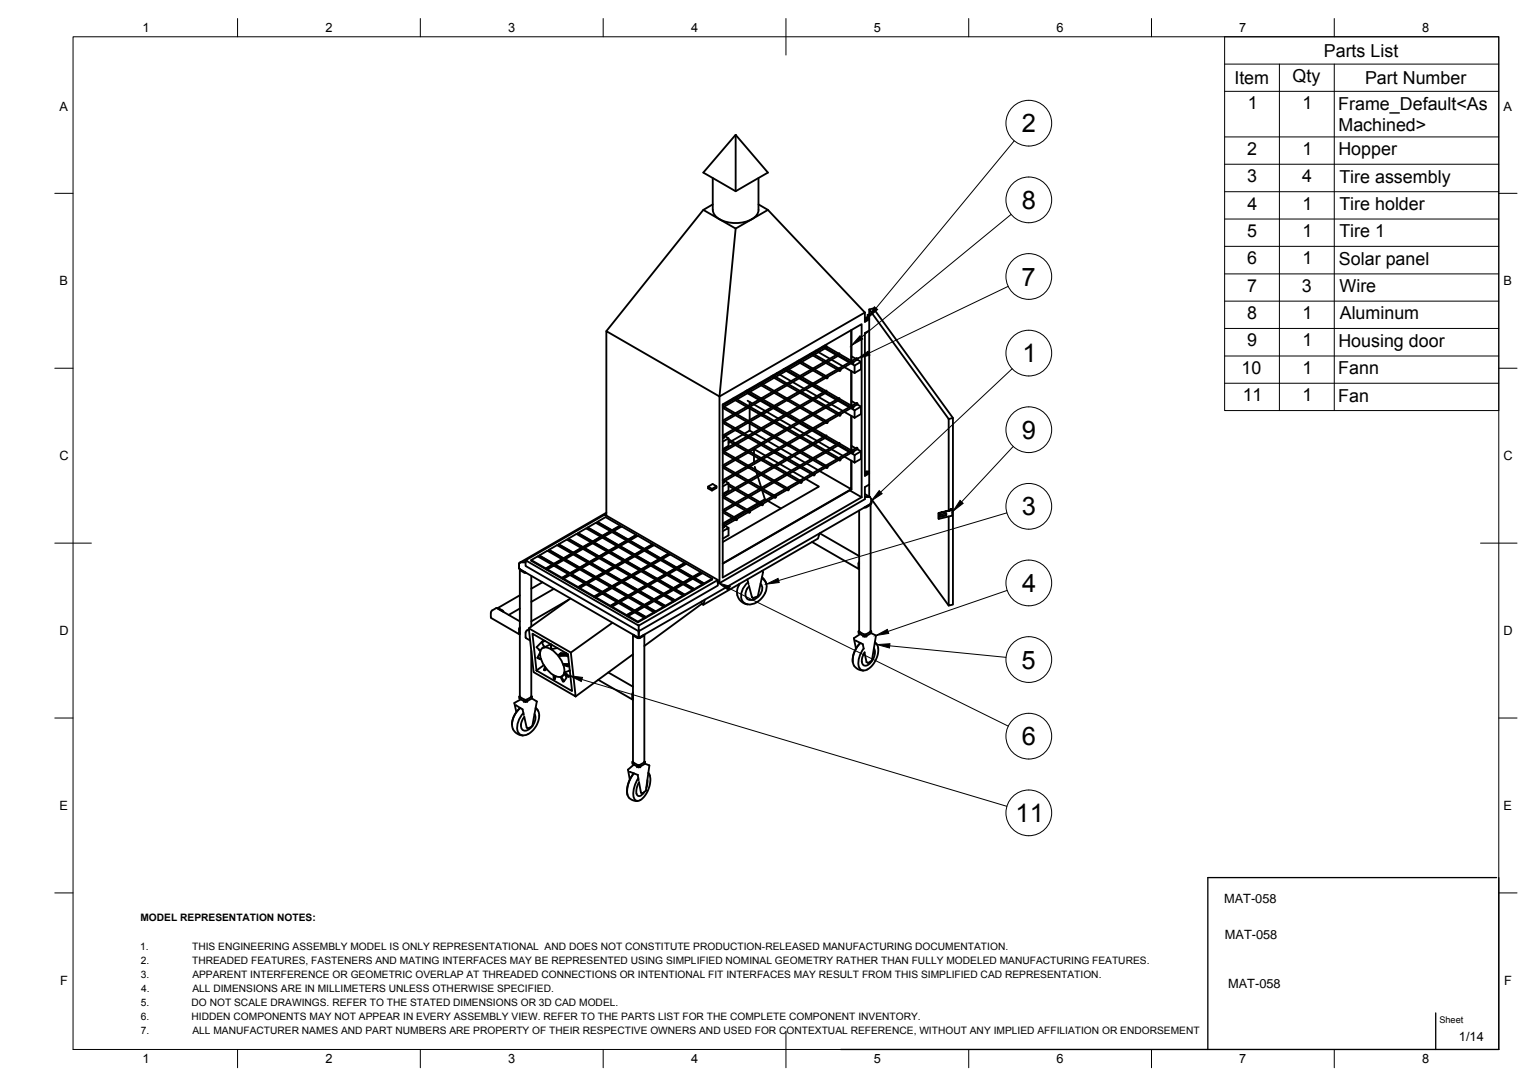
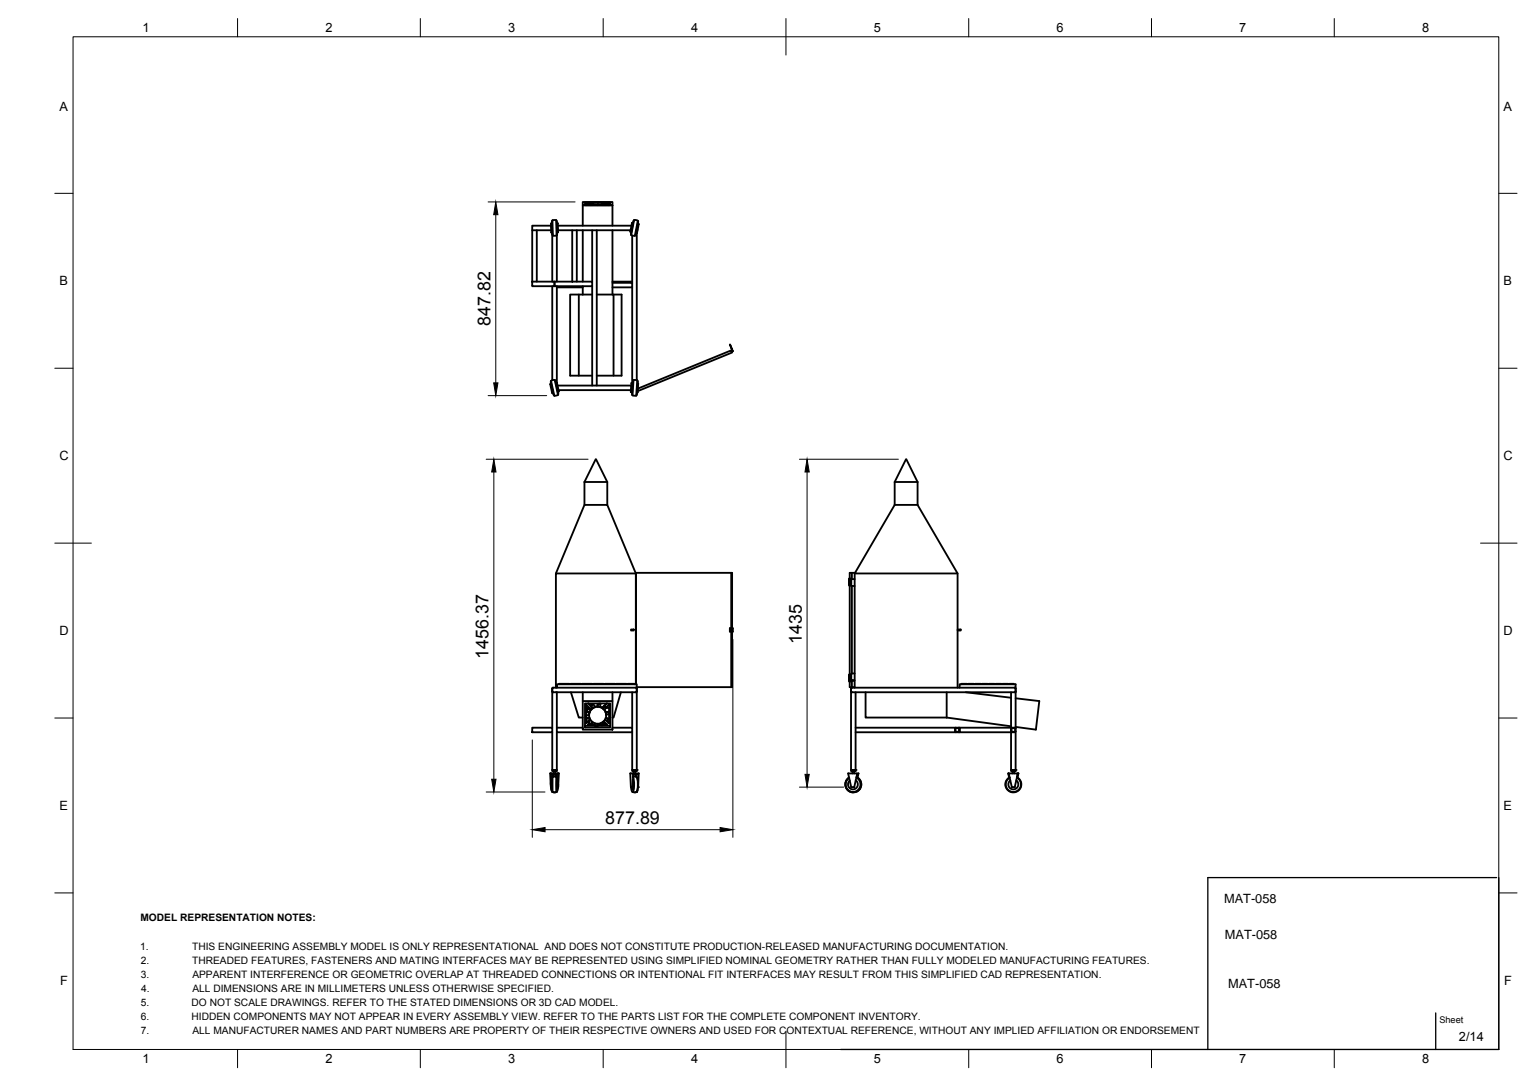
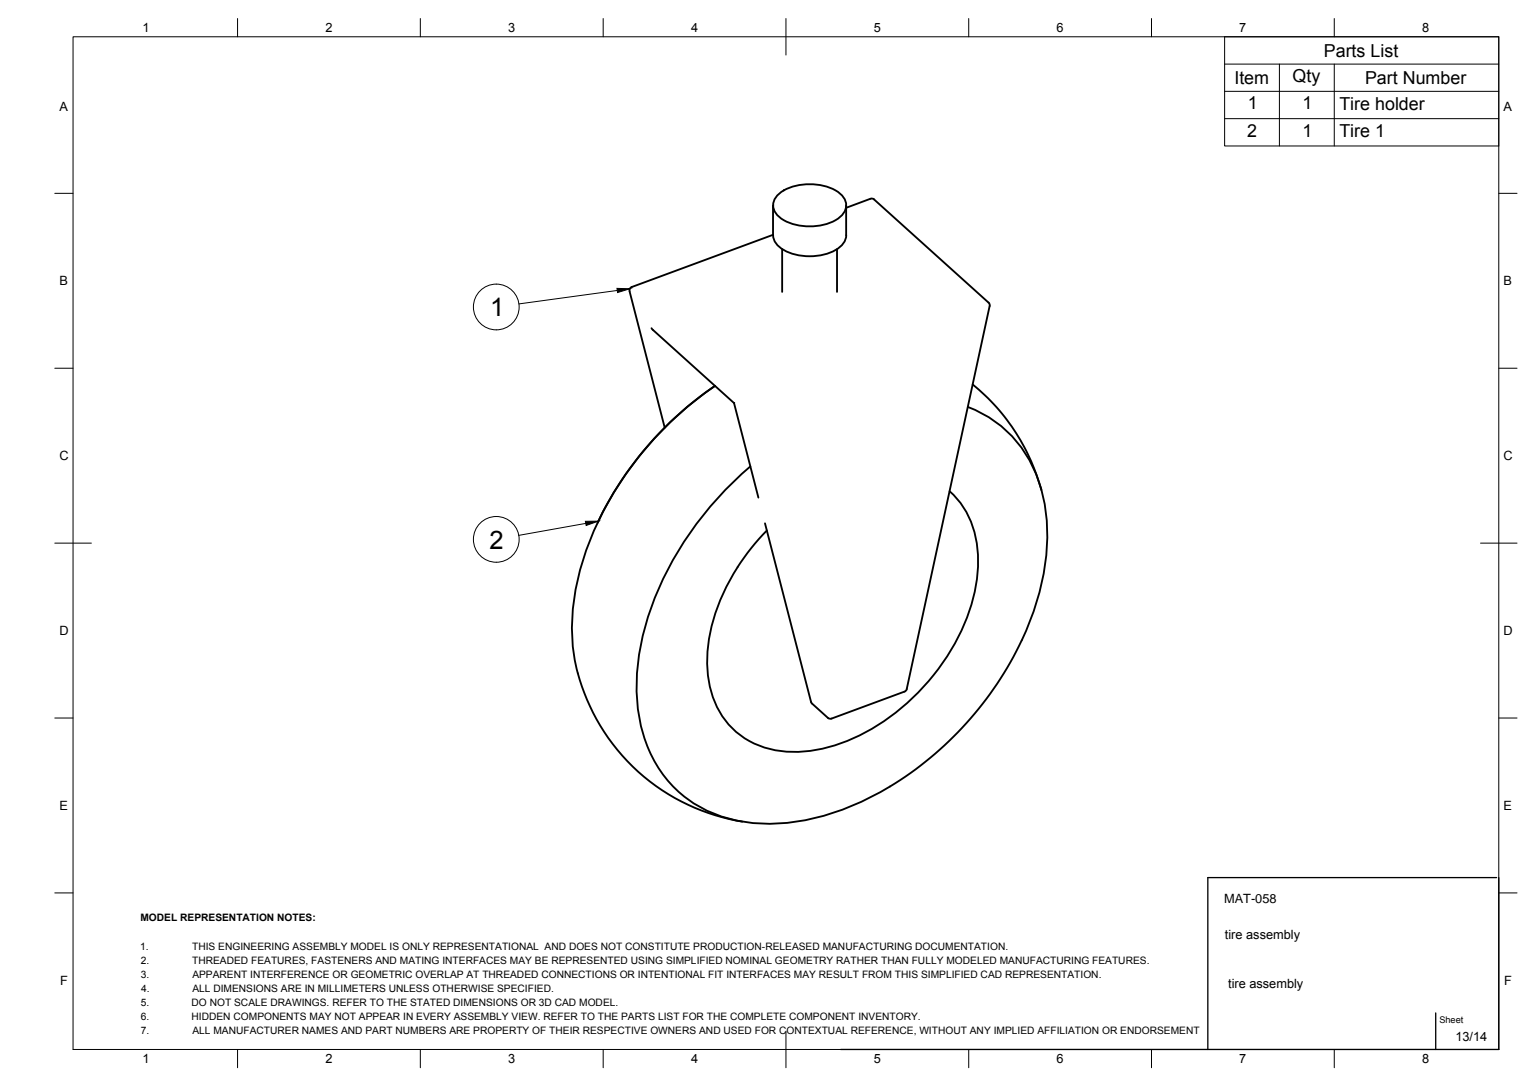
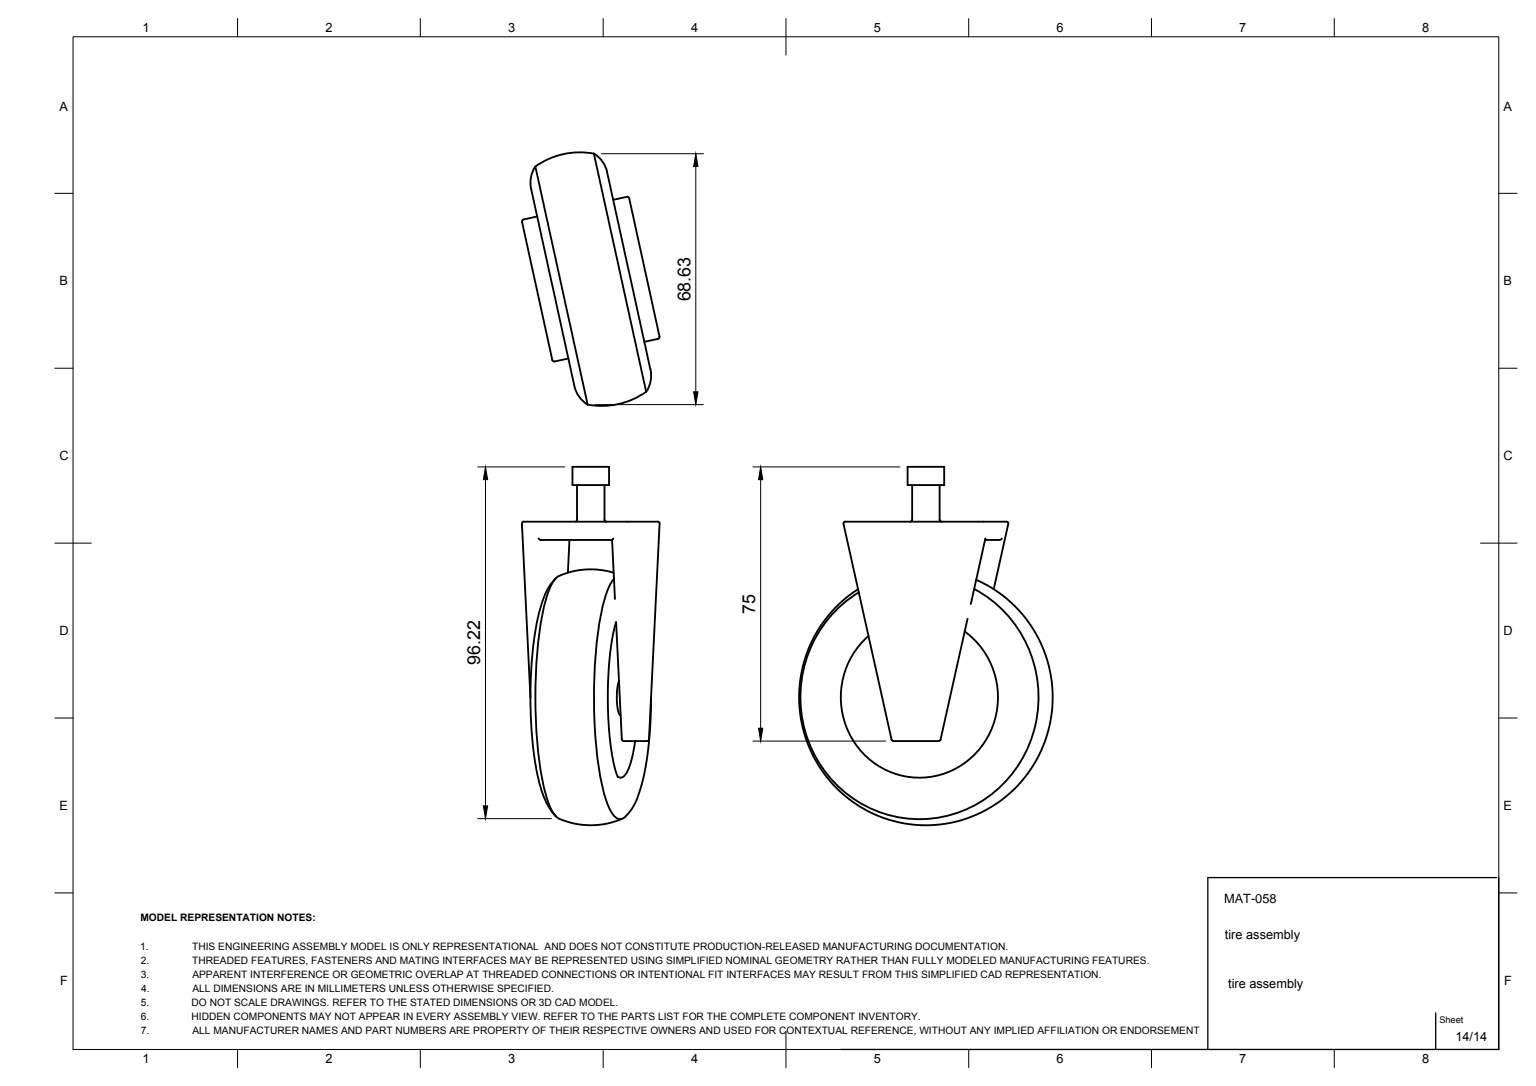
ISO-10303-21;
HEADER;
FILE_DESCRIPTION (('STEP AP214'),
    '1' );
FILE_NAME ('MAT-058',
    '2026-10-21T17:54:40',
    ( '' ),
    ( '' ),
    'SwSTEP 2.0',
    'SolidWorks 2026',
    '' );
FILE_SCHEMA (( 'AUTOMOTIVE_DESIGN' ));
ENDSEC;

DATA;
#1 = CARTESIAN_POINT ( 'NONE',  ( -0.3862712429686977478, 1.188820645368937390, -10.00000000000000000 ) ) ;
#2 = CIRCLE ( 'NONE', #7396, 2.000000000000001776 ) ;
#3 = ORIENTED_EDGE ( 'NONE', *, *, #134, .T. ) ;
#4 = FACE_OUTER_BOUND ( 'NONE', #5138, .T. ) ;
#5 = ORIENTED_EDGE ( 'NONE', *, *, #50322, .T. ) ;
#6 = ADVANCED_FACE ( 'NONE', ( #30321 ), #29814, .T. ) ;
#7 = ORIENTED_EDGE ( 'NONE', *, *, #34701, .F. ) ;
#8 = CARTESIAN_POINT ( 'NONE',  ( 341.9999999999999432, -181.0000000000001421, -349.9999999999998863 ) ) ;
#9 = DIRECTION ( 'NONE',  ( -1.000000000000000000, -0.000000000000000000, -0.000000000000000000 ) ) ;
#10 = ORIENTED_EDGE ( 'NONE', *, *, #50701, .F. ) ;
#11 = ORIENTED_EDGE ( 'NONE', *, *, #36636, .F. ) ;
#12 = EDGE_CURVE ( 'NONE', #49361, #27194, #1364, .T. ) ;
#13 = EDGE_CURVE ( 'NONE', #17667, #14780, #49006, .T. ) ;
#14 = ORIENTED_EDGE ( 'NONE', *, *, #5906, .T. ) ;
#15 = CARTESIAN_POINT ( 'NONE',  ( 71.55402655318505367, 1.025126265847089657, 79.06828755692797017 ) ) ;
#16 = DIRECTION ( 'NONE',  ( -1.000000000000000000, -0.000000000000000000, -0.000000000000000000 ) ) ;
#17 = ORIENTED_EDGE ( 'NONE', *, *, #15192, .T. ) ;
#18 = CARTESIAN_POINT ( 'NONE',  ( -1.011271242968683426, -0.7347315653655928092, 3.333333333333333481 ) ) ;
#19 = CARTESIAN_POINT ( 'NONE',  ( 42.78107912161490844, -16.56908454419397003, -9.367992836599951190 ) ) ;
#20 = EDGE_CURVE ( 'NONE', #23493, #39659, #10554, .T. ) ;
#21 = CARTESIAN_POINT ( 'NONE',  ( 191.5540265531851105, 0.000000000000000000, 162.5682875569279702 ) ) ;
#22 = ORIENTED_EDGE ( 'NONE', *, *, #35505, .T. ) ;
#23 = B_SPLINE_CURVE_WITH_KNOTS ( 'NONE', 3,
 ( #8249, #22875, #15684, #35464 ),
 .UNSPECIFIED., .F., .F.,
 ( 4, 4 ),
 ( 0.9895749839358303213, 1.000000000000000000 ),
 .UNSPECIFIED. ) ;
#24 = AXIS2_PLACEMENT_3D ( 'NONE', #27397, #19697, #35376 ) ;
#25 = FACE_OUTER_BOUND ( 'NONE', #19071, .T. ) ;
#26 = AXIS2_PLACEMENT_3D ( 'NONE', #26313, #42956, #39141 ) ;
#27 = VECTOR ( 'NONE', #2447, 1000.000000000000000 ) ;
#28 = EDGE_LOOP ( 'NONE', ( #27721, #41383, #11208, #21958 ) ) ;
#29 = CARTESIAN_POINT ( 'NONE',  ( 155.0540265531850537, 2.143131898507880377E-16, -37.43171244307205825 ) ) ;
#30 = DIRECTION ( 'NONE',  ( 0.000000000000000000, 0.000000000000000000, 1.000000000000000000 ) ) ;
#31 = ORIENTED_EDGE ( 'NONE', *, *, #39072, .F. ) ;
#32 = CARTESIAN_POINT ( 'NONE',  ( -24.39427009666018265, -44.07992421011638129, 8.807470649214879543 ) ) ;
#33 = VECTOR ( 'NONE', #35078, 1000.000000000000000 ) ;
#34 = AXIS2_PLACEMENT_3D ( 'NONE', #550, #47684, #4384 ) ;
#35 = CARTESIAN_POINT ( 'NONE',  ( 181.0000000000000284, -174.9999999999999716, -111.0000000000001563 ) ) ;
#36 = VERTEX_POINT ( 'NONE', #37038 ) ;
#37 = CARTESIAN_POINT ( 'NONE',  ( 38.06347959788622859, -17.13191708601470964, -8.080361901872240793 ) ) ;
#38 = FACE_OUTER_BOUND ( 'NONE', #34200, .T. ) ;
#39 = CARTESIAN_POINT ( 'NONE',  ( -48.44597344681495343, 0.000000000000000000, 159.0682875569279702 ) ) ;
#40 = VECTOR ( 'NONE', #48975, 1000.000000000000000 ) ;
#41 = DIRECTION ( 'NONE',  ( -1.000000000000000000, -0.000000000000000000, -0.000000000000000000 ) ) ;
#42 = EDGE_LOOP ( 'NONE', ( #31144, #13391, #8793, #47116, #38295 ) ) ;
#43 = FACE_OUTER_BOUND ( 'NONE', #38714, .T. ) ;
#44 = CARTESIAN_POINT ( 'NONE',  ( 45.64490844644691236, 21.32281559348795952, 8.807470649214879543 ) ) ;
#45 = LINE ( 'NONE', #24156, #46879 ) ;
#46 = ORIENTED_EDGE ( 'NONE', *, *, #39361, .F. ) ;
#47 = ADVANCED_FACE ( 'NONE', ( #25459 ), #1863, .T. ) ;
#48 = ORIENTED_EDGE ( 'NONE', *, *, #42434, .T. ) ;
#49 = PRODUCT_CONTEXT ( 'NONE', #18094, 'mechanical' ) ;
#50 = CARTESIAN_POINT ( 'NONE',  ( 112.2789002873379758, -1.749999999999996891, -80.20683870891909351 ) ) ;
#51 = CARTESIAN_POINT ( 'NONE',  ( -114.9999999999984652, 17.00000000000000000, 60.00000000000000000 ) ) ;
#52 =( LENGTH_UNIT ( ) NAMED_UNIT ( * ) SI_UNIT ( .MILLI., .METRE. ) );
#53 = DIRECTION ( 'NONE',  ( -1.000000000000000000, -0.000000000000000000, -0.000000000000000000 ) ) ;
#54 = CARTESIAN_POINT ( 'NONE',  ( -85.67084718096784002, 1.750000000000010214, -118.1565861772249519 ) ) ;
#55 = VERTEX_POINT ( 'NONE', #2115 ) ;
#56 = CARTESIAN_POINT ( 'NONE',  ( 47.23269937569327226, -16.43609759007049931, -2.408242355805840784 ) ) ;
#57 = LINE ( 'NONE', #42375, #32687 ) ;
#58 = CARTESIAN_POINT ( 'NONE',  ( 130.0000000000021032, 17.00000000000000000, 95.00000000000000000 ) ) ;
#59 = CARTESIAN_POINT ( 'NONE',  ( 164.9999999999999716, -174.9999999999999716, -340.0000000000001137 ) ) ;
#60 = AXIS2_PLACEMENT_3D ( 'NONE', #7908, #4040, #30745 ) ;
#61 = EDGE_LOOP ( 'NONE', ( #36555, #35091, #44528, #47513 ) ) ;
#62 = AXIS2_PLACEMENT_3D ( 'NONE', #28771, #36489, #21066 ) ;
#63 = ORIENTED_EDGE ( 'NONE', *, *, #25801, .F. ) ;
#64 = CYLINDRICAL_SURFACE ( 'NONE', #8155, 1.750000000000001554 ) ;
#65 = CARTESIAN_POINT ( 'NONE',  ( -0.3370904143228978245, 0.2449105217885259589, 10.00000000000000000 ) ) ;
#66 = ORIENTED_EDGE ( 'NONE', *, *, #13113, .F. ) ;
#67 = CARTESIAN_POINT ( 'NONE',  ( -12.78770032058971395, -31.68259716188267916, 7.455576670931136185 ) ) ;
#68 = CARTESIAN_POINT ( 'NONE',  ( 183.0000000000000000, 175.0000000000000284, -356.0000000000001705 ) ) ;
#69 = AXIS2_PLACEMENT_3D ( 'NONE', #31209, #39422, #27614 ) ;
#70 = AXIS2_PLACEMENT_3D ( 'NONE', #6927, #30792, #6416 ) ;
#71 = CARTESIAN_POINT ( 'NONE',  ( 10.30302290646030450, 13.08520913973580235, -9.683996418299976483 ) ) ;
#72 = LINE ( 'NONE', #42385, #35392 ) ;
#73 = EDGE_LOOP ( 'NONE', ( #24470, #20215, #48107, #6586 ) ) ;
#74 = CARTESIAN_POINT ( 'NONE',  ( 50.11058929355269953, -7.578863168071589662, 7.455576670931136185 ) ) ;
#75 = DIRECTION ( 'NONE',  ( 0.000000000000000000, 3.469446951953611033E-15, 1.000000000000000000 ) ) ;
#76 = VERTEX_POINT ( 'NONE', #17762 ) ;
#77 = LINE ( 'NONE', #43169, #13986 ) ;
#78 = DIRECTION ( 'NONE',  ( -0.000000000000000000, -0.000000000000000000, -1.000000000000000000 ) ) ;
#79 = DIRECTION ( 'NONE',  ( 0.000000000000000000, -1.000000000000000000, -3.186989995019654210E-49 ) ) ;
#80 = CARTESIAN_POINT ( 'NONE',  ( -10.00000000000000355, -34.54492135858216528, 5.000000000000000000 ) ) ;
#81 = EDGE_CURVE ( 'NONE', #16655, #7516, #13481, .T. ) ;
#82 = ORIENTED_EDGE ( 'NONE', *, *, #7839, .T. ) ;
#83 = ORIENTED_EDGE ( 'NONE', *, *, #42278, .F. ) ;
#84 = CARTESIAN_POINT ( 'NONE',  ( -0.8965959638259611841, -1.582931917743307215, 9.903764339332084887 ) ) ;
#85 = ORIENTED_EDGE ( 'NONE', *, *, #19964, .F. ) ;
#86 = CARTESIAN_POINT ( 'NONE',  ( 71.55402655318505367, 0.000000000000000000, 165.0000000000000000 ) ) ;
#87 = CARTESIAN_POINT ( 'NONE',  ( 355.9999999999999432, -181.0000000000001421, -349.9999999999999432 ) ) ;
#88 = DIRECTION ( 'NONE',  ( 1.121065046350011585E-16, 0.7071067811865475727, 0.7071067811865474617 ) ) ;
#89 = ORIENTED_EDGE ( 'NONE', *, *, #20681, .F. ) ;
#90 = CARTESIAN_POINT ( 'NONE',  ( 193.3040265531851105, 1.750000000000010658, 80.81828755692798438 ) ) ;
#91 = ORIENTED_EDGE ( 'NONE', *, *, #48428, .F. ) ;
#92 = EDGE_CURVE ( 'NONE', #33627, #36736, #41611, .T. ) ;
#93 = CARTESIAN_POINT ( 'NONE',  ( -32.43949840348904701, -7.871562655726274116, -9.367992836599954742 ) ) ;
#94 = EDGE_CURVE ( 'NONE', #19596, #23363, #2597, .T. ) ;
#95 = CARTESIAN_POINT ( 'NONE',  ( 111.5540265531850679, 0.000000000000000000, -77.43171244307204404 ) ) ;
#96 = CIRCLE ( 'NONE', #3362, 4.000000000000003553 ) ;
#97 = LINE ( 'NONE', #40110, #967 ) ;
#98 = AXIS2_PLACEMENT_3D ( 'NONE', #41759, #33325, #22512 ) ;
#99 = ORIENTED_EDGE ( 'NONE', *, *, #35916, .T. ) ;
#100 = EDGE_LOOP ( 'NONE', ( #22322, #8541, #32792, #19627 ) ) ;
#101 = ORIENTED_EDGE ( 'NONE', *, *, #35031, .T. ) ;
#102 = CARTESIAN_POINT ( 'NONE',  ( 1.011271242968688311, -0.7347315653655855927, 10.00000000000000000 ) ) ;
#103 = FACE_OUTER_BOUND ( 'NONE', #47648, .T. ) ;
#104 = CARTESIAN_POINT ( 'NONE',  ( -164.9459734468149463, 1.025126265847089435, -40.93171244307204404 ) ) ;
#105 = ORIENTED_EDGE ( 'NONE', *, *, #23023, .F. ) ;
#106 = CARTESIAN_POINT ( 'NONE',  ( -194.9999999999999432, 173.0000000000000000, 372.0000000000000000 ) ) ;
#107 = VECTOR ( 'NONE', #36359, 1000.000000000000000 ) ;
#108 = ADVANCED_FACE ( 'NONE', ( #42862 ), #18238, .T. ) ;
#109 = B_SPLINE_CURVE_WITH_KNOTS ( 'NONE', 3,
 ( #13337, #1308, #25156, #24903 ),
 .UNSPECIFIED., .F., .F.,
 ( 4, 4 ),
 ( 1.110764993427085326E-17, 0.002466147708923237519 ),
 .UNSPECIFIED. ) ;
#110 = ORIENTED_EDGE ( 'NONE', *, *, #46921, .F. ) ;
#111 = DIRECTION ( 'NONE',  ( 0.000000000000000000, -2.265761274745217480E-16, 1.000000000000000000 ) ) ;
#112 = ORIENTED_EDGE ( 'NONE', *, *, #36233, .F. ) ;
#113 = EDGE_CURVE ( 'NONE', #40036, #44970, #10285, .T. ) ;
#114 = CARTESIAN_POINT ( 'NONE',  ( 0.000000000000000000, 181.0000000000000284, -356.0000000000002274 ) ) ;
#115 = CARTESIAN_POINT ( 'NONE',  ( 24.39427009665985224, 44.07992421011656603, 8.807470649214879543 ) ) ;
#116 = PLANE ( 'NONE',  #46273 ) ;
#117 = CARTESIAN_POINT ( 'NONE',  ( 357.1715728752538439, -167.0000000000001137, 342.0000000000000000 ) ) ;
#118 = LINE ( 'NONE', #878, #10886 ) ;
#119 = ORIENTED_EDGE ( 'NONE', *, *, #13290, .T. ) ;
#120 = EDGE_LOOP ( 'NONE', ( #42684, #24578, #28599, #31905 ) ) ;
#121 = CARTESIAN_POINT ( 'NONE',  ( -114.9999999999978542, 17.00000000000000000, 95.00000000000000000 ) ) ;
#122 =( BOUNDED_CURVE ( )  B_SPLINE_CURVE ( 3, ( #11119, #46228, #4929, #44170 ),
 .UNSPECIFIED., .F., .F. ) 
 B_SPLINE_CURVE_WITH_KNOTS ( ( 4, 4 ),
 ( 0.000000000000000000, 1.570796326794896558 ),
 .UNSPECIFIED. ) 
 CURVE ( )  GEOMETRIC_REPRESENTATION_ITEM ( )  RATIONAL_B_SPLINE_CURVE ( ( 1.000000000000000000, 0.8047378541243649375, 0.8047378541243649375, 1.000000000000000000 ) ) 
 REPRESENTATION_ITEM ( '' )  );
#123 = DIRECTION ( 'NONE',  ( -0.000000000000000000, -1.000000000000000000, -0.000000000000000000 ) ) ;
#124 = DIRECTION ( 'NONE',  ( -0.000000000000000000, -0.000000000000000000, -1.000000000000000000 ) ) ;
#125 = CARTESIAN_POINT ( 'NONE',  ( -115.0000000000000284, 17.00000000000000000, -114.9999999999999858 ) ) ;
#126 = CARTESIAN_POINT ( 'NONE',  ( 168.9999999999999716, -272.4999999999999432, -359.9999999999999432 ) ) ;
#127 = ORIENTED_EDGE ( 'NONE', *, *, #28456, .T. ) ;
#128 = CARTESIAN_POINT ( 'NONE',  ( 355.9999999999999432, 174.9999999999996589, -356.0000000000003411 ) ) ;
#129 = CIRCLE ( 'NONE', #5860, 4.000000000000003553 ) ;
#130 = EDGE_CURVE ( 'NONE', #39856, #25517, #44158, .T. ) ;
#131 = DIRECTION ( 'NONE',  ( -1.000000000000000000, -1.156482317317870492E-16, 0.000000000000000000 ) ) ;
#132 = CIRCLE ( 'NONE', #9133, 37.50000000000000000 ) ;
#133 = ORIENTED_EDGE ( 'NONE', *, *, #48424, .F. ) ;
#134 = EDGE_CURVE ( 'NONE', #24013, #25229, #8136, .T. ) ;
#135 = EDGE_CURVE ( 'NONE', #16306, #8464, #38459, .T. ) ;
#136 = CARTESIAN_POINT ( 'NONE',  ( -127.7210997126620242, -1.749999999999996891, 119.7931612910809065 ) ) ;
#137 = FACE_OUTER_BOUND ( 'NONE', #38012, .T. ) ;
#138 = ADVANCED_FACE ( 'NONE', ( #43 ), #14562, .T. ) ;
#139 = ORIENTED_EDGE ( 'NONE', *, *, #39135, .F. ) ;
#140 = VECTOR ( 'NONE', #20878, 1000.000000000000000 ) ;
#141 = ORIENTED_EDGE ( 'NONE', *, *, #37641, .T. ) ;
#142 = CARTESIAN_POINT ( 'NONE',  ( 1.088201875076330705, 0.7239277119154168272, 9.945465949847356768 ) ) ;
#143 = ADVANCED_FACE ( 'NONE', ( #18750 ), #30578, .T. ) ;
#144 = FACE_OUTER_BOUND ( 'NONE', #19501, .T. ) ;
#145 = ORIENTED_EDGE ( 'NONE', *, *, #17426, .F. ) ;
#146 = ORIENTED_EDGE ( 'NONE', *, *, #12335, .F. ) ;
#147 = CARTESIAN_POINT ( 'NONE',  ( -44.94597344681493922, 2.143131898507880377E-16, -37.43171244307200141 ) ) ;
#148 = CARTESIAN_POINT ( 'NONE',  ( 35.51846793572394034, -35.99772139009119343, 7.906207997025717304 ) ) ;
#149 = CARTESIAN_POINT ( 'NONE',  ( -4.763548243873389154, 16.57409059453848599, 8.727788335465566760 ) ) ;
#150 = CARTESIAN_POINT ( 'NONE',  ( -14.99999999999876366, 17.00000000000000000, 30.00000000000000000 ) ) ;
#151 = ORIENTED_EDGE ( 'NONE', *, *, #46263, .F. ) ;
#152 = ORIENTED_EDGE ( 'NONE', *, *, #12710, .F. ) ;
#153 = ORIENTED_EDGE ( 'NONE', *, *, #11070, .T. ) ;
#154 = CARTESIAN_POINT ( 'NONE',  ( 2.188678504086826848, -0.3267089737525829540, 9.881002359080282460 ) ) ;
#155 = DIRECTION ( 'NONE',  ( 0.000000000000000000, 0.000000000000000000, 1.000000000000000000 ) ) ;
#156 = VERTEX_POINT ( 'NONE', #11065 ) ;
#157 = CARTESIAN_POINT ( 'NONE',  ( 1.249999999999999778, 0.000000000000000000, 3.333333333333333481 ) ) ;
#158 = CARTESIAN_POINT ( 'NONE',  ( 1.228394325311184421, -1.341866297401743235, 9.903764339332088440 ) ) ;
#159 = CARTESIAN_POINT ( 'NONE',  ( 73.30402655318508209, 1.750000000000010658, -119.1817124430720440 ) ) ;
#160 = ORIENTED_EDGE ( 'NONE', *, *, #20171, .T. ) ;
#161 = ORIENTED_EDGE ( 'NONE', *, *, #26521, .T. ) ;
#162 = LINE ( 'NONE', #15801, #49153 ) ;
#163 = CARTESIAN_POINT ( 'NONE',  ( -124.9459734468149463, 2.143131898507847836E-16, -120.9317124430720156 ) ) ;
#164 = AXIS2_PLACEMENT_3D ( 'NONE', #11516, #32040, #11769 ) ;
#165 = LINE ( 'NONE', #47317, #28159 ) ;
#166 = ORIENTED_EDGE ( 'NONE', *, *, #34974, .F. ) ;
#167 = EDGE_CURVE ( 'NONE', #5103, #46968, #26727, .T. ) ;
#168 = ADVANCED_FACE ( 'NONE', ( #34691 ), #50265, .F. ) ;
#169 = VERTEX_POINT ( 'NONE', #24652 ) ;
#170 = CARTESIAN_POINT ( 'NONE',  ( -0.3862712429686977478, 1.188820645368937390, -3.333333333333333481 ) ) ;
#171 = EDGE_LOOP ( 'NONE', ( #28708, #6316, #9774, #15681 ) ) ;
#172 = EDGE_CURVE ( 'NONE', #7661, #23271, #44918, .T. ) ;
#173 = CARTESIAN_POINT ( 'NONE',  ( 113.3040265531850537, 1.749999999999997113, 40.81828755692798438 ) ) ;
#174 = LINE ( 'NONE', #20666, #643 ) ;
#175 = CARTESIAN_POINT ( 'NONE',  ( 30.00000000000062172, 17.00000000000000000, -54.99999999999999289 ) ) ;
#176 = EDGE_CURVE ( 'NONE', #39875, #24207, #43623, .T. ) ;
#177 = VECTOR ( 'NONE', #3121, 1000.000000000000000 ) ;
#178 = CARTESIAN_POINT ( 'NONE',  ( 26.18032376592674737, -21.95228666728361233, 7.455576670931136185 ) ) ;
#179 = ORIENTED_EDGE ( 'NONE', *, *, #14430, .F. ) ;
#180 = ADVANCED_FACE ( 'NONE', ( #12327 ), #40546, .F. ) ;
#181 = CYLINDRICAL_SURFACE ( 'NONE', #33279, 4.000000000000003553 ) ;
#182 = ADVANCED_FACE ( 'NONE', ( #17198 ), #5386, .T. ) ;
#183 = DIRECTION ( 'NONE',  ( -1.000000000000000000, -0.000000000000000000, -0.000000000000000000 ) ) ;
#184 = CARTESIAN_POINT ( 'NONE',  ( 115.0540265531850395, 2.143131898507847836E-16, 42.56828755692795596 ) ) ;
#185 = CARTESIAN_POINT ( 'NONE',  ( 359.9999999999999432, -165.0000000000001137, -106.0000000000001990 ) ) ;
#186 = ORIENTED_EDGE ( 'NONE', *, *, #38813, .T. ) ;
#187 = CARTESIAN_POINT ( 'NONE',  ( 214.9999999999999432, 164.9999999999999716, 132.0000000000000000 ) ) ;
#188 = CARTESIAN_POINT ( 'NONE',  ( -49.46074318306826001, 9.578883844007169301, 8.807470649214879543 ) ) ;
#189 = EDGE_CURVE ( 'NONE', #37243, #19301, #48193, .T. ) ;
#190 = CARTESIAN_POINT ( 'NONE',  ( 151.5540265531850537, 1.025126265847089435, 39.06828755692797728 ) ) ;
#191 = ORIENTED_EDGE ( 'NONE', *, *, #24035, .F. ) ;
#192 = CARTESIAN_POINT ( 'NONE',  ( -88.44597344681497475, 0.000000000000000000, 122.5682875569279986 ) ) ;
#193 = EDGE_CURVE ( 'NONE', #28907, #37670, #20287, .T. ) ;
#194 = ADVANCED_FACE ( 'NONE', ( #21045 ), #12090, .T. ) ;
#195 = FACE_OUTER_BOUND ( 'NONE', #5721, .T. ) ;
#196 = VECTOR ( 'NONE', #29683, 1000.000000000000000 ) ;
#197 = ORIENTED_EDGE ( 'NONE', *, *, #48845, .F. ) ;
#198 = PLANE ( 'NONE',  #9790 ) ;
#199 = CYLINDRICAL_SURFACE ( 'NONE', #44476, 1.750000000000015543 ) ;
#200 = DIRECTION ( 'NONE',  ( -0.000000000000000000, -0.000000000000000000, 1.000000000000000000 ) ) ;
#201 = AXIS2_PLACEMENT_3D ( 'NONE', #39874, #40365, #36024 ) ;
#202 = ORIENTED_EDGE ( 'NONE', *, *, #48337, .T. ) ;
#203 = CARTESIAN_POINT ( 'NONE',  ( 349.9999999999999432, -168.9999999999999432, 339.9999999999997726 ) ) ;
#204 = ORIENTED_EDGE ( 'NONE', *, *, #887, .F. ) ;
#205 = ORIENTED_EDGE ( 'NONE', *, *, #34328, .T. ) ;
#206 = CARTESIAN_POINT ( 'NONE',  ( -46.69597344681494633, -1.750000000000010214, -39.18171244307202983 ) ) ;
#207 = DIRECTION ( 'NONE',  ( -3.469446951953610639E-15, 0.000000000000000000, 1.000000000000000000 ) ) ;
#208 = ORIENTED_EDGE ( 'NONE', *, *, #13614, .F. ) ;
#209 = VECTOR ( 'NONE', #36714, 1000.000000000000000 ) ;
#210 = CARTESIAN_POINT ( 'NONE',  ( 168.9999999999999716, 165.0000000000000000, -360.0000000000002274 ) ) ;
#211 = DIRECTION ( 'NONE',  ( -1.000000000000000000, 0.000000000000000000, 1.860490536778032451E-50 ) ) ;
#212 = ADVANCED_FACE ( 'NONE', ( #47688 ), #43368, .T. ) ;
#213 = CARTESIAN_POINT ( 'NONE',  ( -0.4830800013901715428, -1.200413232422907761, 9.947020512645419643 ) ) ;
#214 = VERTEX_POINT ( 'NONE', #5134 ) ;
#215 = DIRECTION ( 'NONE',  ( 0.000000000000000000, 3.186989995019654210E-49, 1.000000000000000000 ) ) ;
#216 = DIRECTION ( 'NONE',  ( 3.172065784643302499E-16, 1.000000000000000000, 0.000000000000000000 ) ) ;
#217 = DIRECTION ( 'NONE',  ( -1.000000000000000000, -0.000000000000000000, -0.000000000000000000 ) ) ;
#218 = VERTEX_POINT ( 'NONE', #20031 ) ;
#219 = CARTESIAN_POINT ( 'NONE',  ( 1.011271242968677653, 0.7347315653656002477, 10.00000000000000000 ) ) ;
#220 = CARTESIAN_POINT ( 'NONE',  ( 168.9999999999999716, 10.00000000000006395, 339.9999999999998295 ) ) ;
#221 = ORIENTED_EDGE ( 'NONE', *, *, #30959, .F. ) ;
#222 = EDGE_CURVE ( 'NONE', #31646, #38096, #39265, .T. ) ;
#223 = EDGE_LOOP ( 'NONE', ( #625, #40155, #13058, #17108 ) ) ;
#224 = ORIENTED_EDGE ( 'NONE', *, *, #7871, .F. ) ;
#225 = CARTESIAN_POINT ( 'NONE',  ( -1.365263087672800246, 0.5437404457009007430, 9.958264684458713489 ) ) ;
#226 = VECTOR ( 'NONE', #47044, 1000.000000000000000 ) ;
#227 = CARTESIAN_POINT ( 'NONE',  ( -0.9983599181300891745, -1.124146016603549070, 9.953784399990620813 ) ) ;
#228 = ORIENTED_EDGE ( 'NONE', *, *, #24802, .T. ) ;
#229 = CARTESIAN_POINT ( 'NONE',  ( -166.6959734468149463, -1.750000000000010658, -79.18171244307201562 ) ) ;
#230 = PLANE ( 'NONE',  #20488 ) ;
#231 = CARTESIAN_POINT ( 'NONE',  ( -44.99506233596264337, -23.32283626942287214, 7.455576670931136185 ) ) ;
#232 = ADVANCED_FACE ( 'NONE', ( #4388 ), #35956, .T. ) ;
#233 = CARTESIAN_POINT ( 'NONE',  ( 0.4166666666666669072, 0.000000000000000000, 10.00000000000000000 ) ) ;
#234 = DIRECTION ( 'NONE',  ( -0.8962124318248270161, 0.000000000000000000, 0.4436251537532894806 ) ) ;
#235 = ADVANCED_FACE ( 'NONE', ( #32351 ), #40053, .F. ) ;
#236 = DIRECTION ( 'NONE',  ( -0.000000000000000000, -1.000000000000000000, 2.537652627714643577E-15 ) ) ;
#237 = AXIS2_PLACEMENT_3D ( 'NONE', #8518, #24169, #12111 ) ;
#238 = CARTESIAN_POINT ( 'NONE',  ( -1.222012661920452326, 0.2471648704738776681, 9.981352469109934233 ) ) ;
#239 = CARTESIAN_POINT ( 'NONE',  ( -1.249999999999999778, 0.000000000000000000, 9.972675548442463622 ) ) ;
#240 = AXIS2_PLACEMENT_3D ( 'NONE', #22049, #38489, #34625 ) ;
#241 = CARTESIAN_POINT ( 'NONE',  ( -208.1473046169136580, -154.8119894309599260, 472.8425600500171981 ) ) ;
#242 = EDGE_CURVE ( 'NONE', #42713, #16089, #36464, .T. ) ;
#243 = DIRECTION ( 'NONE',  ( 1.000000000000000000, 0.000000000000000000, 0.000000000000000000 ) ) ;
#244 = PLANE ( 'NONE',  #29355 ) ;
#245 = VECTOR ( 'NONE', #20305, 1000.000000000000000 ) ;
#246 = EDGE_CURVE ( 'NONE', #20951, #20388, #31853, .T. ) ;
#247 = EDGE_CURVE ( 'NONE', #43286, #47057, #22018, .T. ) ;
#248 = LINE ( 'NONE', #3822, #36404 ) ;
#249 = CARTESIAN_POINT ( 'NONE',  ( -128.4459734468149179, 0.000000000000000000, -117.4317124430720725 ) ) ;
#250 = AXIS2_PLACEMENT_3D ( 'NONE', #2774, #2274, #17912 ) ;
#251 = DIRECTION ( 'NONE',  ( -1.000000000000000000, -0.000000000000000000, 9.251858538543084240E-16 ) ) ;
#252 = CARTESIAN_POINT ( 'NONE',  ( -86.69597344681494633, -1.750000000000009992, 0.8182875569279768335 ) ) ;
#253 = ORIENTED_EDGE ( 'NONE', *, *, #26936, .F. ) ;
#254 = DIRECTION ( 'NONE',  ( 0.000000000000000000, -1.000000000000000000, 0.000000000000000000 ) ) ;
#255 = EDGE_CURVE ( 'NONE', #50289, #1639, #37383, .T. ) ;
#256 = CARTESIAN_POINT ( 'NONE',  ( -14.52758583651993618, -8.922352469211071835, 8.953103998512858652 ) ) ;
#257 = LINE ( 'NONE', #31044, #20090 ) ;
#258 = CARTESIAN_POINT ( 'NONE',  ( 155.0540265531850537, 2.143131898507880377E-16, 165.0000000000000000 ) ) ;
#259 =( BOUNDED_CURVE ( )  B_SPLINE_CURVE ( 3, ( #2249, #37429, #6606, #3247 ),
 .UNSPECIFIED., .F., .F. ) 
 B_SPLINE_CURVE_WITH_KNOTS ( ( 4, 4 ),
 ( 1.570796326794896558, 3.141592653589793116 ),
 .UNSPECIFIED. ) 
 CURVE ( )  GEOMETRIC_REPRESENTATION_ITEM ( )  RATIONAL_B_SPLINE_CURVE ( ( 1.000000000000000000, 0.8047378541243649375, 0.8047378541243649375, 1.000000000000000000 ) ) 
 REPRESENTATION_ITEM ( '' )  );
#260 = ORIENTED_EDGE ( 'NONE', *, *, #20042, .T. ) ;
#261 = LINE ( 'NONE', #24365, #22339 ) ;
#262 = ORIENTED_EDGE ( 'NONE', *, *, #31509, .T. ) ;
#263 = FACE_OUTER_BOUND ( 'NONE', #4989, .T. ) ;
#264 = EDGE_LOOP ( 'NONE', ( #43850, #6676, #18926, #28305 ) ) ;
#265 = LINE ( 'NONE', #19995, #41034 ) ;
#266 = DIRECTION ( 'NONE',  ( 0.000000000000000000, 0.000000000000000000, 1.000000000000000000 ) ) ;
#267 =( BOUNDED_CURVE ( )  B_SPLINE_CURVE ( 3, ( #50247, #49055, #13937, #13448 ),
 .UNSPECIFIED., .F., .F. ) 
 B_SPLINE_CURVE_WITH_KNOTS ( ( 4, 4 ),
 ( 4.712388980384689674, 6.283185307179586232 ),
 .UNSPECIFIED. ) 
 CURVE ( )  GEOMETRIC_REPRESENTATION_ITEM ( )  RATIONAL_B_SPLINE_CURVE ( ( 1.000000000000000000, 0.8047378541243649375, 0.8047378541243649375, 1.000000000000000000 ) ) 
 REPRESENTATION_ITEM ( '' )  );
#268 = ORIENTED_EDGE ( 'NONE', *, *, #3344, .T. ) ;
#269 = VERTEX_POINT ( 'NONE', #28497 ) ;
#270 = ORIENTED_EDGE ( 'NONE', *, *, #36402, .F. ) ;
#271 = CARTESIAN_POINT ( 'NONE',  ( 71.55402655318506788, 0.000000000000000000, 162.5682875569279702 ) ) ;
#272 = DIRECTION ( 'NONE',  ( 0.000000000000000000, 0.000000000000000000, 1.000000000000000000 ) ) ;
#273 = VECTOR ( 'NONE', #4541, 1000.000000000000000 ) ;
#274 = ORIENTED_EDGE ( 'NONE', *, *, #2719, .F. ) ;
#275 = CARTESIAN_POINT ( 'NONE',  ( -84.94597344681493212, 1.025126265847089879, 122.5682875569280128 ) ) ;
#276 = CARTESIAN_POINT ( 'NONE',  ( 358.0000000000000000, -165.0000000000001137, -94.00000000000019895 ) ) ;
#277 = VECTOR ( 'NONE', #22809, 1000.000000000000000 ) ;
#278 = DIRECTION ( 'NONE',  ( 0.000000000000000000, 5.664403186863042467E-17, 1.000000000000000000 ) ) ;
#279 = ORIENTED_EDGE ( 'NONE', *, *, #33326, .F. ) ;
#280 = DIRECTION ( 'NONE',  ( 3.172065784643304472E-16, 1.000000000000000000, -1.710569414459005214E-49 ) ) ;
#281 = EDGE_CURVE ( 'NONE', #25566, #31089, #9489, .T. ) ;
#282 = DIRECTION ( 'NONE',  ( 0.000000000000000000, -0.000000000000000000, 1.000000000000000000 ) ) ;
#283 = ORIENTED_EDGE ( 'NONE', *, *, #247, .F. ) ;
#284 = AXIS2_PLACEMENT_3D ( 'NONE', #31805, #27184, #19732 ) ;
#285 = CARTESIAN_POINT ( 'NONE',  ( 37.27397286063867199, -4.111076158911552092, 7.697694107796188234 ) ) ;
#286 = EDGE_LOOP ( 'NONE', ( #4759, #15600, #2107, #33444, #6619, #35466, #25872, #11433 ) ) ;
#287 = DIRECTION ( 'NONE',  ( -0.000000000000000000, -1.000000000000000000, -0.000000000000000000 ) ) ;
#288 = CARTESIAN_POINT ( 'NONE',  ( -168.4459734468149463, 0.000000000000000000, 2.568287556927978166 ) ) ;
#289 = B_SPLINE_SURFACE_WITH_KNOTS ( 'NONE', 3, 3, ( 
 ( #36201, #41482, #14018, #25837 ),
 ( #10681, #49135, #24646, #8988 ),
 ( #37654, #47941, #16676, #34051 ),
 ( #45298, #29938, #45553, #6075 ) ),
 .UNSPECIFIED., .F., .F., .F.,
 ( 4, 4 ),
 ( 4, 4 ),
 ( 0.000000000000000000, 1.000000000000000000 ),
 ( 0.000000000000000000, 1.000000000000000000 ),
 .UNSPECIFIED. ) ;
#290 = VERTEX_POINT ( 'NONE', #6397 ) ;
#291 = CARTESIAN_POINT ( 'NONE',  ( 356.0000000000000000, -167.0000000000001137, -349.9999999999999432 ) ) ;
#292 = FACE_OUTER_BOUND ( 'NONE', #17808, .T. ) ;
#293 = LINE ( 'NONE', #43877, #10669 ) ;
#294 = CARTESIAN_POINT ( 'NONE',  ( 74.32915281903215998, -1.750000000000009548, -78.15658617722490931 ) ) ;
#295 = EDGE_CURVE ( 'NONE', #49251, #40145, #37979, .T. ) ;
#296 = EDGE_CURVE ( 'NONE', #47828, #22723, #5634, .T. ) ;
#297 = VERTEX_POINT ( 'NONE', #25154 ) ;
#298 = CARTESIAN_POINT ( 'NONE',  ( 0.3862712429686727678, 1.188820645368945605, -3.333333333333333481 ) ) ;
#299 = CARTESIAN_POINT ( 'NONE',  ( -0.1287570809895658697, 0.3962735484563123523, 10.00000000000000000 ) ) ;
#300 = EDGE_CURVE ( 'NONE', #33060, #42445, #25916, .T. ) ;
#301 = DIRECTION ( 'NONE',  ( 0.000000000000000000, 0.000000000000000000, -1.000000000000000000 ) ) ;
#302 = VERTEX_POINT ( 'NONE', #41553 ) ;
#303 = ORIENTED_EDGE ( 'NONE', *, *, #21142, .F. ) ;
#304 = EDGE_CURVE ( 'NONE', #27971, #25755, #44964, .T. ) ;
#305 = SHAPE_DEFINITION_REPRESENTATION ( #14247, #39915 ) ;
#306 = EDGE_CURVE ( 'NONE', #36749, #10540, #17931, .T. ) ;
#307 = CARTESIAN_POINT ( 'NONE',  ( 113.3040265531850537, -1.749999999999997335, -79.18171244307201562 ) ) ;
#308 = CARTESIAN_POINT ( 'NONE',  ( -3.975459390375366997, -0.2195152216756601216, -2.642742795433417058E-16 ) ) ;
#309 = CARTESIAN_POINT ( 'NONE',  ( 192.2789002873380184, 1.750000000000009548, 39.79316129108089228 ) ) ;
#310 = CIRCLE ( 'NONE', #31701, 4.000000000000003553 ) ;
#311 = VECTOR ( 'NONE', #35432, 1000.000000000000000 ) ;
#312 = CARTESIAN_POINT ( 'NONE',  ( -0.8433491450857070193, 0.9182416014173486740, 9.981352469109932457 ) ) ;
#313 = EDGE_LOOP ( 'NONE', ( #26683, #2356, #8405, #20446 ) ) ;
#314 = EDGE_CURVE ( 'NONE', #4361, #2042, #6678, .T. ) ;
#315 = CARTESIAN_POINT ( 'NONE',  ( 339.9999999999998863, -183.3431457505075741, 358.3431457505074036 ) ) ;
#316 = AXIS2_PLACEMENT_3D ( 'NONE', #35851, #27117, #42740 ) ;
#317 = DIRECTION ( 'NONE',  ( -0.000000000000000000, -0.000000000000000000, -1.000000000000000000 ) ) ;
#318 = PLANE ( 'NONE',  #3677 ) ;
#319 = VECTOR ( 'NONE', #21069, 1000.000000000000000 ) ;
#320 = CYLINDRICAL_SURFACE ( 'NONE', #46063, 1.750000000000015543 ) ;
#321 = ORIENTED_EDGE ( 'NONE', *, *, #26994, .T. ) ;
#322 = CARTESIAN_POINT ( 'NONE',  ( -128.4459734468149179, 0.000000000000000000, 165.0000000000000000 ) ) ;
#323 = VERTEX_POINT ( 'NONE', #49457 ) ;
#324 = CARTESIAN_POINT ( 'NONE',  ( 340.0000000000000000, 181.0000000000000568, 359.9999999999998295 ) ) ;
#325 = VERTEX_POINT ( 'NONE', #9998 ) ;
#326 = FACE_OUTER_BOUND ( 'NONE', #20541, .T. ) ;
#327 = DIRECTION ( 'NONE',  ( 1.000000000000000000, 0.000000000000000000, -0.000000000000000000 ) ) ;
#328 = CARTESIAN_POINT ( 'NONE',  ( 340.0000000000000568, 185.0000000000000284, 355.9999999999997726 ) ) ;
#329 = CARTESIAN_POINT ( 'NONE',  ( 191.5540265531850537, -1.025126265847089435, -157.4317124430720582 ) ) ;
#330 = ORIENTED_EDGE ( 'NONE', *, *, #46512, .T. ) ;
#331 = VECTOR ( 'NONE', #47511, 1000.000000000000000 ) ;
#332 = DIRECTION ( 'NONE',  ( 0.000000000000000000, -1.000000000000000000, 0.000000000000000000 ) ) ;
#333 = CARTESIAN_POINT ( 'NONE',  ( 355.9999999999999432, 185.0000000000002274, -360.0000000000003411 ) ) ;
#334 = ORIENTED_EDGE ( 'NONE', *, *, #5259, .T. ) ;
#335 = CARTESIAN_POINT ( 'NONE',  ( 7.937171537365877327, 0.3824377404836619698, 9.432811472610140413 ) ) ;
#336 = LINE ( 'NONE', #31644, #47492 ) ;
#337 = CARTESIAN_POINT ( 'NONE',  ( 0.000000000000000000, 0.000000000000000000, 910.0000000000000000 ) ) ;
#338 = EDGE_CURVE ( 'NONE', #17026, #45615, #13594, .T. ) ;
#339 = VERTEX_POINT ( 'NONE', #33870 ) ;
#340 = ORIENTED_EDGE ( 'NONE', *, *, #875, .T. ) ;
#341 = PLANE ( 'NONE',  #14465 ) ;
#342 = ADVANCED_FACE ( 'NONE', ( #29249, #10502, #26150 ), #6152, .F. ) ;
#343 = VERTEX_POINT ( 'NONE', #22300 ) ;
#344 = CARTESIAN_POINT ( 'NONE',  ( 36.97942854200454832, -6.226705766838405154, 8.914903342594563185 ) ) ;
#345 = DIRECTION ( 'NONE',  ( -1.000000000000000000, 0.000000000000000000, 0.000000000000000000 ) ) ;
#346 = VECTOR ( 'NONE', #39780, 1000.000000000000000 ) ;
#347 = VECTOR ( 'NONE', #5302, 1000.000000000000000 ) ;
#348 = DIRECTION ( 'NONE',  ( -1.000000000000000000, -0.000000000000000000, -0.000000000000000000 ) ) ;
#349 = EDGE_LOOP ( 'NONE', ( #28250, #8227, #4948, #139, #25034, #3385 ) ) ;
#350 = DIRECTION ( 'NONE',  ( -1.000000000000000000, -0.000000000000000000, -0.000000000000000000 ) ) ;
#351 = AXIS2_PLACEMENT_3D ( 'NONE', #22254, #34073, #6858 ) ;
#352 = ORIENTED_EDGE ( 'NONE', *, *, #46014, .T. ) ;
#353 = DIRECTION ( 'NONE',  ( 0.000000000000000000, 0.000000000000000000, 1.000000000000000000 ) ) ;
#354 = VECTOR ( 'NONE', #29219, 1000.000000000000000 ) ;
#355 = DIRECTION ( 'NONE',  ( 3.172065745548403743E-16, 1.000000000000000000, 0.000000000000000000 ) ) ;
#356 = DIRECTION ( 'NONE',  ( 0.000000000000000000, -1.000000000000000000, 0.000000000000000000 ) ) ;
#357 = VERTEX_POINT ( 'NONE', #3480 ) ;
#358 = ORIENTED_EDGE ( 'NONE', *, *, #25263, .T. ) ;
#359 = EDGE_LOOP ( 'NONE', ( #2759, #29859, #45477, #2453, #26930, #35930, #303, #44900 ) ) ;
#360 = DIRECTION ( 'NONE',  ( 0.000000000000000000, 0.000000000000000000, 1.000000000000000000 ) ) ;
#361 = CARTESIAN_POINT ( 'NONE',  ( -84.94597344681493212, -1.025126265847088991, 159.0682875569279418 ) ) ;
#362 = CARTESIAN_POINT ( 'NONE',  ( -29.18392875402943432, -17.44843138996582965, 7.906207997025717304 ) ) ;
#363 = ORIENTED_EDGE ( 'NONE', *, *, #44882, .T. ) ;
#364 = FACE_OUTER_BOUND ( 'NONE', #38900, .T. ) ;
#365 = ORIENTED_EDGE ( 'NONE', *, *, #8301, .F. ) ;
#366 = DIRECTION ( 'NONE',  ( 1.000000000000000000, 0.000000000000000000, 0.000000000000000000 ) ) ;
#367 = ORIENTED_EDGE ( 'NONE', *, *, #18075, .F. ) ;
#368 = CARTESIAN_POINT ( 'NONE',  ( -126.6959734468149321, -1.749999999999997335, 80.81828755692798438 ) ) ;
#369 = CARTESIAN_POINT ( 'NONE',  ( -225.0000000000000568, -165.6999999999999602, 254.8599999999999852 ) ) ;
#370 = CARTESIAN_POINT ( 'NONE',  ( 356.0000000000000000, 175.0000000000000284, -108.0000000000002132 ) ) ;
#371 = VECTOR ( 'NONE', #12956, 1000.000000000000000 ) ;
#372 = CARTESIAN_POINT ( 'NONE',  ( 185.0000000000000000, -93.49999999999998579, -350.0000000000001705 ) ) ;
#373 = LINE ( 'NONE', #27571, #20702 ) ;
#374 = EDGE_LOOP ( 'NONE', ( #37007, #35684, #23876, #49067, #24411 ) ) ;
#375 = VERTEX_POINT ( 'NONE', #32866 ) ;
#376 = EDGE_CURVE ( 'NONE', #35109, #22226, #31907, .T. ) ;
#377 = DIRECTION ( 'NONE',  ( 0.000000000000000000, -0.000000000000000000, -1.000000000000000000 ) ) ;
#378 = CARTESIAN_POINT ( 'NONE',  ( 0.5000000000000000000, -0.5000000000000000000, 1000.000000000000000 ) ) ;
#379 = FACE_OUTER_BOUND ( 'NONE', #33356, .T. ) ;
#380 = CARTESIAN_POINT ( 'NONE',  ( 0.000000000000000000, -165.1999999999999602, 340.1999999999997044 ) ) ;
#381 = AXIS2_PLACEMENT_3D ( 'NONE', #4181, #15227, #23679 ) ;
#382 = CARTESIAN_POINT ( 'NONE',  ( 195.0540265531851105, 2.143131898507880377E-16, 79.06828755692797017 ) ) ;
#383 = ORIENTED_EDGE ( 'NONE', *, *, #37796, .F. ) ;
#384 = VECTOR ( 'NONE', #28524, 1000.000000000000000 ) ;
#385 = DIRECTION ( 'NONE',  ( 0.000000000000000000, -1.000000000000000000, 0.000000000000000000 ) ) ;
#386 = CARTESIAN_POINT ( 'NONE',  ( 0.000000000000000000, 0.000000000000000000, 910.0000000000000000 ) ) ;
#387 = VERTEX_POINT ( 'NONE', #1801 ) ;
#388 = CARTESIAN_POINT ( 'NONE',  ( 8.277096487746778308, -33.14818118907697198, 7.455576670931136185 ) ) ;
#389 = DIRECTION ( 'NONE',  ( 0.000000000000000000, 0.000000000000000000, 1.000000000000000000 ) ) ;
#390 = DIRECTION ( 'NONE',  ( 0.000000000000000000, -2.265761274745217480E-16, 1.000000000000000000 ) ) ;
#391 = ORIENTED_EDGE ( 'NONE', *, *, #26509, .F. ) ;
#392 = PRODUCT_DEFINITION_SHAPE ( 'NONE', 'NONE',  #50736 ) ;
#393 = ORIENTED_EDGE ( 'NONE', *, *, #8336, .F. ) ;
#394 = CARTESIAN_POINT ( 'NONE',  ( 153.3040265531850537, 1.750000000000010658, 80.81828755692798438 ) ) ;
#395 = CARTESIAN_POINT ( 'NONE',  ( 23.82716369509147825, 44.49195112876006419, 8.356839323120299312 ) ) ;
#396 = AXIS2_PLACEMENT_3D ( 'NONE', #30919, #46501, #11395 ) ;
#397 = EDGE_LOOP ( 'NONE', ( #43742, #46810, #26881 ) ) ;
#398 = ORIENTED_EDGE ( 'NONE', *, *, #44450, .F. ) ;
#399 = CARTESIAN_POINT ( 'NONE',  ( 343.9999999999999432, 174.9999999999996589, -360.0000000000003411 ) ) ;
#400 = CARTESIAN_POINT ( 'NONE',  ( -3.229232847726260403, 16.57333684275945629, 9.178419661560148768 ) ) ;
#401 = CYLINDRICAL_SURFACE ( 'NONE', #39045, 4.000000000000003553 ) ;
#402 = DIRECTION ( 'NONE',  ( 1.000000000000000000, -4.105366553918459587E-48, -1.586032880504786307E-16 ) ) ;
#403 = EDGE_LOOP ( 'NONE', ( #46548, #45741, #3676, #28607 ) ) ;
#404 = AXIS2_PLACEMENT_3D ( 'NONE', #20557, #28515, #1323 ) ;
#405 = VERTEX_POINT ( 'NONE', #29501 ) ;
#406 = ORIENTED_EDGE ( 'NONE', *, *, #20191, .F. ) ;
#407 = DIRECTION ( 'NONE',  ( -0.000000000000000000, -0.000000000000000000, -1.000000000000000000 ) ) ;
#408 = EDGE_LOOP ( 'NONE', ( #49712, #23075, #15648, #3432 ) ) ;
#409 = DIRECTION ( 'NONE',  ( 1.000000000000000000, 0.000000000000000000, 0.000000000000000000 ) ) ;
#410 = PLANE ( 'NONE',  #69 ) ;
#411 = ORIENTED_EDGE ( 'NONE', *, *, #49299, .F. ) ;
#412 = ORIENTED_EDGE ( 'NONE', *, *, #15278, .F. ) ;
#413 = CARTESIAN_POINT ( 'NONE',  ( -126.6959734468149321, -1.749999999999997113, -39.18171244307202983 ) ) ;
#414 = CARTESIAN_POINT ( 'NONE',  ( 6.174150299305392053, -50.00000000000000711, 8.807470649214879543 ) ) ;
#415 =( BOUNDED_CURVE ( )  B_SPLINE_CURVE ( 3, ( #5683, #44416, #25963, #48241 ),
 .UNSPECIFIED., .F., .F. ) 
 B_SPLINE_CURVE_WITH_KNOTS ( ( 4, 4 ),
 ( 4.712388980384689674, 6.283185307179586232 ),
 .UNSPECIFIED. ) 
 CURVE ( )  GEOMETRIC_REPRESENTATION_ITEM ( )  RATIONAL_B_SPLINE_CURVE ( ( 1.000000000000000000, 0.8047378541243649375, 0.8047378541243649375, 1.000000000000000000 ) ) 
 REPRESENTATION_ITEM ( '' )  );
#416 = CARTESIAN_POINT ( 'NONE',  ( 344.0000000000000000, 165.0000000000000000, -90.00000000000018474 ) ) ;
#417 = ORIENTED_EDGE ( 'NONE', *, *, #25940, .F. ) ;
#418 = VERTEX_POINT ( 'NONE', #45117 ) ;
#419 = DIRECTION ( 'NONE',  ( -0.000000000000000000, -0.000000000000000000, -1.000000000000000000 ) ) ;
#420 = SURFACE_SIDE_STYLE ('',( #36087 ) ) ;
#421 = ORIENTED_EDGE ( 'NONE', *, *, #38475, .T. ) ;
#422 = DIRECTION ( 'NONE',  ( 0.000000000000000000, -1.000000000000000000, 1.822804496942679766E-16 ) ) ;
#423 = CARTESIAN_POINT ( 'NONE',  ( -47.72109971266203132, 1.750000000000010436, 119.7931612910808781 ) ) ;
#424 = LINE ( 'NONE', #28123, #46558 ) ;
#425 = CYLINDRICAL_SURFACE ( 'NONE', #22465, 1.750000000000001554 ) ;
#426 = ORIENTED_EDGE ( 'NONE', *, *, #295, .T. ) ;
#427 = EDGE_CURVE ( 'NONE', #32721, #15345, #25659, .T. ) ;
#428 = PLANE ( 'NONE',  #26708 ) ;
#429 = DIRECTION ( 'NONE',  ( -1.000000000000000000, 0.000000000000000000, 0.000000000000000000 ) ) ;
#430 = LINE ( 'NONE', #46568, #36748 ) ;
#431 = EDGE_CURVE ( 'NONE', #16089, #12079, #28992, .T. ) ;
#432 = DIRECTION ( 'NONE',  ( -1.000000000000000000, 1.331116318405244905E-23, 4.755310728521421461E-16 ) ) ;
#433 = ADVANCED_FACE ( 'NONE', ( #33614 ), #49204, .F. ) ;
#434 = VECTOR ( 'NONE', #13236, 1000.000000000000000 ) ;
#435 = APPLICATION_CONTEXT ( 'automotive_design' ) ;
#436 = AXIS2_PLACEMENT_3D ( 'NONE', #25349, #45321, #26098 ) ;
#437 = ADVANCED_FACE ( 'NONE', ( #14088 ), #48694, .T. ) ;
#438 = FACE_OUTER_BOUND ( 'NONE', #43936, .T. ) ;
#439 = DIRECTION ( 'NONE',  ( -1.586032892321652236E-16, -1.000000000000000000, -6.853681917100419162E-49 ) ) ;
#440 = EDGE_CURVE ( 'NONE', #43432, #19548, #26025, .T. ) ;
#441 = ORIENTED_EDGE ( 'NONE', *, *, #33733, .F. ) ;
#442 = LINE ( 'NONE', #685, #41199 ) ;
#443 = VECTOR ( 'NONE', #3485, 1000.000000000000000 ) ;
#444 = FACE_OUTER_BOUND ( 'NONE', #40389, .T. ) ;
#445 = CIRCLE ( 'NONE', #40629, 2.000000000000001776 ) ;
#446 = ORIENTED_EDGE ( 'NONE', *, *, #24923, .F. ) ;
#447 = CARTESIAN_POINT ( 'NONE',  ( 35.05402655318504657, 2.143131898507880377E-16, 42.56828755692798438 ) ) ;
#448 = DIRECTION ( 'NONE',  ( 0.000000000000000000, 0.000000000000000000, 1.000000000000000000 ) ) ;
#449 = VERTEX_POINT ( 'NONE', #669 ) ;
#450 = PRODUCT_DEFINITION_FORMATION_WITH_SPECIFIED_SOURCE ( 'ANY', '', #29832, .NOT_KNOWN. ) ;
#451 = CARTESIAN_POINT ( 'NONE',  ( -5.647304616913629616, 54.43801056904005975, 22.84256005001721945 ) ) ;
#452 = ADVANCED_FACE ( 'NONE', ( #16069 ), #23519, .T. ) ;
#454 = ORIENTED_EDGE ( 'NONE', *, *, #15929, .F. ) ;
#453 = EDGE_CURVE ( 'NONE', #46359, #24983, #8124, .T. ) ;
#455 = EDGE_LOOP ( 'NONE', ( #22398, #42737, #33219, #30241 ) ) ;
#456 = CARTESIAN_POINT ( 'NONE',  ( 33.08717642956892746, 5.870837526465160217, -8.016098858316199838 ) ) ;
#457 = CARTESIAN_POINT ( 'NONE',  ( 153.2026953830863647, 69.44873401059479079, -93.79675437945476801 ) ) ;
#458 = EDGE_CURVE ( 'NONE', #40596, #15960, #31982, .T. ) ;
#459 = EDGE_CURVE ( 'NONE', #16448, #40222, #8626, .T. ) ;
#460 = ORIENTED_EDGE ( 'NONE', *, *, #7056, .F. ) ;
#461 = DIRECTION ( 'NONE',  ( -1.000000000000000000, -0.000000000000000000, -0.000000000000000000 ) ) ;
#462 = LINE ( 'NONE', #35873, #24910 ) ;
#463 = ORIENTED_EDGE ( 'NONE', *, *, #39701, .T. ) ;
#464 = EDGE_CURVE ( 'NONE', #48470, #25557, #25629, .T. ) ;
#465 = ADVANCED_FACE ( 'NONE', ( #19658 ), #39933, .F. ) ;
#466 = DIRECTION ( 'NONE',  ( 0.000000000000000000, 0.000000000000000000, 1.000000000000000000 ) ) ;
#467 = ORIENTED_EDGE ( 'NONE', *, *, #8643, .T. ) ;
#468 = CARTESIAN_POINT ( 'NONE',  ( -9.998889670239194061, -0.1490146381531308739, 9.282506307616474217 ) ) ;
#469 = CARTESIAN_POINT ( 'NONE',  ( 135.0000000000015632, 17.00000000000000000, 35.00000000000000000 ) ) ;
#470 = AXIS2_PLACEMENT_3D ( 'NONE', #3136, #22152, #46465 ) ;
#471 = ORIENTED_EDGE ( 'NONE', *, *, #17428, .F. ) ;
#472 = CYLINDRICAL_SURFACE ( 'NONE', #11197, 1.750000000000008438 ) ;
#473 = CARTESIAN_POINT ( 'NONE',  ( 355.9999999999999432, -185.0000000000001421, 360.0000000000000000 ) ) ;
#474 = ORIENTED_EDGE ( 'NONE', *, *, #34538, .F. ) ;
#475 = AXIS2_PLACEMENT_3D ( 'NONE', #19383, #34284, #35070 ) ;
#476 = ORIENTED_EDGE ( 'NONE', *, *, #29069, .T. ) ;
#477 = ORIENTED_EDGE ( 'NONE', *, *, #9884, .T. ) ;
#478 = CARTESIAN_POINT ( 'NONE',  ( -34.38425513258694366, 36.82177522737846687, 8.807470649214879543 ) ) ;
#479 = AXIS2_PLACEMENT_3D ( 'NONE', #48205, #1053, #44377 ) ;
#480 = PLANE ( 'NONE',  #30774 ) ;
#481 = ORIENTED_EDGE ( 'NONE', *, *, #5333, .T. ) ;
#482 = EDGE_CURVE ( 'NONE', #50669, #27161, #35845, .T. ) ;
#483 = CARTESIAN_POINT ( 'NONE',  ( -26.18032376592659105, 21.95228666728381128, 7.455576670931136185 ) ) ;
#484 = DIRECTION ( 'NONE',  ( 0.1191452206184307472, 0.000000000000000000, -0.9928768384869219865 ) ) ;
#485 = DIRECTION ( 'NONE',  ( -0.000000000000000000, -0.000000000000000000, -1.000000000000000000 ) ) ;
#486 = EDGE_CURVE ( 'NONE', #24711, #40831, #43254, .T. ) ;
#487 = CARTESIAN_POINT ( 'NONE',  ( -6.174150299305392053, 50.00000000000000711, 8.807470649214879543 ) ) ;
#488 = CARTESIAN_POINT ( 'NONE',  ( -87.72109971266203843, -1.750000000000009548, 159.7931612910809065 ) ) ;
#489 = EDGE_CURVE ( 'NONE', #13008, #49667, #30971, .T. ) ;
#490 = CARTESIAN_POINT ( 'NONE',  ( 2.462075149652696027, -16.57295996686994499, 9.403735324607438884 ) ) ;
#491 = AXIS2_PLACEMENT_3D ( 'NONE', #861, #24715, #16507 ) ;
#492 = DIRECTION ( 'NONE',  ( 1.000000000000000000, 0.000000000000000000, 0.000000000000000000 ) ) ;
#493 = PRESENTATION_STYLE_ASSIGNMENT (( #23834 ) ) ;
#494 = CARTESIAN_POINT ( 'NONE',  ( 1.578643388466006714, -1.550786058692517511, 9.881002359080275355 ) ) ;
#495 = DIRECTION ( 'NONE',  ( 0.000000000000000000, 2.537652627714642000E-15, 1.000000000000000000 ) ) ;
#496 = CARTESIAN_POINT ( 'NONE',  ( 0.2773062244624638351, -1.251557370488896481, 9.948547179989619238 ) ) ;
#497 = AXIS2_PLACEMENT_3D ( 'NONE', #34833, #26856, #31230 ) ;
#498 = EDGE_CURVE ( 'NONE', #19922, #10844, #20629, .T. ) ;
#499 = VECTOR ( 'NONE', #28091, 1000.000000000000000 ) ;
#500 = PLANE ( 'NONE',  #17515 ) ;
#501 = CARTESIAN_POINT ( 'NONE',  ( 359.9999999999999432, -181.0000000000001137, -356.0000000000003411 ) ) ;
#502 =( BOUNDED_CURVE ( )  B_SPLINE_CURVE ( 3, ( #2955, #14255, #29915, #26067 ),
 .UNSPECIFIED., .F., .F. ) 
 B_SPLINE_CURVE_WITH_KNOTS ( ( 4, 4 ),
 ( 1.570796326794896558, 3.141592653589793116 ),
 .UNSPECIFIED. ) 
 CURVE ( )  GEOMETRIC_REPRESENTATION_ITEM ( )  RATIONAL_B_SPLINE_CURVE ( ( 1.000000000000000000, 0.8047378541243649375, 0.8047378541243649375, 1.000000000000000000 ) ) 
 REPRESENTATION_ITEM ( '' )  );
#503 = CARTESIAN_POINT ( 'NONE',  ( 35.00000000000186162, 17.00000000000000000, 90.00000000000000000 ) ) ;
#504 = CARTESIAN_POINT ( 'NONE',  ( 343.9999999999999432, 165.0000000000000000, -108.0000000000002132 ) ) ;
#505 = ORIENTED_EDGE ( 'NONE', *, *, #34410, .F. ) ;
#506 = CARTESIAN_POINT ( 'NONE',  ( 193.3040265531851105, 1.750000000000010658, -119.1817124430720440 ) ) ;
#507 = CARTESIAN_POINT ( 'NONE',  ( 113.3040265531850537, -1.749999999999996891, 160.8182875569279702 ) ) ;
#508 = CARTESIAN_POINT ( 'NONE',  ( -49.46074318306826001, 9.578883844007169301, 8.807470649214879543 ) ) ;
#509 = ADVANCED_FACE ( 'NONE', ( #12210 ), #8377, .F. ) ;
#510 = ORIENTED_EDGE ( 'NONE', *, *, #27958, .F. ) ;
#511 = FACE_OUTER_BOUND ( 'NONE', #39266, .T. ) ;
#512 = ORIENTED_EDGE ( 'NONE', *, *, #25092, .T. ) ;
#513 = LINE ( 'NONE', #24116, #49110 ) ;
#514 = EDGE_CURVE ( 'NONE', #45973, #15209, #36212, .T. ) ;
#515 = AXIS2_PLACEMENT_3D ( 'NONE', #26720, #30070, #30315 ) ;
#516 = B_SPLINE_CURVE_WITH_KNOTS ( 'NONE', 3,
 ( #27272, #33769, #31384, #8032 ),
 .UNSPECIFIED., .F., .F.,
 ( 4, 4 ),
 ( 3.824349771687705441E-16, 0.009762429746916051129 ),
 .UNSPECIFIED. ) ;
#517 = ORIENTED_EDGE ( 'NONE', *, *, #29930, .T. ) ;
#518 = CARTESIAN_POINT ( 'NONE',  ( -239.0000000000000853, -165.6999999999999602, 254.8599999999999852 ) ) ;
#519 = CARTESIAN_POINT ( 'NONE',  ( 191.5540265531851105, 0.000000000000000000, -77.43171244307204404 ) ) ;
#520 = CARTESIAN_POINT ( 'NONE',  ( 111.5540265531850537, 1.025126265847081886, -120.9317124430720440 ) ) ;
#521 = ORIENTED_EDGE ( 'NONE', *, *, #27225, .F. ) ;
#522 = LINE ( 'NONE', #27456, #25721 ) ;
#523 = ORIENTED_EDGE ( 'NONE', *, *, #44396, .T. ) ;
#524 = CIRCLE ( 'NONE', #29193, 2.000000000000001776 ) ;
#525 = EDGE_CURVE ( 'NONE', #17682, #46476, #42731, .T. ) ;
#526 = ADVANCED_FACE ( 'NONE', ( #38927 ), #19406, .T. ) ;
#527 = ORIENTED_EDGE ( 'NONE', *, *, #43614, .T. ) ;
#528 = CARTESIAN_POINT ( 'NONE',  ( -194.9999999999999432, 0.000000000000000000, 0.000000000000000000 ) ) ;
#529 = CARTESIAN_POINT ( 'NONE',  ( 130.0000000000008811, 17.00000000000000000, 0.000000000000000000 ) ) ;
#530 = VECTOR ( 'NONE', #42052, 1000.000000000000000 ) ;
#531 = ORIENTED_EDGE ( 'NONE', *, *, #41855, .T. ) ;
#532 = CARTESIAN_POINT ( 'NONE',  ( -126.6959734468149321, 1.749999999999996891, -159.1817124430720298 ) ) ;
#533 = CARTESIAN_POINT ( 'NONE',  ( -1.280882217648866117, 0.5301415400469891015, 9.960033073700733652 ) ) ;
#534 = EDGE_CURVE ( 'NONE', #28470, #12513, #27359, .T. ) ;
#535 = FACE_OUTER_BOUND ( 'NONE', #48692, .T. ) ;
#536 = EDGE_CURVE ( 'NONE', #38434, #12843, #25274, .T. ) ;
#537 = CARTESIAN_POINT ( 'NONE',  ( 168.9999999999999716, 10.00000000000006395, -350.0000000000001705 ) ) ;
#538 = AXIS2_PLACEMENT_3D ( 'NONE', #2831, #26198, #14128 ) ;
#539 = EDGE_CURVE ( 'NONE', #9223, #45368, #5772, .T. ) ;
#540 = CARTESIAN_POINT ( 'NONE',  ( 0.000000000000000000, 17.00000000000000000, 0.000000000000000000 ) ) ;
#541 = VERTEX_POINT ( 'NONE', #28876 ) ;
#542 = CARTESIAN_POINT ( 'NONE',  ( -1.250000000000000222, 0.000000000000000000, -3.333333333333333481 ) ) ;
#543 = CARTESIAN_POINT ( 'NONE',  ( -127.7210997126620242, -1.749999999999996891, -80.20683870891909351 ) ) ;
#544 = EDGE_LOOP ( 'NONE', ( #3336, #43444, #1050, #33795, #29407 ) ) ;
#545 = DIRECTION ( 'NONE',  ( 0.000000000000000000, 0.000000000000000000, -1.000000000000000000 ) ) ;
#546 = FACE_OUTER_BOUND ( 'NONE', #42414, .T. ) ;
#547 = ORIENTED_EDGE ( 'NONE', *, *, #1230, .F. ) ;
#548 = LINE ( 'NONE', #16187, #556 ) ;
#549 = CARTESIAN_POINT ( 'NONE',  ( -16.02661358026017524, -4.530191650547608972, -9.683996418299976483 ) ) ;
#550 = CARTESIAN_POINT ( 'NONE',  ( -14.99999999999906919, 17.00000000000000000, 0.000000000000000000 ) ) ;
#551 = DIRECTION ( 'NONE',  ( 1.000000000000000000, -4.758098676964956461E-16, -8.975803739141899931E-48 ) ) ;
#552 = AXIS2_PLACEMENT_3D ( 'NONE', #49748, #38283, #46673 ) ;
#553 = ADVANCED_FACE ( 'NONE', ( #32726 ), #1435, .F. ) ;
#554 = EDGE_LOOP ( 'NONE', ( #44360, #32925, #21521, #39510 ) ) ;
#555 = CARTESIAN_POINT ( 'NONE',  ( -206.6959734468149463, 0.000000000000000000, 165.0000000000000000 ) ) ;
#556 = VECTOR ( 'NONE', #4868, 1000.000000000000000 ) ;
#557 = CARTESIAN_POINT ( 'NONE',  ( 181.0000000000000000, -182.9999999999999716, -350.0000000000001705 ) ) ;
#558 = PLANE ( 'NONE',  #37929 ) ;
#559 = VERTEX_POINT ( 'NONE', #44993 ) ;
#560 = ORIENTED_EDGE ( 'NONE', *, *, #34963, .T. ) ;
#561 = DIRECTION ( 'NONE',  ( 1.000000000000000000, 0.000000000000000000, 0.000000000000000000 ) ) ;
#562 = FACE_OUTER_BOUND ( 'NONE', #36379, .T. ) ;
#563 =( BOUNDED_CURVE ( )  B_SPLINE_CURVE ( 3, ( #5786, #21426, #38810, #49593 ),
 .UNSPECIFIED., .F., .F. ) 
 B_SPLINE_CURVE_WITH_KNOTS ( ( 4, 4 ),
 ( 1.570796326794896558, 3.141592653589793116 ),
 .UNSPECIFIED. ) 
 CURVE ( )  GEOMETRIC_REPRESENTATION_ITEM ( )  RATIONAL_B_SPLINE_CURVE ( ( 1.000000000000000000, 0.8047378541243649375, 0.8047378541243649375, 1.000000000000000000 ) ) 
 REPRESENTATION_ITEM ( '' )  );
#564 = CARTESIAN_POINT ( 'NONE',  ( 339.9999999999999432, -168.9999999999999432, 343.9999999999998295 ) ) ;
#565 = CARTESIAN_POINT ( 'NONE',  ( -1.011271242968683426, -0.7347315653655928092, 3.333333333333333481 ) ) ;
#566 = VERTEX_POINT ( 'NONE', #21168 ) ;
#567 = DIRECTION ( 'NONE',  ( -1.000000000000000000, -0.000000000000000000, -0.000000000000000000 ) ) ;
#568 =( BOUNDED_CURVE ( )  B_SPLINE_CURVE ( 3, ( #26623, #27136, #28083, #11235 ),
 .UNSPECIFIED., .F., .F. ) 
 B_SPLINE_CURVE_WITH_KNOTS ( ( 4, 4 ),
 ( 1.570796326794896558, 3.141592653589793116 ),
 .UNSPECIFIED. ) 
 CURVE ( )  GEOMETRIC_REPRESENTATION_ITEM ( )  RATIONAL_B_SPLINE_CURVE ( ( 1.000000000000000000, 0.8047378541243649375, 0.8047378541243649375, 1.000000000000000000 ) ) 
 REPRESENTATION_ITEM ( '' )  );
#569 = CARTESIAN_POINT ( 'NONE',  ( -47.72109971266203132, -1.750000000000009548, 41.84341382277508359 ) ) ;
#570 = FACE_OUTER_BOUND ( 'NONE', #16621, .T. ) ;
#571 = DIRECTION ( 'NONE',  ( 0.000000000000000000, 0.000000000000000000, 1.000000000000000000 ) ) ;
#572 = VERTEX_POINT ( 'NONE', #13469 ) ;
#573 = DIRECTION ( 'NONE',  ( -1.000000000000000000, -0.000000000000000000, -0.000000000000000000 ) ) ;
#574 = VERTEX_POINT ( 'NONE', #21414 ) ;
#575 = FACE_OUTER_BOUND ( 'NONE', #37918, .T. ) ;
#576 = VERTEX_POINT ( 'NONE', #29130 ) ;
#577 = CARTESIAN_POINT ( 'NONE',  ( -4.945973446814917018, 1.025126265847097429, 42.56828755692800570 ) ) ;
#578 = CARTESIAN_POINT ( 'NONE',  ( -4.945973446814903696, 2.143131898507912917E-16, 2.568287556928034121 ) ) ;
#579 = DIRECTION ( 'NONE',  ( -1.000000000000000000, 0.000000000000000000, 0.000000000000000000 ) ) ;
#580 = ORIENTED_EDGE ( 'NONE', *, *, #21589, .T. ) ;
#581 = ADVANCED_FACE ( 'NONE', ( #9872 ), #36344, .T. ) ;
#582 = PLANE ( 'NONE',  #3188 ) ;
#583 = EDGE_CURVE ( 'NONE', #42490, #24640, #48326, .T. ) ;
#584 = VECTOR ( 'NONE', #25385, 1000.000000000000000 ) ;
#585 = DIRECTION ( 'NONE',  ( -1.000000000000000000, 0.000000000000000000, 0.000000000000000000 ) ) ;
#586 = VERTEX_POINT ( 'NONE', #1185 ) ;
#587 = CARTESIAN_POINT ( 'NONE',  ( -206.6959734468149463, 1.750000000000010214, -39.18171244307202983 ) ) ;
#588 = CARTESIAN_POINT ( 'NONE',  ( 32.27890028733795447, -1.750000000000009548, 41.84341382277508359 ) ) ;
#589 = CARTESIAN_POINT ( 'NONE',  ( -10.49999999999999467, -46.01315789473684248, -5.916985404131818171 ) ) ;
#590 = DIRECTION ( 'NONE',  ( 0.000000000000000000, 0.000000000000000000, -1.000000000000000000 ) ) ;
#591 = ORIENTED_EDGE ( 'NONE', *, *, #21037, .F. ) ;
#592 = EDGE_CURVE ( 'NONE', #28510, #10704, #32994, .T. ) ;
#593 = VERTEX_POINT ( 'NONE', #47822 ) ;
#594 = DIRECTION ( 'NONE',  ( 0.000000000000000000, 1.000000000000000000, -0.000000000000000000 ) ) ;
#595 = EDGE_CURVE ( 'NONE', #49549, #4874, #20923, .T. ) ;
#596 = EDGE_CURVE ( 'NONE', #45670, #46289, #13721, .T. ) ;
#597 = ORIENTED_EDGE ( 'NONE', *, *, #24654, .T. ) ;
#598 = LINE ( 'NONE', #43663, #20030 ) ;
#599 = DIRECTION ( 'NONE',  ( 0.000000000000000000, 0.2223603367690637489, -0.9749645535258953943 ) ) ;
#600 = FACE_OUTER_BOUND ( 'NONE', #36261, .T. ) ;
#601 = ORIENTED_EDGE ( 'NONE', *, *, #3400, .F. ) ;
#602 = CARTESIAN_POINT ( 'NONE',  ( 195.0540265531851105, 2.143131898507880377E-16, 79.06828755692797017 ) ) ;
#603 = ORIENTED_EDGE ( 'NONE', *, *, #32628, .T. ) ;
#604 = ADVANCED_FACE ( 'NONE', ( #36090 ), #930, .T. ) ;
#605 = FACE_OUTER_BOUND ( 'NONE', #3161, .T. ) ;
#606 = DIRECTION ( 'NONE',  ( 3.172065745548403743E-16, 1.000000000000000000, 0.000000000000000000 ) ) ;
#607 = ORIENTED_EDGE ( 'NONE', *, *, #46352, .F. ) ;
#608 = ORIENTED_EDGE ( 'NONE', *, *, #26583, .T. ) ;
#609 = VERTEX_POINT ( 'NONE', #32230 ) ;
#610 = DIRECTION ( 'NONE',  ( -1.000000000000000000, -0.000000000000000000, -0.000000000000000000 ) ) ;
#611 = CARTESIAN_POINT ( 'NONE',  ( -5.670847180967843570, -1.750000000000023315, 121.8434138227750623 ) ) ;
#612 = DIRECTION ( 'NONE',  ( 0.5038710255240859137, 0.000000000000000000, -0.8637789008984335659 ) ) ;
#613 = PRODUCT_DEFINITION_CONTEXT ( 'detailed design', #38126, 'design' ) ;
#614 = VERTEX_POINT ( 'NONE', #44251 ) ;
#615 = DIRECTION ( 'NONE',  ( -0.000000000000000000, -1.000000000000000000, 0.000000000000000000 ) ) ;
#616 = ORIENTED_EDGE ( 'NONE', *, *, #17986, .F. ) ;
#617 = CARTESIAN_POINT ( 'NONE',  ( 4.353119224256710496, 9.002796955358187247, 0.000000000000000000 ) ) ;
#618 = ORIENTED_EDGE ( 'NONE', *, *, #16431, .T. ) ;
#619 = CARTESIAN_POINT ( 'NONE',  ( 350.0000000000000000, -164.9999999999999432, -344.0000000000001705 ) ) ;
#620 = CARTESIAN_POINT ( 'NONE',  ( 34.32915281903212446, 1.750000000000009326, 161.8434138227750907 ) ) ;
#621 = DIRECTION ( 'NONE',  ( 0.000000000000000000, 0.000000000000000000, -1.000000000000000000 ) ) ;
#622 = DIRECTION ( 'NONE',  ( 0.000000000000000000, -1.000000000000000000, 0.000000000000000000 ) ) ;
#623 = CARTESIAN_POINT ( 'NONE',  ( -19.99999999999971223, 16.00000000000000000, -84.99999999999998579 ) ) ;
#624 = CARTESIAN_POINT ( 'NONE',  ( 432.7825420346616170, 74.83106485270648989, -130.5992382549688955 ) ) ;
#625 = ORIENTED_EDGE ( 'NONE', *, *, #32485, .F. ) ;
#626 = ORIENTED_EDGE ( 'NONE', *, *, #37900, .T. ) ;
#627 = DIRECTION ( 'NONE',  ( -0.000000000000000000, 0.000000000000000000, 1.000000000000000000 ) ) ;
#628 = FACE_OUTER_BOUND ( 'NONE', #50651, .T. ) ;
#629 = ADVANCED_FACE ( 'NONE', ( #5269 ), #9371, .F. ) ;
#630 = FACE_OUTER_BOUND ( 'NONE', #38256, .T. ) ;
#631 = DIRECTION ( 'NONE',  ( 0.000000000000000000, -1.000000000000000000, 5.664403186863042467E-17 ) ) ;
#632 = EDGE_LOOP ( 'NONE', ( #41784, #42230, #9108, #39526 ) ) ;
#633 = FACE_OUTER_BOUND ( 'NONE', #3064, .T. ) ;
#634 = CARTESIAN_POINT ( 'NONE',  ( -7.937171537365877327, -0.3824377404836087346, 9.432811472610140413 ) ) ;
#635 = ORIENTED_EDGE ( 'NONE', *, *, #15818, .F. ) ;
#636 = CARTESIAN_POINT ( 'NONE',  ( -0.6440276692615888310, -16.64212148744554298, -9.683996418299976483 ) ) ;
#637 = DIRECTION ( 'NONE',  ( 0.000000000000000000, 2.537652627714642000E-15, 1.000000000000000000 ) ) ;
#638 = DIRECTION ( 'NONE',  ( 0.000000000000000000, 0.000000000000000000, -1.000000000000000000 ) ) ;
#639 = VERTEX_POINT ( 'NONE', #48070 ) ;
#640 = ORIENTED_EDGE ( 'NONE', *, *, #27418, .F. ) ;
#641 = DIRECTION ( 'NONE',  ( -0.000000000000000000, -0.000000000000000000, -1.000000000000000000 ) ) ;
#642 = FACE_OUTER_BOUND ( 'NONE', #16793, .T. ) ;
#643 = VECTOR ( 'NONE', #47580, 1000.000000000000000 ) ;
#644 = ORIENTED_EDGE ( 'NONE', *, *, #10302, .T. ) ;
#645 = ORIENTED_EDGE ( 'NONE', *, *, #18172, .T. ) ;
#646 = CARTESIAN_POINT ( 'NONE',  ( -124.9459734468149463, 2.143131898507847836E-16, -120.9317124430720156 ) ) ;
#647 = DIRECTION ( 'NONE',  ( 1.000000000000000000, 0.000000000000000000, 0.000000000000000000 ) ) ;
#648 = CARTESIAN_POINT ( 'NONE',  ( 25.04522487443081502, -22.77512090857307925, 8.356839323120299312 ) ) ;
#649 = DIRECTION ( 'NONE',  ( -0.000000000000000000, -0.000000000000000000, -1.000000000000000000 ) ) ;
#650 = DIRECTION ( 'NONE',  ( -1.000000000000000000, 0.000000000000000000, -0.000000000000000000 ) ) ;
#651 = ORIENTED_EDGE ( 'NONE', *, *, #30859, .F. ) ;
#652 = ORIENTED_EDGE ( 'NONE', *, *, #762, .F. ) ;
#653 = ADVANCED_FACE ( 'NONE', ( #40684 ), #36606, .T. ) ;
#654 = ORIENTED_EDGE ( 'NONE', *, *, #31562, .T. ) ;
#655 = CARTESIAN_POINT ( 'NONE',  ( -34.08355720199904226, 2.371364769369340042, 7.455576670931136185 ) ) ;
#656 = ORIENTED_EDGE ( 'NONE', *, *, #48271, .F. ) ;
#657 = CARTESIAN_POINT ( 'NONE',  ( -1.057156451998854996, 0.7920882637787067804, 9.943883492372851407 ) ) ;
#658 = ORIENTED_EDGE ( 'NONE', *, *, #1230, .T. ) ;
#659 = ORIENTED_EDGE ( 'NONE', *, *, #38242, .F. ) ;
#660 = LINE ( 'NONE', #35837, #18061 ) ;
#661 = FACE_OUTER_BOUND ( 'NONE', #3377, .T. ) ;
#662 = CIRCLE ( 'NONE', #47316, 1.750000000000001554 ) ;
#663 = CARTESIAN_POINT ( 'NONE',  ( -204.9459734468149463, 2.143131898507880377E-16, 2.568287556927978166 ) ) ;
#664 = ORIENTED_EDGE ( 'NONE', *, *, #22451, .F. ) ;
#665 = ORIENTED_EDGE ( 'NONE', *, *, #13294, .F. ) ;
#666 = CARTESIAN_POINT ( 'NONE',  ( 34.08355720199905647, -2.371364769369109116, 7.455576670931136185 ) ) ;
#667 = CARTESIAN_POINT ( 'NONE',  ( -126.6959734468149321, 1.749999999999997335, 80.81828755692798438 ) ) ;
#668 = ORIENTED_EDGE ( 'NONE', *, *, #6729, .T. ) ;
#669 = CARTESIAN_POINT ( 'NONE',  ( -20.21530556545279111, 31.58467066308232063, -9.422646554964174470 ) ) ;
#670 = DIRECTION ( 'NONE',  ( -1.000000000000000000, 0.000000000000000000, 0.000000000000000000 ) ) ;
#671 = LINE ( 'NONE', #11708, #25318 ) ;
#672 = CARTESIAN_POINT ( 'NONE',  ( 20.40054609052976531, -26.26366202847973597, -3.760136334089591248 ) ) ;
#673 = EDGE_LOOP ( 'NONE', ( #3363, #25492, #26505, #29647 ) ) ;
#674 = CARTESIAN_POINT ( 'NONE',  ( -119.9999999999994174, 17.00000000000000000, -54.99999999999999289 ) ) ;
#675 = DIRECTION ( 'NONE',  ( 1.000000000000000000, -0.000000000000000000, -0.000000000000000000 ) ) ;
#676 = CARTESIAN_POINT ( 'NONE',  ( 155.0540265531850537, 1.025126265847089879, 122.5682875569280128 ) ) ;
#677 = EDGE_CURVE ( 'NONE', #7451, #29467, #310, .T. ) ;
#678 = CARTESIAN_POINT ( 'NONE',  ( 0.9494396179258391966, -9.954826186926261755, 9.646707543097345905 ) ) ;
#679 = AXIS2_PLACEMENT_3D ( 'NONE', #33054, #24590, #40002 ) ;
#680 = CARTESIAN_POINT ( 'NONE',  ( 80.00000000000153477, 16.00000000000000000, 60.00000000000000000 ) ) ;
#681 = CARTESIAN_POINT ( 'NONE',  ( 164.9999999999999716, 17.00000000000000000, -60.00000000000001421 ) ) ;
#682 = DIRECTION ( 'NONE',  ( 1.000000000000000000, 0.000000000000000000, 0.000000000000000000 ) ) ;
#683 =( BOUNDED_CURVE ( )  B_SPLINE_CURVE ( 3, ( #1713, #9405, #36121, #5040 ),
 .UNSPECIFIED., .F., .F. ) 
 B_SPLINE_CURVE_WITH_KNOTS ( ( 4, 4 ),
 ( 1.570796326794896558, 3.141592653589793116 ),
 .UNSPECIFIED. ) 
 CURVE ( )  GEOMETRIC_REPRESENTATION_ITEM ( )  RATIONAL_B_SPLINE_CURVE ( ( 1.000000000000000000, 0.8047378541243649375, 0.8047378541243649375, 1.000000000000000000 ) ) 
 REPRESENTATION_ITEM ( '' )  );
#684 = ORIENTED_EDGE ( 'NONE', *, *, #22229, .T. ) ;
#685 = CARTESIAN_POINT ( 'NONE',  ( 35.00000000000091660, 17.00000000000000000, -24.99999999999999289 ) ) ;
#686 = CARTESIAN_POINT ( 'NONE',  ( 0.3896797354184660667, -1.262193838292004155, 9.943883492372872723 ) ) ;
#687 = ORIENTED_EDGE ( 'NONE', *, *, #36269, .F. ) ;
#688 = B_SPLINE_CURVE_WITH_KNOTS ( 'NONE', 3,
 ( #8937, #24844, #17140, #45060 ),
 .UNSPECIFIED., .F., .F.,
 ( 4, 4 ),
 ( 0.01010185847678695022, 0.01012833122191988955 ),
 .UNSPECIFIED. ) ;
#689 = CARTESIAN_POINT ( 'NONE',  ( 154.3291528190321458, -1.750000000000009548, -40.20683870891912193 ) ) ;
#690 = LINE ( 'NONE', #30995, #5198 ) ;
#691 = CYLINDRICAL_SURFACE ( 'NONE', #41373, 1.750000000000015543 ) ;
#692 = VERTEX_POINT ( 'NONE', #29376 ) ;
#693 = DIRECTION ( 'NONE',  ( 0.000000000000000000, -0.000000000000000000, 1.000000000000000000 ) ) ;
#694 = B_SPLINE_SURFACE_WITH_KNOTS ( 'NONE', 3, 3, ( 
 ( #30681, #46277, #15527, #50370 ),
 ( #15286, #30946, #46531, #27073 ),
 ( #42705, #38897, #23215, #7579 ),
 ( #3722, #19374, #35056, #28845 ) ),
 .UNSPECIFIED., .F., .F., .F.,
 ( 4, 4 ),
 ( 4, 4 ),
 ( 0.000000000000000000, 1.000000000000000000 ),
 ( 0.000000000000000000, 1.000000000000000000 ),
 .UNSPECIFIED. ) ;
#695 = EDGE_LOOP ( 'NONE', ( #33411, #25754, #20493, #618 ) ) ;
#696 = ORIENTED_EDGE ( 'NONE', *, *, #28856, .F. ) ;
#697 = DIRECTION ( 'NONE',  ( -1.000000000000000000, 0.000000000000000000, 0.000000000000000000 ) ) ;
#698 = CARTESIAN_POINT ( 'NONE',  ( -210.0000000000000568, 0.000000000000000000, -119.1817124430720440 ) ) ;
#699 = ORIENTED_EDGE ( 'NONE', *, *, #40875, .F. ) ;
#700 = DIRECTION ( 'NONE',  ( 1.000000000000000000, 0.000000000000000000, 0.000000000000000000 ) ) ;
#701 = LINE ( 'NONE', #27656, #40511 ) ;
#702 = ORIENTED_EDGE ( 'NONE', *, *, #9302, .T. ) ;
#703 = ADVANCED_FACE ( 'NONE', ( #24523 ), #36856, .T. ) ;
#704 =( BOUNDED_CURVE ( )  B_SPLINE_CURVE ( 3, ( #40799, #48942, #14089, #33120 ),
 .UNSPECIFIED., .F., .F. ) 
 B_SPLINE_CURVE_WITH_KNOTS ( ( 4, 4 ),
 ( 0.000000000000000000, 1.570796326794896558 ),
 .UNSPECIFIED. ) 
 CURVE ( )  GEOMETRIC_REPRESENTATION_ITEM ( )  RATIONAL_B_SPLINE_CURVE ( ( 1.000000000000000000, 0.8047378541243649375, 0.8047378541243649375, 1.000000000000000000 ) ) 
 REPRESENTATION_ITEM ( '' )  );
#705 = CARTESIAN_POINT ( 'NONE',  ( 75.05402655318509630, 1.025126265847089879, 82.56828755692798438 ) ) ;
#706 = ORIENTED_EDGE ( 'NONE', *, *, #193, .T. ) ;
#707 = CARTESIAN_POINT ( 'NONE',  ( 194.9999999999999432, 0.000000000000000000, 0.000000000000000000 ) ) ;
#708 = DIRECTION ( 'NONE',  ( -1.000000000000000000, -0.000000000000000000, -0.000000000000000000 ) ) ;
#709 = CARTESIAN_POINT ( 'NONE',  ( -119.9999999999978400, 17.00000000000000000, 95.00000000000000000 ) ) ;
#710 = ORIENTED_EDGE ( 'NONE', *, *, #4911, .F. ) ;
#711 = AXIS2_PLACEMENT_3D ( 'NONE', #49529, #33197, #17779 ) ;
#712 = CARTESIAN_POINT ( 'NONE',  ( 34.95136153415558056, -36.40974830873469870, 8.356839323120299312 ) ) ;
#713 = CARTESIAN_POINT ( 'NONE',  ( 75.05402655318509630, 1.025126265847089879, 122.5682875569280128 ) ) ;
#714 = ORIENTED_EDGE ( 'NONE', *, *, #39946, .T. ) ;
#715 = VERTEX_POINT ( 'NONE', #28612 ) ;
#716 = ORIENTED_EDGE ( 'NONE', *, *, #36986, .T. ) ;
#717 = FACE_OUTER_BOUND ( 'NONE', #38405, .T. ) ;
#718 = EDGE_CURVE ( 'NONE', #17041, #22983, #49580, .T. ) ;
#719 = EDGE_CURVE ( 'NONE', #32283, #25110, #43691, .T. ) ;
#720 = LINE ( 'NONE', #35138, #11092 ) ;
#721 = ORIENTED_EDGE ( 'NONE', *, *, #6928, .T. ) ;
#722 = CLOSED_SHELL ( 'NONE', ( #33273, #13699, #32863, #47477, #42616, #48990, #26917, #42906, #40350, #7482, #18343, #10767, #37802, #12006, #35923, #10315, #35706, #47951 ) ) ;
#723 = EDGE_CURVE ( 'NONE', #541, #5037, #49825, .T. ) ;
#724 = DIRECTION ( 'NONE',  ( 0.000000000000000000, 1.000000000000000000, 0.000000000000000000 ) ) ;
#725 = CARTESIAN_POINT ( 'NONE',  ( 113.3040265531850537, 0.000000000000000000, 165.0000000000000000 ) ) ;
#726 = EDGE_CURVE ( 'NONE', #3329, #34466, #14990, .T. ) ;
#727 = DIRECTION ( 'NONE',  ( 0.000000000000000000, 0.000000000000000000, 1.000000000000000000 ) ) ;
#728 = PLANE ( 'NONE',  #43991 ) ;
#729 = CYLINDRICAL_SURFACE ( 'NONE', #31264, 1.750000000000015543 ) ;
#730 = CARTESIAN_POINT ( 'NONE',  ( 152.2789002873379900, 1.750000000000009548, 159.7931612910809065 ) ) ;
#731 = CARTESIAN_POINT ( 'NONE',  ( -204.9459734468149463, 2.143131898507880377E-16, -80.93171244307201562 ) ) ;
#732 = CARTESIAN_POINT ( 'NONE',  ( -14.99999999999970868, 17.00000000000000000, -60.00000000000000000 ) ) ;
#733 = CARTESIAN_POINT ( 'NONE',  ( -9.919534718723015843, 1.461167986671116470, 9.524510970296136136 ) ) ;
#734 = PLANE ( 'NONE',  #17438 ) ;
#735 = EDGE_CURVE ( 'NONE', #23031, #24640, #41747, .T. ) ;
#736 = CARTESIAN_POINT ( 'NONE',  ( 30.77287599203632951, 12.70002479445995824, 3.199614146704519602 ) ) ;
#737 = EDGE_CURVE ( 'NONE', #25893, #7888, #18657, .T. ) ;
#738 = DIRECTION ( 'NONE',  ( -1.000000000000000000, -0.000000000000000000, -0.000000000000000000 ) ) ;
#739 = ADVANCED_FACE ( 'NONE', ( #38101 ), #2185, .F. ) ;
#740 = EDGE_CURVE ( 'NONE', #30097, #19392, #10883, .T. ) ;
#741 = CARTESIAN_POINT ( 'NONE',  ( -204.9459734468149463, 2.143131898507880377E-16, 39.06828755692798438 ) ) ;
#742 = DIRECTION ( 'NONE',  ( 1.000000000000000000, 0.000000000000000000, 0.000000000000000000 ) ) ;
#743 = ORIENTED_EDGE ( 'NONE', *, *, #50525, .T. ) ;
#744 = CARTESIAN_POINT ( 'NONE',  ( 2.595273106918288164, 2.906811120256387326, 9.741991644047248045 ) ) ;
#745 = EDGE_CURVE ( 'NONE', #4376, #24866, #38008, .T. ) ;
#746 = DIRECTION ( 'NONE',  ( -0.000000000000000000, -0.000000000000000000, -1.000000000000000000 ) ) ;
#747 = CARTESIAN_POINT ( 'NONE',  ( 5.505322767148756569, -37.09368438467003415, 8.914903342594564961 ) ) ;
#748 = CARTESIAN_POINT ( 'NONE',  ( 153.3040265531850537, -1.750000000000009992, 160.8182875569279702 ) ) ;
#749 = VECTOR ( 'NONE', #19138, 1000.000000000000000 ) ;
#750 = VERTEX_POINT ( 'NONE', #17821 ) ;
#751 = FACE_OUTER_BOUND ( 'NONE', #17565, .T. ) ;
#752 = VECTOR ( 'NONE', #24361, 1000.000000000000000 ) ;
#753 = VECTOR ( 'NONE', #3880, 1000.000000000000000 ) ;
#754 = ORIENTED_EDGE ( 'NONE', *, *, #25734, .F. ) ;
#755 = VECTOR ( 'NONE', #25642, 1000.000000000000000 ) ;
#756 = CARTESIAN_POINT ( 'NONE',  ( -10.30302290646040397, -13.08520913973572597, -9.683996418299976483 ) ) ;
#757 = CARTESIAN_POINT ( 'NONE',  ( -124.9459734468149463, 2.143131898507847836E-16, -77.43171244307204404 ) ) ;
#758 = VECTOR ( 'NONE', #16905, 1000.000000000000000 ) ;
#759 = CARTESIAN_POINT ( 'NONE',  ( 224.9999999999999716, -175.0000000000000000, 32.29650858650035161 ) ) ;
#760 = ORIENTED_EDGE ( 'NONE', *, *, #40276, .T. ) ;
#761 = CARTESIAN_POINT ( 'NONE',  ( 344.0000000000000568, -165.0000000000001137, 340.0000000000000568 ) ) ;
#762 = EDGE_CURVE ( 'NONE', #38466, #44684, #48892, .T. ) ;
#763 = ORIENTED_EDGE ( 'NONE', *, *, #20651, .T. ) ;
#764 = ORIENTED_EDGE ( 'NONE', *, *, #23321, .T. ) ;
#765 = AXIS2_PLACEMENT_3D ( 'NONE', #29029, #12869, #12609 ) ;
#766 = EDGE_CURVE ( 'NONE', #31254, #1663, #37599, .T. ) ;
#767 = EDGE_CURVE ( 'NONE', #14253, #48821, #16231, .T. ) ;
#768 = ORIENTED_EDGE ( 'NONE', *, *, #15009, .T. ) ;
#769 = CARTESIAN_POINT ( 'NONE',  ( -6.000000000000000888, 0.000000000000000000, 15.00000000000000000 ) ) ;
#770 = DIRECTION ( 'NONE',  ( 0.000000000000000000, 0.000000000000000000, -1.000000000000000000 ) ) ;
#771 = ORIENTED_EDGE ( 'NONE', *, *, #33152, .T. ) ;
#772 = DIRECTION ( 'NONE',  ( 0.000000000000000000, 1.000000000000000000, 0.000000000000000000 ) ) ;
#773 = CARTESIAN_POINT ( 'NONE',  ( 350.0000000000000000, -164.9999999999999432, 339.9999999999997726 ) ) ;
#774 = ADVANCED_FACE ( 'NONE', ( #50080 ), #18072, .T. ) ;
#775 = CARTESIAN_POINT ( 'NONE',  ( 181.0000000000000000, -93.49999999999998579, -350.0000000000001705 ) ) ;
#776 = CARTESIAN_POINT ( 'NONE',  ( -16.94310420131188266, 28.83076186680435171, -8.917361510505369182 ) ) ;
#777 = EDGE_LOOP ( 'NONE', ( #3669, #1337, #39144 ) ) ;
#778 = EDGE_CURVE ( 'NONE', #19154, #19994, #662, .T. ) ;
#779 = PLANE ( 'NONE',  #43621 ) ;
#780 = ORIENTED_EDGE ( 'NONE', *, *, #22663, .T. ) ;
#781 = CARTESIAN_POINT ( 'NONE',  ( 135.0000000000021600, 16.00000000000000000, 95.00000000000000000 ) ) ;
#782 = ORIENTED_EDGE ( 'NONE', *, *, #44110, .F. ) ;
#783 = CARTESIAN_POINT ( 'NONE',  ( -1.088201916217454546, -0.7239275277298468092, 9.945465957785078359 ) ) ;
#784 = DIRECTION ( 'NONE',  ( 1.000000000000000000, 0.000000000000000000, 0.000000000000000000 ) ) ;
#785 = ORIENTED_EDGE ( 'NONE', *, *, #12346, .F. ) ;
#786 = DIRECTION ( 'NONE',  ( 4.996003610813203446E-16, 1.000000000000000000, 0.000000000000000000 ) ) ;
#787 = AXIS2_PLACEMENT_3D ( 'NONE', #7371, #10699, #11720 ) ;
#788 = CARTESIAN_POINT ( 'NONE',  ( -34.38425513258695077, 36.82177522737848108, 8.807470649214879543 ) ) ;
#789 = CARTESIAN_POINT ( 'NONE',  ( -19.99999999999940670, 17.00000000000000000, -30.00000000000000000 ) ) ;
#790 = FACE_OUTER_BOUND ( 'NONE', #30397, .T. ) ;
#791 = VECTOR ( 'NONE', #23137, 1000.000000000000000 ) ;
#792 = EDGE_LOOP ( 'NONE', ( #16265, #22967, #43892, #43654, #12939, #41162, #11499, #30707 ) ) ;
#793 =( BOUNDED_CURVE ( )  B_SPLINE_CURVE ( 3, ( #39098, #35003, #3405, #39345 ),
 .UNSPECIFIED., .F., .F. ) 
 B_SPLINE_CURVE_WITH_KNOTS ( ( 4, 4 ),
 ( 0.000000000000000000, 1.570796326794896558 ),
 .UNSPECIFIED. ) 
 CURVE ( )  GEOMETRIC_REPRESENTATION_ITEM ( )  RATIONAL_B_SPLINE_CURVE ( ( 1.000000000000000000, 0.8047378541243649375, 0.8047378541243649375, 1.000000000000000000 ) ) 
 REPRESENTATION_ITEM ( '' )  );
#794 = EDGE_CURVE ( 'NONE', #35777, #38611, #10388, .T. ) ;
#795 = DIRECTION ( 'NONE',  ( -1.586032892321652236E-16, -1.000000000000000000, -6.853681917100419162E-49 ) ) ;
#796 = VECTOR ( 'NONE', #5565, 1000.000000000000000 ) ;
#797 = CARTESIAN_POINT ( 'NONE',  ( 1.040834085586084257E-14, -6.912230148066169200, 5.000000000000000000 ) ) ;
#798 = VECTOR ( 'NONE', #15889, 1000.000000000000000 ) ;
#799 = DIRECTION ( 'NONE',  ( 0.000000000000000000, -1.000000000000000000, 0.000000000000000000 ) ) ;
#800 = ORIENTED_EDGE ( 'NONE', *, *, #21171, .T. ) ;
#801 = ADVANCED_FACE ( 'NONE', ( #14216 ), #41679, .T. ) ;
#802 = EDGE_LOOP ( 'NONE', ( #19892, #43000, #16154, #21779 ) ) ;
#803 = APPLICATION_PROTOCOL_DEFINITION ( 'draft international standard', 'automotive_design', 1998, #40744 ) ;
#805 = FACE_OUTER_BOUND ( 'NONE', #27242, .T. ) ;
#804 = VECTOR ( 'NONE', #10594, 1000.000000000000000 ) ;
#806 = CARTESIAN_POINT ( 'NONE',  ( 0.1265591857323814795, 1.213367045380162823, 9.963925895596176474 ) ) ;
#807 = EDGE_CURVE ( 'NONE', #14566, #8176, #18570, .T. ) ;
#808 = EDGE_CURVE ( 'NONE', #7132, #20673, #30143, .T. ) ;
#809 = DIRECTION ( 'NONE',  ( -1.000000000000000000, 0.000000000000000000, 0.000000000000000000 ) ) ;
#810 = CARTESIAN_POINT ( 'NONE',  ( -85.67084718096784002, -1.750000000000010436, -80.20683870891910772 ) ) ;
#811 = CARTESIAN_POINT ( 'NONE',  ( 35.00000000000186162, 16.00000000000000000, 65.00000000000000000 ) ) ;
#812 = ORIENTED_EDGE ( 'NONE', *, *, #6128, .T. ) ;
#813 = EDGE_CURVE ( 'NONE', #46472, #47613, #15528, .T. ) ;
#814 = CARTESIAN_POINT ( 'NONE',  ( -208.1473046169136580, -154.8119894309599260, 472.8425600500171981 ) ) ;
#815 = ADVANCED_FACE ( 'NONE', ( #7814 ), #26795, .T. ) ;
#816 = CARTESIAN_POINT ( 'NONE',  ( 340.0000000000000000, 165.0000000000000000, -94.00000000000019895 ) ) ;
#817 = LINE ( 'NONE', #58, #1250 ) ;
#818 = CARTESIAN_POINT ( 'NONE',  ( 0.5107275442771160856, 1.175643901748075537, 9.976582533991678048 ) ) ;
#819 = EDGE_LOOP ( 'NONE', ( #45356, #48998, #15248, #7254 ) ) ;
#820 = FACE_BOUND ( 'NONE', #42955, .T. ) ;
#821 = ORIENTED_EDGE ( 'NONE', *, *, #15184, .F. ) ;
#822 = DIRECTION ( 'NONE',  ( -1.000000000000000000, -0.000000000000000000, -0.000000000000000000 ) ) ;
#823 = ORIENTED_EDGE ( 'NONE', *, *, #37911, .F. ) ;
#824 = CARTESIAN_POINT ( 'NONE',  ( 195.0540265531851105, 2.143131898507880377E-16, -80.93171244307201562 ) ) ;
#825 = DIRECTION ( 'NONE',  ( 0.000000000000000000, 3.186989995019654210E-49, 1.000000000000000000 ) ) ;
#826 = LINE ( 'NONE', #16475, #23214 ) ;
#827 = DIRECTION ( 'NONE',  ( 1.000000000000000000, -4.996003610813203446E-16, 1.033975765691284410E-24 ) ) ;
#828 = AXIS2_PLACEMENT_3D ( 'NONE', #16656, #16407, #1278 ) ;
#829 = VERTEX_POINT ( 'NONE', #368 ) ;
#830 = AXIS2_PLACEMENT_3D ( 'NONE', #22262, #22003, #42013 ) ;
#831 = VECTOR ( 'NONE', #20626, 1000.000000000000000 ) ;
#832 = DIRECTION ( 'NONE',  ( -1.000000000000000000, 0.000000000000000000, -0.000000000000000000 ) ) ;
#833 = EDGE_CURVE ( 'NONE', #38070, #15143, #32836, .T. ) ;
#834 = LINE ( 'NONE', #43911, #33679 ) ;
#835 = VERTEX_POINT ( 'NONE', #19344 ) ;
#836 = CARTESIAN_POINT ( 'NONE',  ( -208.4459734468148611, 1.025126265847089213, -37.43171244307202272 ) ) ;
#837 = CARTESIAN_POINT ( 'NONE',  ( -44.94597344681493922, 2.143131898507880377E-16, 165.0000000000000000 ) ) ;
#838 = DIRECTION ( 'NONE',  ( -1.156482317317870492E-16, 1.000000000000000000, 0.000000000000000000 ) ) ;
#839 = CARTESIAN_POINT ( 'NONE',  ( 35.00000000000152767, 16.00000000000000000, 35.00000000000000000 ) ) ;
#840 = AXIS2_PLACEMENT_3D ( 'NONE', #7728, #46676, #34680 ) ;
#841 = ORIENTED_EDGE ( 'NONE', *, *, #33518, .T. ) ;
#842 = PRODUCT_DEFINITION ( 'UNKNOWN', '', #50382, #12393 ) ;
#843 = ORIENTED_EDGE ( 'NONE', *, *, #48550, .T. ) ;
#844 = CARTESIAN_POINT ( 'NONE',  ( -14.99999999999970868, 16.00000000000000000, -84.99999999999998579 ) ) ;
#845 = VECTOR ( 'NONE', #3851, 1000.000000000000000 ) ;
#846 = ORIENTED_EDGE ( 'NONE', *, *, #17978, .T. ) ;
#847 = DIRECTION ( 'NONE',  ( 0.000000000000000000, 0.000000000000000000, -1.000000000000000000 ) ) ;
#848 = CARTESIAN_POINT ( 'NONE',  ( -164.9999999999990905, 17.00000000000000000, -24.99999999999999289 ) ) ;
#849 = CARTESIAN_POINT ( 'NONE',  ( 181.0000000000000000, 165.0000000000000000, -356.0000000000001705 ) ) ;
#850 = ORIENTED_EDGE ( 'NONE', *, *, #26302, .T. ) ;
#851 = LINE ( 'NONE', #19823, #3024 ) ;
#852 = EDGE_CURVE ( 'NONE', #6557, #6202, #30915, .T. ) ;
#853 = CARTESIAN_POINT ( 'NONE',  ( 341.9999999999999432, -174.9999999999999432, 343.9999999999998295 ) ) ;
#854 =( BOUNDED_CURVE ( )  B_SPLINE_CURVE ( 3, ( #12564, #12315, #543, #19499 ),
 .UNSPECIFIED., .F., .F. ) 
 B_SPLINE_CURVE_WITH_KNOTS ( ( 4, 4 ),
 ( 0.000000000000000000, 1.570796326794896558 ),
 .UNSPECIFIED. ) 
 CURVE ( )  GEOMETRIC_REPRESENTATION_ITEM ( )  RATIONAL_B_SPLINE_CURVE ( ( 1.000000000000000000, 0.8047378541243649375, 0.8047378541243649375, 1.000000000000000000 ) ) 
 REPRESENTATION_ITEM ( '' )  );
#855 = CARTESIAN_POINT ( 'NONE',  ( -204.9459734468148895, -1.025126265847089657, 119.0682875569279560 ) ) ;
#856 = ORIENTED_EDGE ( 'NONE', *, *, #7061, .T. ) ;
#857 = ORIENTED_EDGE ( 'NONE', *, *, #37508, .F. ) ;
#858 = EDGE_CURVE ( 'NONE', #47433, #8314, #11391, .T. ) ;
#859 = ORIENTED_EDGE ( 'NONE', *, *, #37775, .T. ) ;
#860 = FACE_OUTER_BOUND ( 'NONE', #47872, .T. ) ;
#861 = CARTESIAN_POINT ( 'NONE',  ( 153.3040265531850537, 0.000000000000000000, 165.0000000000000000 ) ) ;
#862 =( BOUNDED_CURVE ( )  B_SPLINE_CURVE ( 3, ( #46764, #38884, #31695, #35808 ),
 .UNSPECIFIED., .F., .F. ) 
 B_SPLINE_CURVE_WITH_KNOTS ( ( 4, 4 ),
 ( 0.000000000000000000, 1.570796326794896780 ),
 .UNSPECIFIED. ) 
 CURVE ( )  GEOMETRIC_REPRESENTATION_ITEM ( )  RATIONAL_B_SPLINE_CURVE ( ( 1.000000000000000000, 0.8047378541243649375, 0.8047378541243649375, 1.000000000000000000 ) ) 
 REPRESENTATION_ITEM ( '' )  );
#863 = CARTESIAN_POINT ( 'NONE',  ( -582.5000000000000000, -62.49999999999998579, -58.60000000000003695 ) ) ;
#864 = ORIENTED_EDGE ( 'NONE', *, *, #18638, .T. ) ;
#865 = VERTEX_POINT ( 'NONE', #23456 ) ;
#866 = CARTESIAN_POINT ( 'NONE',  ( -46.10908423965022251, -19.89422939639105437, 1.847720168420772691 ) ) ;
#868 = ORIENTED_EDGE ( 'NONE', *, *, #35811, .F. ) ;
#867 = AXIS2_PLACEMENT_3D ( 'NONE', #20688, #16848, #48346 ) ;
#869 = DIRECTION ( 'NONE',  ( 0.000000000000000000, 0.000000000000000000, 1.000000000000000000 ) ) ;
#870 = CARTESIAN_POINT ( 'NONE',  ( 360.0000000000000000, 169.0000000000000000, -344.0000000000001705 ) ) ;
#871 = LINE ( 'NONE', #16519, #9645 ) ;
#872 = CARTESIAN_POINT ( 'NONE',  ( 155.0540265531850537, -1.025126265847088991, -157.4317124430720582 ) ) ;
#873 = EDGE_CURVE ( 'NONE', #23733, #17617, #46498, .T. ) ;
#874 = AXIS2_PLACEMENT_3D ( 'NONE', #50548, #11862, #46963 ) ;
#875 = EDGE_CURVE ( 'NONE', #3991, #24185, #15745, .T. ) ;
#876 = SURFACE_STYLE_FILL_AREA ( #36031 ) ;
#877 = CARTESIAN_POINT ( 'NONE',  ( 9.999999999999998224, -41.51315789473684248, -25.00000000000000000 ) ) ;
#878 = CARTESIAN_POINT ( 'NONE',  ( 350.0000000000001137, 165.0000000000000000, 339.9999999999997726 ) ) ;
#879 = ORIENTED_EDGE ( 'NONE', *, *, #10874, .F. ) ;
#881 = VECTOR ( 'NONE', #25390, 1000.000000000000000 ) ;
#880 = CARTESIAN_POINT ( 'NONE',  ( -19.99999999999815969, 16.00000000000000000, 65.00000000000000000 ) ) ;
#882 = COLOUR_RGB ( '',0.7921568627450980005, 0.8196078431372548767, 0.9333333333333333481 ) ;
#883 = ADVANCED_FACE ( 'NONE', ( #35791 ), #3095, .T. ) ;
#885 = AXIS2_PLACEMENT_3D ( 'NONE', #24920, #14879, #22568 ) ;
#884 = CARTESIAN_POINT ( 'NONE',  ( -9.645054515263723260, 2.693981805359463078, 6.429802539306485265 ) ) ;
#886 = DIRECTION ( 'NONE',  ( 1.000000000000000000, 0.000000000000000000, -0.000000000000000000 ) ) ;
#887 = EDGE_CURVE ( 'NONE', #25778, #16503, #8068, .T. ) ;
#888 = ADVANCED_FACE ( 'NONE', ( #35027, #43446 ), #35271, .F. ) ;
#889 = CARTESIAN_POINT ( 'NONE',  ( -64.99999999999940314, 17.00000000000000000, -54.99999999999999289 ) ) ;
#890 = CARTESIAN_POINT ( 'NONE',  ( 356.0000000000000000, 175.0000000000000284, -106.0000000000001990 ) ) ;
#891 = VERTEX_POINT ( 'NONE', #8318 ) ;
#892 = CARTESIAN_POINT ( 'NONE',  ( 85.00000000000184741, 17.00000000000000000, 65.00000000000000000 ) ) ;
#893 = ADVANCED_FACE ( 'NONE', ( #43200 ), #31679, .T. ) ;
#894 = LINE ( 'NONE', #40643, #19792 ) ;
#895 = ORIENTED_EDGE ( 'NONE', *, *, #4687, .F. ) ;
#896 = CARTESIAN_POINT ( 'NONE',  ( 4.672045878990125800, -50.00000000000000711, 1.847720168420772691 ) ) ;
#897 = CARTESIAN_POINT ( 'NONE',  ( 3.239037401336969602, 33.28348308860766025, -8.917361510505369182 ) ) ;
#898 = FACE_OUTER_BOUND ( 'NONE', #9786, .T. ) ;
#899 = DIRECTION ( 'NONE',  ( -1.000000000000000000, 0.000000000000000000, -2.958228394578794270E-31 ) ) ;
#900 = B_SPLINE_CURVE_WITH_KNOTS ( 'NONE', 3,
 ( #9085, #634, #24744, #13179 ),
 .UNSPECIFIED., .F., .F.,
 ( 4, 4 ),
 ( 0.8097120833243681703, 0.9322955464062560038 ),
 .UNSPECIFIED. ) ;
#901 = EDGE_LOOP ( 'NONE', ( #812, #8607, #36597, #25658, #49808, #20531, #25126, #10877 ) ) ;
#902 = ORIENTED_EDGE ( 'NONE', *, *, #48896, .F. ) ;
#903 = CARTESIAN_POINT ( 'NONE',  ( 153.3040265531850537, -1.750000000000010658, -119.1817124430720440 ) ) ;
#904 = CARTESIAN_POINT ( 'NONE',  ( 14.91630425054810161, -7.943683830272122215, -9.008049429158100807 ) ) ;
#905 = AXIS2_PLACEMENT_3D ( 'NONE', #21960, #14251, #29911 ) ;
#906 = AXIS2_PLACEMENT_3D ( 'NONE', #14046, #29713, #45328 ) ;
#907 = VERTEX_POINT ( 'NONE', #23706 ) ;
#908 = ORIENTED_EDGE ( 'NONE', *, *, #17972, .T. ) ;
#909 = CARTESIAN_POINT ( 'NONE',  ( -44.94597344681493922, 2.143131898507880377E-16, 159.0682875569279702 ) ) ;
#910 = CARTESIAN_POINT ( 'NONE',  ( 35.05402655318504657, 2.143131898507880377E-16, 42.56828755692798438 ) ) ;
#911 = CARTESIAN_POINT ( 'NONE',  ( -204.9459734468148895, 1.025126265847089213, -0.9317124430720324924 ) ) ;
#912 = CARTESIAN_POINT ( 'NONE',  ( 358.0000000000000000, 181.0000000000000284, -356.0000000000001705 ) ) ;
#913 = VERTEX_POINT ( 'NONE', #3428 ) ;
#914 = ORIENTED_EDGE ( 'NONE', *, *, #10312, .F. ) ;
#915 = ORIENTED_EDGE ( 'NONE', *, *, #35068, .T. ) ;
#916 = VECTOR ( 'NONE', #24302, 1000.000000000000000 ) ;
#917 = ADVANCED_FACE ( 'NONE', ( #47265 ), #4455, .F. ) ;
#918 = CARTESIAN_POINT ( 'NONE',  ( -84.94597344681494633, 2.143131898507880377E-16, -77.43171244307204404 ) ) ;
#919 = LINE ( 'NONE', #40420, #42638 ) ;
#920 = VERTEX_POINT ( 'NONE', #34765 ) ;
#921 = VERTEX_POINT ( 'NONE', #15493 ) ;
#922 = CARTESIAN_POINT ( 'NONE',  ( 166.9999999999999716, -81.49999999999997158, -350.0000000000001705 ) ) ;
#923 = FACE_OUTER_BOUND ( 'NONE', #18696, .T. ) ;
#924 = CARTESIAN_POINT ( 'NONE',  ( -204.9459734468149463, 2.143131898507880377E-16, -117.4317124430720725 ) ) ;
#925 = ORIENTED_EDGE ( 'NONE', *, *, #735, .T. ) ;
#926 = ORIENTED_EDGE ( 'NONE', *, *, #50038, .F. ) ;
#927 = CARTESIAN_POINT ( 'NONE',  ( 1.437255894074055185, -3.713052624461447682, -1.301042606982605321E-15 ) ) ;
#928 = CARTESIAN_POINT ( 'NONE',  ( -164.9459734468149463, 1.025126265847089657, -80.93171244307201562 ) ) ;
#929 = ORIENTED_EDGE ( 'NONE', *, *, #34476, .T. ) ;
#930 = CYLINDRICAL_SURFACE ( 'NONE', #24074, 1.750000000000015543 ) ;
#931 = CARTESIAN_POINT ( 'NONE',  ( -207.7210997126620384, 1.750000000000009548, 121.8434138227750623 ) ) ;
#932 = CARTESIAN_POINT ( 'NONE',  ( -1.862232582514199875, -0.9302239440314029606, 9.888808121373916293 ) ) ;
#933 = EDGE_CURVE ( 'NONE', #12765, #28712, #42680, .T. ) ;
#934 = EDGE_CURVE ( 'NONE', #2472, #2811, #29066, .T. ) ;
#935 = CARTESIAN_POINT ( 'NONE',  ( -84.94597344681494633, 2.143131898507873721E-16, 165.0000000000000000 ) ) ;
#936 = VERTEX_POINT ( 'NONE', #12401 ) ;
#937 = LINE ( 'NONE', #39687, #19297 ) ;
#938 = CARTESIAN_POINT ( 'NONE',  ( 17.23491422248386584, -0.5912720620000816441, 8.727788335465566760 ) ) ;
#939 = CARTESIAN_POINT ( 'NONE',  ( 210.0000000000000568, 0.000000000000000000, -79.18171244307201562 ) ) ;
#940 = VECTOR ( 'NONE', #40898, 1000.000000000000000 ) ;
#941 = ADVANCED_FACE ( 'NONE', ( #36028 ), #13159, .F. ) ;
#942 = DIRECTION ( 'NONE',  ( -0.000000000000000000, -0.000000000000000000, -1.000000000000000000 ) ) ;
#943 = EDGE_CURVE ( 'NONE', #29362, #4473, #21108, .T. ) ;
#944 = ADVANCED_FACE ( 'NONE', ( #47762 ), #9567, .T. ) ;
#945 = LINE ( 'NONE', #44015, #12242 ) ;
#946 = VECTOR ( 'NONE', #12223, 1000.000000000000000 ) ;
#947 = LINE ( 'NONE', #16587, #9432 ) ;
#948 = CIRCLE ( 'NONE', #42702, 4.000000000000003553 ) ;
#949 = CARTESIAN_POINT ( 'NONE',  ( 20.08067494016817633, 41.72051557472632055, 7.455576670931136185 ) ) ;
#950 = VERTEX_POINT ( 'NONE', #33187 ) ;
#951 =( LENGTH_UNIT ( ) NAMED_UNIT ( * ) SI_UNIT ( .MILLI., .METRE. ) );
#952 = CARTESIAN_POINT ( 'NONE',  ( -35.87018513526855656, -11.05844981164215746, -6.568693074176323421 ) ) ;
#953 = VERTEX_POINT ( 'NONE', #13403 ) ;
#954 = CARTESIAN_POINT ( 'NONE',  ( 10.00419011302946259, 8.486842105263161073, 18.42339408367722697 ) ) ;
#955 = DIRECTION ( 'NONE',  ( -0.2599384441937725998, 0.8000082703740912793, -0.5407575913134976542 ) ) ;
#956 = CARTESIAN_POINT ( 'NONE',  ( -204.9459734468149463, 2.143131898507880377E-16, -77.43171244307204404 ) ) ;
#957 = ORIENTED_EDGE ( 'NONE', *, *, #47722, .F. ) ;
#958 = FACE_OUTER_BOUND ( 'NONE', #48495, .T. ) ;
#959 = ORIENTED_EDGE ( 'NONE', *, *, #6440, .T. ) ;
#960 = VERTEX_POINT ( 'NONE', #8817 ) ;
#961 = CARTESIAN_POINT ( 'NONE',  ( -3.345242017215803276, 2.159124855890678596, -2.642742795433417058E-16 ) ) ;
#962 = CYLINDRICAL_SURFACE ( 'NONE', #6597, 1.750000000000008438 ) ;
#963 = ORIENTED_EDGE ( 'NONE', *, *, #1726, .F. ) ;
#964 = DIRECTION ( 'NONE',  ( -1.586032880504786307E-16, 1.654361225106055350E-24, -1.000000000000000000 ) ) ;
#965 = CYLINDRICAL_SURFACE ( 'NONE', #36426, 1.750000000000001554 ) ;
#966 = ORIENTED_EDGE ( 'NONE', *, *, #43724, .T. ) ;
#967 = VECTOR ( 'NONE', #8554, 1000.000000000000000 ) ;
#968 = AXIS2_PLACEMENT_3D ( 'NONE', #46813, #24023, #39678 ) ;
#969 = CARTESIAN_POINT ( 'NONE',  ( 210.0000000000000568, 2.143131898507881856E-16, 119.0682875569279560 ) ) ;
#970 = VERTEX_POINT ( 'NONE', #24218 ) ;
#971 = EDGE_CURVE ( 'NONE', #865, #3838, #17011, .T. ) ;
#972 = CARTESIAN_POINT ( 'NONE',  ( -8.445973446814962315, -1.025126265847097207, -157.4317124430720014 ) ) ;
#973 = CARTESIAN_POINT ( 'NONE',  ( -10.01251772323708522, 8.486842105263161073, -18.46084505325461578 ) ) ;
#974 = ORIENTED_EDGE ( 'NONE', *, *, #47561, .T. ) ;
#975 = CARTESIAN_POINT ( 'NONE',  ( 370.7621192902014968, 70.03596893647589638, -94.69675437945477370 ) ) ;
#976 = VECTOR ( 'NONE', #24664, 1000.000000000000000 ) ;
#977 = CARTESIAN_POINT ( 'NONE',  ( 4.030068433199813782, -6.879221474127158231, -6.505213034913026604E-16 ) ) ;
#978 = ORIENTED_EDGE ( 'NONE', *, *, #12489, .T. ) ;
#979 = ORIENTED_EDGE ( 'NONE', *, *, #1420, .T. ) ;
#980 = VERTEX_POINT ( 'NONE', #870 ) ;
#981 = LINE ( 'NONE', #28431, #46677 ) ;
#982 = CARTESIAN_POINT ( 'NONE',  ( 191.5540265531850537, 1.025126265847089657, -80.93171244307201562 ) ) ;
#983 = VECTOR ( 'NONE', #33572, 1000.000000000000000 ) ;
#984 = ORIENTED_EDGE ( 'NONE', *, *, #12101, .F. ) ;
#985 = LINE ( 'NONE', #10188, #43833 ) ;
#986 = CYLINDRICAL_SURFACE ( 'NONE', #23136, 1.750000000000008438 ) ;
#987 = DIRECTION ( 'NONE',  ( 1.000000000000000000, 0.000000000000000000, 0.000000000000000000 ) ) ;
#988 = DIRECTION ( 'NONE',  ( 0.000000000000000000, 0.000000000000000000, -1.000000000000000000 ) ) ;
#989 = CARTESIAN_POINT ( 'NONE',  ( 0.000000000000000000, 0.000000000000000000, 10.00000000000000000 ) ) ;
#990 = CARTESIAN_POINT ( 'NONE',  ( 15.00000000000000000, 8.986842105263161073, 18.46084505325461578 ) ) ;
#991 = PLANE ( 'NONE',  #47135 ) ;
#992 = FACE_OUTER_BOUND ( 'NONE', #20572, .T. ) ;
#993 = CARTESIAN_POINT ( 'NONE',  ( 31.93002621080262671, 9.285431160462559674, -2.408242355805840784 ) ) ;
#994 = FACE_BOUND ( 'NONE', #1999, .T. ) ;
#995 =( BOUNDED_CURVE ( )  B_SPLINE_CURVE ( 3, ( #20608, #1379, #32169, #1875 ),
 .UNSPECIFIED., .F., .F. ) 
 B_SPLINE_CURVE_WITH_KNOTS ( ( 4, 4 ),
 ( 0.000000000000000000, 1.570796326794896558 ),
 .UNSPECIFIED. ) 
 CURVE ( )  GEOMETRIC_REPRESENTATION_ITEM ( )  RATIONAL_B_SPLINE_CURVE ( ( 1.000000000000000000, 0.8047378541243649375, 0.8047378541243649375, 1.000000000000000000 ) ) 
 REPRESENTATION_ITEM ( '' )  );
#996 = UNCERTAINTY_MEASURE_WITH_UNIT (LENGTH_MEASURE( 1.000000000000000082E-05 ), #25917, 'distance_accuracy_value', 'NONE');
#997 = CARTESIAN_POINT ( 'NONE',  ( -64.99999999999815259, 17.00000000000000000, 90.00000000000000000 ) ) ;
#998 = ORIENTED_EDGE ( 'NONE', *, *, #4229, .F. ) ;
#999 = EDGE_CURVE ( 'NONE', #12768, #45415, #1198, .T. ) ;
#1000 = FACE_OUTER_BOUND ( 'NONE', #32780, .T. ) ;
#1001 =( BOUNDED_CURVE ( )  B_SPLINE_CURVE ( 3, ( #47575, #25032, #24518, #44247 ),
 .UNSPECIFIED., .F., .F. ) 
 B_SPLINE_CURVE_WITH_KNOTS ( ( 4, 4 ),
 ( 4.712388980384689674, 6.283185307179586232 ),
 .UNSPECIFIED. ) 
 CURVE ( )  GEOMETRIC_REPRESENTATION_ITEM ( )  RATIONAL_B_SPLINE_CURVE ( ( 1.000000000000000000, 0.8047378541243649375, 0.8047378541243649375, 1.000000000000000000 ) ) 
 REPRESENTATION_ITEM ( '' )  );
#1002 = AXIS2_PLACEMENT_3D ( 'NONE', #43365, #551, #47189 ) ;
#1003 = DIRECTION ( 'NONE',  ( -0.000000000000000000, -1.000000000000000000, -0.000000000000000000 ) ) ;
#1004 = CARTESIAN_POINT ( 'NONE',  ( 210.0000000000000568, 0.000000000000000000, 0.8182875569279768335 ) ) ;
#1005 = DIRECTION ( 'NONE',  ( -0.000000000000000000, -0.000000000000000000, -1.000000000000000000 ) ) ;
#1006 = AXIS2_PLACEMENT_3D ( 'NONE', #10575, #7241, #26244 ) ;
#1007 = ORIENTED_EDGE ( 'NONE', *, *, #6239, .F. ) ;
#1008 = SURFACE_STYLE_USAGE ( .BOTH. , #15639 ) ;
#1009 = AXIS2_PLACEMENT_3D ( 'NONE', #24502, #44226, #9104 ) ;
#1010 = CARTESIAN_POINT ( 'NONE',  ( -210.0000000000000568, 0.000000000000000000, 80.81828755692798438 ) ) ;
#1011 = ORIENTED_EDGE ( 'NONE', *, *, #33096, .F. ) ;
#1012 = CARTESIAN_POINT ( 'NONE',  ( -0.9983599181300891745, -1.124146016603549070, 9.953784399990620813 ) ) ;
#1013 = CARTESIAN_POINT ( 'NONE',  ( 169.0000000000000000, -174.9999999999999716, -111.0000000000001563 ) ) ;
#1014 = DIRECTION ( 'NONE',  ( 0.000000000000000000, 0.000000000000000000, -1.000000000000000000 ) ) ;
#1015 =( BOUNDED_CURVE ( )  B_SPLINE_CURVE ( 3, ( #7919, #15095, #7653, #30753 ),
 .UNSPECIFIED., .F., .F. ) 
 B_SPLINE_CURVE_WITH_KNOTS ( ( 4, 4 ),
 ( 4.712388980384689674, 6.283185307179586232 ),
 .UNSPECIFIED. ) 
 CURVE ( )  GEOMETRIC_REPRESENTATION_ITEM ( )  RATIONAL_B_SPLINE_CURVE ( ( 1.000000000000000000, 0.8047378541243649375, 0.8047378541243649375, 1.000000000000000000 ) ) 
 REPRESENTATION_ITEM ( '' )  );
#1016 = VERTEX_POINT ( 'NONE', #25216 ) ;
#1017 = ORIENTED_EDGE ( 'NONE', *, *, #10506, .T. ) ;
#1018 = ORIENTED_EDGE ( 'NONE', *, *, #28826, .T. ) ;
#1019 = ORIENTED_EDGE ( 'NONE', *, *, #24264, .T. ) ;
#1020 = DIRECTION ( 'NONE',  ( -1.000000000000000000, -0.000000000000000000, -0.000000000000000000 ) ) ;
#1021 = CARTESIAN_POINT ( 'NONE',  ( 210.0000000000000568, 0.000000000000000000, -79.18171244307201562 ) ) ;
#1022 = VERTEX_POINT ( 'NONE', #16761 ) ;
#1023 = FACE_OUTER_BOUND ( 'NONE', #10966, .T. ) ;
#1024 = DIRECTION ( 'NONE',  ( 0.000000000000000000, 0.000000000000000000, -1.000000000000000000 ) ) ;
#1025 = DIRECTION ( 'NONE',  ( 2.874857526315640942E-31, -1.000000000000000000, 2.537652627714643577E-15 ) ) ;
#1026 = AXIS2_PLACEMENT_3D ( 'NONE', #8099, #23744, #11682 ) ;
#1027 = CARTESIAN_POINT ( 'NONE',  ( 85.00000000000056843, 17.00000000000000000, -30.00000000000000000 ) ) ;
#1028 = ORIENTED_EDGE ( 'NONE', *, *, #35334, .F. ) ;
#1029 = CARTESIAN_POINT ( 'NONE',  ( -177.4999999999999716, -112.5000000000000000, 0.000000000000000000 ) ) ;
#1030 = ORIENTED_EDGE ( 'NONE', *, *, #46824, .F. ) ;
#1031 = LINE ( 'NONE', #47673, #2150 ) ;
#1032 = CARTESIAN_POINT ( 'NONE',  ( -86.69597344681496054, 0.000000000000000000, 165.0000000000000000 ) ) ;
#1033 = VECTOR ( 'NONE', #47820, 1000.000000000000000 ) ;
#1034 = EDGE_LOOP ( 'NONE', ( #26621, #37966, #49162, #17827 ) ) ;
#1035 = CARTESIAN_POINT ( 'NONE',  ( -14.99999999999876366, 17.00000000000000000, 5.000000000000004441 ) ) ;
#1036 = CIRCLE ( 'NONE', #44408, 37.50000000000000000 ) ;
#1037 = CARTESIAN_POINT ( 'NONE',  ( -34.91952936320829792, 13.67027684621028349, -9.422646554964178023 ) ) ;
#1038 = ORIENTED_EDGE ( 'NONE', *, *, #33245, .F. ) ;
#1039 = VECTOR ( 'NONE', #9761, 1000.000000000000114 ) ;
#1040 = CARTESIAN_POINT ( 'NONE',  ( -44.94597344681493922, 1.025126265847089657, 79.06828755692797017 ) ) ;
#1041 = CARTESIAN_POINT ( 'NONE',  ( -1.011271242968683426, -0.7347315653655928092, 10.00000000000000000 ) ) ;
#1042 = LINE ( 'NONE', #5128, #26252 ) ;
#1043 = DIRECTION ( 'NONE',  ( -1.000000000000000000, 1.331116318405244905E-23, 4.759647537211363479E-16 ) ) ;
#1044 = AXIS2_PLACEMENT_3D ( 'NONE', #45099, #28976, #17429 ) ;
#1045 = VERTEX_POINT ( 'NONE', #32667 ) ;
#1046 = DIRECTION ( 'NONE',  ( 0.000000000000000000, 0.000000000000000000, 1.000000000000000000 ) ) ;
#1047 = PLANE ( 'NONE',  #45564 ) ;
#1048 = CARTESIAN_POINT ( 'NONE',  ( -35.51846793572368455, 35.99772139009146343, 7.906207997025717304 ) ) ;
#1049 = VERTEX_POINT ( 'NONE', #48515 ) ;
#1050 = ORIENTED_EDGE ( 'NONE', *, *, #34971, .T. ) ;
#1051 = ITEM_DEFINED_TRANSFORMATION ( 'NONE', 'NONE', #27478,  #30773 ) ;
#1052 = CARTESIAN_POINT ( 'NONE',  ( -168.4459734468149747, 0.000000000000000000, 162.5682875569279702 ) ) ;
#1053 = DIRECTION ( 'NONE',  ( 0.000000000000000000, -2.537652627714643577E-15, -1.000000000000000000 ) ) ;
#1054 = EDGE_CURVE ( 'NONE', #43553, #14725, #7925, .T. ) ;
#1055 = CARTESIAN_POINT ( 'NONE',  ( 191.5540265531850537, 1.025126265847089435, 39.06828755692797728 ) ) ;
#1056 = CARTESIAN_POINT ( 'NONE',  ( 183.0000000000000000, -164.9999999999999432, -344.0000000000001137 ) ) ;
#1057 = DIRECTION ( 'NONE',  ( 0.000000000000000000, -0.000000000000000000, -1.000000000000000000 ) ) ;
#1058 = VERTEX_POINT ( 'NONE', #40863 ) ;
#1059 = CARTESIAN_POINT ( 'NONE',  ( 210.0000000000000568, 2.143131898507881856E-16, 119.0682875569279560 ) ) ;
#1060 = EDGE_CURVE ( 'NONE', #41472, #40281, #17516, .T. ) ;
#1061 = VECTOR ( 'NONE', #15986, 1000.000000000000000 ) ;
#1062 = CARTESIAN_POINT ( 'NONE',  ( -206.6959734468149463, -1.750000000000009992, 160.8182875569279702 ) ) ;
#1063 = PLANE ( 'NONE',  #31580 ) ;
#1064 = EDGE_CURVE ( 'NONE', #18038, #23733, #24471, .T. ) ;
#1065 = CARTESIAN_POINT ( 'NONE',  ( 0.000000000000000000, -184.9999999999999716, -344.0000000000001705 ) ) ;
#1066 = EDGE_CURVE ( 'NONE', #38528, #20059, #40122, .T. ) ;
#1067 = ORIENTED_EDGE ( 'NONE', *, *, #11385, .F. ) ;
#1068 = CARTESIAN_POINT ( 'NONE',  ( 193.3040265531851105, -1.750000000000010658, 120.8182875569279702 ) ) ;
#1069 = VERTEX_POINT ( 'NONE', #12649 ) ;
#1070 = CARTESIAN_POINT ( 'NONE',  ( 0.3370904143228924954, 0.2449105217885333141, 10.00000000000000000 ) ) ;
#1071 = ORIENTED_EDGE ( 'NONE', *, *, #6720, .F. ) ;
#1072 = DIRECTION ( 'NONE',  ( -0.000000000000000000, -0.000000000000000000, -1.000000000000000000 ) ) ;
#1073 = VECTOR ( 'NONE', #36151, 1000.000000000000114 ) ;
#1074 = CARTESIAN_POINT ( 'NONE',  ( 18.67411147745603373, 27.51799019669827473, -3.760136334089591248 ) ) ;
#1075 = CARTESIAN_POINT ( 'NONE',  ( -205.6708471809678827, 1.750000000000009548, -158.1565861772249377 ) ) ;
#1076 = DIRECTION ( 'NONE',  ( -4.996003610813203446E-16, -1.000000000000000000, 0.000000000000000000 ) ) ;
#1077 = ORIENTED_EDGE ( 'NONE', *, *, #44672, .T. ) ;
#1078 =( GEOMETRIC_REPRESENTATION_CONTEXT ( 3 ) GLOBAL_UNCERTAINTY_ASSIGNED_CONTEXT ( ( #42989 ) ) GLOBAL_UNIT_ASSIGNED_CONTEXT ( ( #15335, #42505, #10210 ) ) REPRESENTATION_CONTEXT ( 'NONE', 'WORKASPACE' ) );
#1079 = DIRECTION ( 'NONE',  ( -1.000000000000000000, 0.000000000000000000, -2.958228394578794270E-31 ) ) ;
#1080 = VECTOR ( 'NONE', #22199, 1000.000000000000000 ) ;
#1081 = ORIENTED_EDGE ( 'NONE', *, *, #27876, .T. ) ;
#1082 = FACE_OUTER_BOUND ( 'NONE', #44486, .T. ) ;
#1083 = CARTESIAN_POINT ( 'NONE',  ( -5.670847180967843570, 1.750000000000022871, -160.2068387089191219 ) ) ;
#1084 = LINE ( 'NONE', #28024, #34432 ) ;
#1085 = DIRECTION ( 'NONE',  ( -0.000000000000000000, -0.000000000000000000, -1.000000000000000000 ) ) ;
#1086 = ORIENTED_EDGE ( 'NONE', *, *, #37198, .T. ) ;
#1088 = ORIENTED_EDGE ( 'NONE', *, *, #677, .F. ) ;
#1087 = ADVANCED_FACE ( 'NONE', ( #36286 ), #10893, .T. ) ;
#1089 = CARTESIAN_POINT ( 'NONE',  ( 8.176860274785711979, -5.756644512789521606, 9.282506307616484875 ) ) ;
#1090 = EDGE_CURVE ( 'NONE', #32291, #24319, #41871, .T. ) ;
#1091 = B_SPLINE_CURVE_WITH_KNOTS ( 'NONE', 3,
 ( #48534, #44212, #9084, #24739 ),
 .UNSPECIFIED., .F., .F.,
 ( 4, 4 ),
 ( 0.9688112071879400045, 0.9724175925769219520 ),
 .UNSPECIFIED. ) ;
#1092 = EDGE_CURVE ( 'NONE', #21408, #45663, #19109, .T. ) ;
#1093 = EDGE_CURVE ( 'NONE', #47298, #26902, #31284, .T. ) ;
#1094 = EDGE_LOOP ( 'NONE', ( #46101, #20220, #8122, #7542, #28111, #7098 ) ) ;
#1095 = CARTESIAN_POINT ( 'NONE',  ( 33.30402655318503946, 0.000000000000000000, 165.0000000000000000 ) ) ;
#1096 = DIRECTION ( 'NONE',  ( 1.000000000000000000, -0.000000000000000000, -0.000000000000000000 ) ) ;
#1097 = DIRECTION ( 'NONE',  ( 0.000000000000000000, 0.000000000000000000, -1.000000000000000000 ) ) ;
#1098 =( BOUNDED_CURVE ( )  B_SPLINE_CURVE ( 3, ( #43625, #11841, #40298, #12329 ),
 .UNSPECIFIED., .F., .F. ) 
 B_SPLINE_CURVE_WITH_KNOTS ( ( 4, 4 ),
 ( 0.000000000000000000, 1.570796326794896558 ),
 .UNSPECIFIED. ) 
 CURVE ( )  GEOMETRIC_REPRESENTATION_ITEM ( )  RATIONAL_B_SPLINE_CURVE ( ( 1.000000000000000000, 0.8047378541243649375, 0.8047378541243649375, 1.000000000000000000 ) ) 
 REPRESENTATION_ITEM ( '' )  );
#1099 = ORIENTED_EDGE ( 'NONE', *, *, #42448, .F. ) ;
#1100 = CARTESIAN_POINT ( 'NONE',  ( -0.02998614097933045841, -1.600097392939481056, 9.919954280166498606 ) ) ;
#1101 = EDGE_CURVE ( 'NONE', #1605, #16604, #6463, .T. ) ;
#1102 = EDGE_CURVE ( 'NONE', #9708, #15072, #33683, .T. ) ;
#1103 = CARTESIAN_POINT ( 'NONE',  ( 111.5540265531850679, 0.000000000000000000, 79.06828755692798438 ) ) ;
#1104 = CARTESIAN_POINT ( 'NONE',  ( -7.203307948779601233, 6.979912421814565171, 9.516222621873129839 ) ) ;
#1105 = LINE ( 'NONE', #32921, #6079 ) ;
#1106 = FACE_OUTER_BOUND ( 'NONE', #15806, .T. ) ;
#1107 = VERTEX_POINT ( 'NONE', #14152 ) ;
#1108 = VERTEX_POINT ( 'NONE', #30327 ) ;
#1109 = CIRCLE ( 'NONE', #39605, 4.000000000000003553 ) ;
#1110 = EDGE_LOOP ( 'NONE', ( #43754, #46043, #30091, #454, #22015, #22407 ) ) ;
#1111 = LINE ( 'NONE', #9059, #11588 ) ;
#1112 = CIRCLE ( 'NONE', #1913, 1.749999999999987566 ) ;
#1113 = CARTESIAN_POINT ( 'NONE',  ( -6.695973446814940111, -1.750000000000024203, 80.81828755692798438 ) ) ;
#1114 = CARTESIAN_POINT ( 'NONE',  ( -6.695973446814940111, -1.750000000000023315, 0.8182875569279768335 ) ) ;
#1115 = VERTEX_POINT ( 'NONE', #45936 ) ;
#1116 = EDGE_CURVE ( 'NONE', #10525, #16010, #26971, .T. ) ;
#1117 = EDGE_CURVE ( 'NONE', #323, #20716, #47031, .T. ) ;
#1118 = MECHANICAL_DESIGN_GEOMETRIC_PRESENTATION_REPRESENTATION (  '', ( #6856 ), #35553 ) ;
#1119 = CARTESIAN_POINT ( 'NONE',  ( 0.3862712429686894766, -1.188820645368940276, -10.00000000000000000 ) ) ;
#1120 = EDGE_LOOP ( 'NONE', ( #7077, #35444, #31188, #7911, #45465, #8066 ) ) ;
#1121 = DIRECTION ( 'NONE',  ( 0.9999999999999998890, 0.000000000000000000, 0.000000000000000000 ) ) ;
#1122 = CARTESIAN_POINT ( 'NONE',  ( 350.0000000000000000, -166.9999999999999432, -356.0000000000002274 ) ) ;
#1123 = DIRECTION ( 'NONE',  ( -1.000000000000000000, 0.000000000000000000, 1.860490536778032451E-50 ) ) ;
#1124 = DIRECTION ( 'NONE',  ( -1.860490536778032451E-50, 0.000000000000000000, 1.000000000000000000 ) ) ;
#1125 = ADVANCED_FACE ( 'NONE', ( #2606 ), #42111, .T. ) ;
#1126 = EDGE_CURVE ( 'NONE', #11740, #19783, #18760, .T. ) ;
#1127 = AXIS2_PLACEMENT_3D ( 'NONE', #37314, #21123, #10080 ) ;
#1128 = FACE_OUTER_BOUND ( 'NONE', #22979, .T. ) ;
#1129 = CARTESIAN_POINT ( 'NONE',  ( -168.4459734468149747, 2.143131898507880377E-16, -160.9317124430720298 ) ) ;
#1130 = CARTESIAN_POINT ( 'NONE',  ( -27.73884755486766096, 25.23502201956265978, 7.697694107796191787 ) ) ;
#1131 = ORIENTED_EDGE ( 'NONE', *, *, #31229, .T. ) ;
#1132 = CARTESIAN_POINT ( 'NONE',  ( 183.0000000000000000, -5.999999999999950262, -350.0000000000001705 ) ) ;
#1133 = B_SPLINE_SURFACE_WITH_KNOTS ( 'NONE', 3, 3, ( 
 ( #2109, #17756, #29306, #17252 ),
 ( #33174, #21344, #17500, #24707 ),
 ( #40843, #16997, #1357, #9550 ),
 ( #40354, #36519, #21865, #49253 ) ),
 .UNSPECIFIED., .F., .F., .F.,
 ( 4, 4 ),
 ( 4, 4 ),
 ( 0.000000000000000000, 1.000000000000000000 ),
 ( 0.000000000000000000, 1.000000000000000000 ),
 .UNSPECIFIED. ) ;
#1134 = CARTESIAN_POINT ( 'NONE',  ( -48.33712804702535237, -13.03701565032741705, -9.367992836599951190 ) ) ;
#1135 = DIRECTION ( 'NONE',  ( -1.000000000000000000, 0.000000000000000000, 0.000000000000000000 ) ) ;
#1136 = VECTOR ( 'NONE', #49570, 1000.000000000000000 ) ;
#1137 = CARTESIAN_POINT ( 'NONE',  ( 49.46074318306830975, -9.578883844006833570, 8.807470649214879543 ) ) ;
#1138 = EDGE_LOOP ( 'NONE', ( #3171, #13323, #12762, #33669 ) ) ;
#1139 = CARTESIAN_POINT ( 'NONE',  ( 195.0540265531851105, 2.143131898507880377E-16, -40.93171244307202983 ) ) ;
#1140 = ORIENTED_EDGE ( 'NONE', *, *, #36191, .F. ) ;
#1141 = EDGE_CURVE ( 'NONE', #23855, #44104, #48772, .T. ) ;
#1142 = CARTESIAN_POINT ( 'NONE',  ( 210.0000000000000568, 2.143131898507881856E-16, 79.06828755692797017 ) ) ;
#1143 = CARTESIAN_POINT ( 'NONE',  ( 10.00000000000000000, -250.0000000000000000, 225.0000000000000000 ) ) ;
#1144 = ORIENTED_EDGE ( 'NONE', *, *, #37806, .T. ) ;
#1145 = CARTESIAN_POINT ( 'NONE',  ( 111.5540265531850537, -1.025126265847082108, 82.56828755692798438 ) ) ;
#1146 = CARTESIAN_POINT ( 'NONE',  ( 344.0000000000000000, 165.0000000000000000, -340.0000000000001137 ) ) ;
#1147 = VECTOR ( 'NONE', #17968, 1000.000000000000000 ) ;
#1148 = EDGE_CURVE ( 'NONE', #30975, #45021, #10068, .T. ) ;
#1149 = CARTESIAN_POINT ( 'NONE',  ( -88.44597344681497475, 0.000000000000000000, -37.43171244307200141 ) ) ;
#1150 = DIRECTION ( 'NONE',  ( 0.000000000000000000, 0.000000000000000000, 1.000000000000000000 ) ) ;
#1151 = ORIENTED_EDGE ( 'NONE', *, *, #23396, .F. ) ;
#1152 = ORIENTED_EDGE ( 'NONE', *, *, #2044, .F. ) ;
#1153 = LINE ( 'NONE', #40404, #2135 ) ;
#1154 = VECTOR ( 'NONE', #48411, 1000.000000000000000 ) ;
#1155 = CARTESIAN_POINT ( 'NONE',  ( 2.499999999999956035, -194.9999999999999716, -224.9999999999999716 ) ) ;
#1156 = VECTOR ( 'NONE', #18949, 1000.000000000000000 ) ;
#1157 =( BOUNDED_CURVE ( )  B_SPLINE_CURVE ( 3, ( #28676, #45302, #25091, #40741 ),
 .UNSPECIFIED., .F., .F. ) 
 B_SPLINE_CURVE_WITH_KNOTS ( ( 4, 4 ),
 ( 3.141592653589793116, 4.712388980384689674 ),
 .UNSPECIFIED. ) 
 CURVE ( )  GEOMETRIC_REPRESENTATION_ITEM ( )  RATIONAL_B_SPLINE_CURVE ( ( 1.000000000000000000, 0.8047378541243649375, 0.8047378541243649375, 1.000000000000000000 ) ) 
 REPRESENTATION_ITEM ( '' )  );
#1158 = ADVANCED_FACE ( 'NONE', ( #25983 ), #18252, .T. ) ;
#1159 = EDGE_CURVE ( 'NONE', #9081, #16392, #13856, .T. ) ;
#1160 = ORIENTED_EDGE ( 'NONE', *, *, #3882, .F. ) ;
#1161 = VERTEX_POINT ( 'NONE', #21613 ) ;
#1162 = PLANE ( 'NONE',  #7566 ) ;
#1163 = LINE ( 'NONE', #28851, #47055 ) ;
#1164 = CARTESIAN_POINT ( 'NONE',  ( 44.99506233596247995, 23.32283626942318833, 7.455576670931136185 ) ) ;
#1165 = CARTESIAN_POINT ( 'NONE',  ( -124.9459734468149321, 1.025126265847081442, -160.9317124430720014 ) ) ;
#1166 = ORIENTED_EDGE ( 'NONE', *, *, #19540, .F. ) ;
#1167 = ORIENTED_EDGE ( 'NONE', *, *, #38891, .F. ) ;
#1168 = EDGE_LOOP ( 'NONE', ( #24157, #47816, #45794, #1614, #31460, #48514 ) ) ;
#1169 =( BOUNDED_CURVE ( )  B_SPLINE_CURVE ( 3, ( #25913, #29750, #33611, #45623 ),
 .UNSPECIFIED., .F., .F. ) 
 B_SPLINE_CURVE_WITH_KNOTS ( ( 4, 4 ),
 ( 3.141592653589793116, 4.712388980384689674 ),
 .UNSPECIFIED. ) 
 CURVE ( )  GEOMETRIC_REPRESENTATION_ITEM ( )  RATIONAL_B_SPLINE_CURVE ( ( 1.000000000000000000, 0.8047378541243649375, 0.8047378541243649375, 1.000000000000000000 ) ) 
 REPRESENTATION_ITEM ( '' )  );
#1170 = EDGE_CURVE ( 'NONE', #15638, #28163, #46956, .T. ) ;
#1171 = EDGE_CURVE ( 'NONE', #24437, #48718, #17769, .T. ) ;
#1172 = CARTESIAN_POINT ( 'NONE',  ( -0.1287570809895602630, -0.3962735484563142396, 10.00000000000000000 ) ) ;
#1173 = EDGE_CURVE ( 'NONE', #7223, #5437, #15181, .T. ) ;
#1174 = VECTOR ( 'NONE', #42245, 1000.000000000000000 ) ;
#1175 = FACE_OUTER_BOUND ( 'NONE', #4354, .T. ) ;
#1176 = ORIENTED_EDGE ( 'NONE', *, *, #32433, .T. ) ;
#1177 = VERTEX_POINT ( 'NONE', #50018 ) ;
#1178 = EDGE_CURVE ( 'NONE', #36229, #829, #36440, .T. ) ;
#1179 = CARTESIAN_POINT ( 'NONE',  ( 210.0000000000000568, 0.000000000000000000, -39.18171244307202983 ) ) ;
#1180 = VERTEX_POINT ( 'NONE', #43137 ) ;
#1181 = ORIENTED_EDGE ( 'NONE', *, *, #33713, .F. ) ;
#1182 = SPHERICAL_SURFACE ( 'NONE', #12671, 0.5000000000000000000 ) ;
#1183 = FILL_AREA_STYLE ('',( #36341 ) ) ;
#1184 = EDGE_LOOP ( 'NONE', ( #33562, #16368, #48239, #12425, #6053, #20848 ) ) ;
#1185 = CARTESIAN_POINT ( 'NONE',  ( 168.9999999999999716, 165.0000000000000000, -342.0000000000001137 ) ) ;
#1186 = FACE_BOUND ( 'NONE', #10121, .T. ) ;
#1187 = DIRECTION ( 'NONE',  ( 0.000000000000000000, -1.000000000000000000, 3.186989995019654210E-49 ) ) ;
#1188 = EDGE_CURVE ( 'NONE', #25957, #49918, #41661, .T. ) ;
#1189 = VECTOR ( 'NONE', #4370, 1000.000000000000000 ) ;
#1190 = DIRECTION ( 'NONE',  ( 0.000000000000000000, -1.000000000000000000, 2.537652627714643577E-15 ) ) ;
#1191 = ORIENTED_EDGE ( 'NONE', *, *, #21634, .T. ) ;
#1192 = AXIS2_PLACEMENT_3D ( 'NONE', #40576, #16973, #37010 ) ;
#1193 = CARTESIAN_POINT ( 'NONE',  ( -0.3862712429686809279, -1.188820645368943163, 3.333333333333333481 ) ) ;
#1194 = DIRECTION ( 'NONE',  ( 0.000000000000000000, 0.000000000000000000, 1.000000000000000000 ) ) ;
#1195 = CARTESIAN_POINT ( 'NONE',  ( 35.00000000000122213, 17.00000000000000000, 5.000000000000004441 ) ) ;
#1196 = AXIS2_PLACEMENT_3D ( 'NONE', #1796, #2048, #11002 ) ;
#1197 = DIRECTION ( 'NONE',  ( 0.000000000000000000, -0.000000000000000000, 1.000000000000000000 ) ) ;
#1198 = B_SPLINE_CURVE_WITH_KNOTS ( 'NONE', 3,
 ( #4713, #28057, #44689, #20352 ),
 .UNSPECIFIED., .F., .F.,
 ( 4, 4 ),
 ( 0.000000000000000000, 0.002368422649471283413 ),
 .UNSPECIFIED. ) ;
#1199 = CARTESIAN_POINT ( 'NONE',  ( 193.3040265531851105, -1.750000000000009992, 0.8182875569279768335 ) ) ;
#1200 = CARTESIAN_POINT ( 'NONE',  ( -0.8155877869437639927, -0.9072449372115535260, 9.963925895596188909 ) ) ;
#1201 = CARTESIAN_POINT ( 'NONE',  ( -2.052549611693787135, 0.2039603569406744088, 9.894754715216729224 ) ) ;
#1202 = DIRECTION ( 'NONE',  ( 0.000000000000000000, 0.000000000000000000, -1.000000000000000000 ) ) ;
#1203 = ORIENTED_EDGE ( 'NONE', *, *, #7025, .F. ) ;
#1204 = AXIS2_PLACEMENT_3D ( 'NONE', #26739, #7748, #19015 ) ;
#1205 = PLANE ( 'NONE',  #27858 ) ;
#1206 = AXIS2_PLACEMENT_3D ( 'NONE', #1940, #6300, #16138 ) ;
#1207 = VERTEX_POINT ( 'NONE', #42867 ) ;
#1208 = CARTESIAN_POINT ( 'NONE',  ( 153.3040265531850537, 0.000000000000000000, 165.0000000000000000 ) ) ;
#1209 = CARTESIAN_POINT ( 'NONE',  ( 0.3370904143228924954, 0.2449105217885333141, 10.00000000000000000 ) ) ;
#1210 = CARTESIAN_POINT ( 'NONE',  ( 343.9999999999999432, 183.0000000000002274, -358.0000000000003411 ) ) ;
#1211 = VERTEX_POINT ( 'NONE', #8004 ) ;
#1212 = CYLINDRICAL_SURFACE ( 'NONE', #9348, 1.750000000000001554 ) ;
#1213 = EDGE_LOOP ( 'NONE', ( #23628, #22154, #10733 ) ) ;
#1214 = ORIENTED_EDGE ( 'NONE', *, *, #24898, .F. ) ;
#1215 = CARTESIAN_POINT ( 'NONE',  ( 2.945500763482279627, 16.64098165802040086, -9.008049429158100807 ) ) ;
#1216 = CARTESIAN_POINT ( 'NONE',  ( -194.9999999999999432, 173.0000000000000000, 372.0000000000000000 ) ) ;
#1217 = EDGE_CURVE ( 'NONE', #29584, #33010, #8647, .T. ) ;
#1218 = EDGE_CURVE ( 'NONE', #14253, #1522, #27244, .T. ) ;
#1219 = ORIENTED_EDGE ( 'NONE', *, *, #14868, .T. ) ;
#1220 = CARTESIAN_POINT ( 'NONE',  ( 35.00000000000091660, 16.00000000000000000, -24.99999999999999289 ) ) ;
#1221 = CARTESIAN_POINT ( 'NONE',  ( -126.6959734468149321, 0.000000000000000000, 165.0000000000000000 ) ) ;
#1222 = AXIS2_PLACEMENT_3D ( 'NONE', #1095, #37459, #12621 ) ;
#1223 = EDGE_LOOP ( 'NONE', ( #7970, #34321, #34358, #11048, #18357 ) ) ;
#1224 = ORIENTED_EDGE ( 'NONE', *, *, #47145, .F. ) ;
#1225 = EDGE_CURVE ( 'NONE', #46658, #3850, #26979, .T. ) ;
#1226 = CARTESIAN_POINT ( 'NONE',  ( 3.798817505216071755, 5.709742178110386313, 9.753789706659947711 ) ) ;
#1227 = ORIENTED_EDGE ( 'NONE', *, *, #36593, .T. ) ;
#1228 = AXIS2_PLACEMENT_3D ( 'NONE', #19135, #50138, #31468 ) ;
#1230 = EDGE_CURVE ( 'NONE', #27492, #45408, #11849, .T. ) ;
#1229 = CARTESIAN_POINT ( 'NONE',  ( -1.066995270233474624, 33.23888904628638841, -3.760136334089591248 ) ) ;
#1231 = EDGE_CURVE ( 'NONE', #28520, #3732, #42617, .T. ) ;
#1232 = CARTESIAN_POINT ( 'NONE',  ( 14.49999999999999822, 12.98684210526315930, 19.37312575500899925 ) ) ;
#1233 = ORIENTED_EDGE ( 'NONE', *, *, #50556, .T. ) ;
#1234 = DIRECTION ( 'NONE',  ( -0.000000000000000000, -1.000000000000000000, -0.000000000000000000 ) ) ;
#1235 = CARTESIAN_POINT ( 'NONE',  ( 5.888214538810389698, 16.20866436362417673, 8.727788335465566760 ) ) ;
#1236 = EDGE_LOOP ( 'NONE', ( #22817, #30759, #48688, #4298 ) ) ;
#1237 = VERTEX_POINT ( 'NONE', #11074 ) ;
#1238 = ORIENTED_EDGE ( 'NONE', *, *, #31217, .T. ) ;
#1239 = DIRECTION ( 'NONE',  ( 0.000000000000000000, 1.000000000000000000, -1.604368532695312981E-16 ) ) ;
#1240 = EDGE_CURVE ( 'NONE', #38020, #13837, #23637, .T. ) ;
#1241 = EDGE_CURVE ( 'NONE', #44363, #9118, #17083, .T. ) ;
#1242 = CARTESIAN_POINT ( 'NONE',  ( 5.551115123125782702E-14, -168.9999999999999432, 355.9999999999997726 ) ) ;
#1243 = EDGE_LOOP ( 'NONE', ( #50125, #24001, #26640, #3951, #38835, #44398 ) ) ;
#1244 = FACE_OUTER_BOUND ( 'NONE', #11101, .T. ) ;
#1245 = LINE ( 'NONE', #9175, #17393 ) ;
#1246 = DIRECTION ( 'NONE',  ( -1.000000000000000000, -0.000000000000000000, -0.000000000000000000 ) ) ;
#1247 = FACE_OUTER_BOUND ( 'NONE', #4168, .T. ) ;
#1248 = CARTESIAN_POINT ( 'NONE',  ( 44.94002984196458073, 9.722063056714072005, -8.016098858316205167 ) ) ;
#1249 = DIRECTION ( 'NONE',  ( -0.000000000000000000, -0.000000000000000000, 1.000000000000000000 ) ) ;
#1250 = VECTOR ( 'NONE', #8517, 1000.000000000000000 ) ;
#1251 = CARTESIAN_POINT ( 'NONE',  ( -194.9999999999999432, 173.0000000000000000, 352.0000000000000000 ) ) ;
#1252 = DIRECTION ( 'NONE',  ( -0.000000000000000000, -1.000000000000000000, -0.000000000000000000 ) ) ;
#1253 = DIRECTION ( 'NONE',  ( -0.000000000000000000, -0.000000000000000000, -1.000000000000000000 ) ) ;
#1254 = DIRECTION ( 'NONE',  ( 1.586032880504786307E-16, -1.654361225106055350E-24, 1.000000000000000000 ) ) ;
#1255 = DIRECTION ( 'NONE',  ( 0.000000000000000000, 0.000000000000000000, 1.000000000000000000 ) ) ;
#1256 = AXIS2_PLACEMENT_3D ( 'NONE', #22784, #50179, #26889 ) ;
#1257 = CARTESIAN_POINT ( 'NONE',  ( 193.3040265531851105, -1.750000000000009992, 160.8182875569279702 ) ) ;
#1258 = ORIENTED_EDGE ( 'NONE', *, *, #41775, .T. ) ;
#1259 = CARTESIAN_POINT ( 'NONE',  ( -0.6721397084974984892, -9.977385840602783773, 0.000000000000000000 ) ) ;
#1260 = LINE ( 'NONE', #5343, #40134 ) ;
#1261 = CARTESIAN_POINT ( 'NONE',  ( -8.760073316077686911, -197.4999999999999432, -228.6347188485896140 ) ) ;
#1262 = AXIS2_PLACEMENT_3D ( 'NONE', #20041, #39056, #46440 ) ;
#1263 = VECTOR ( 'NONE', #19839, 1000.000000000000000 ) ;
#1264 = LINE ( 'NONE', #17150, #43490 ) ;
#1265 = EDGE_CURVE ( 'NONE', #1473, #46979, #43333, .T. ) ;
#1266 = EDGE_LOOP ( 'NONE', ( #10992, #14682, #46915, #45929 ) ) ;
#1267 = CARTESIAN_POINT ( 'NONE',  ( -126.6959734468149321, 1.749999999999997335, -79.18171244307201562 ) ) ;
#1268 = DIRECTION ( 'NONE',  ( 0.000000000000000000, 0.000000000000000000, 1.000000000000000000 ) ) ;
#1269 = ORIENTED_EDGE ( 'NONE', *, *, #4630, .T. ) ;
#1270 = FACE_OUTER_BOUND ( 'NONE', #33337, .T. ) ;
#1271 = CARTESIAN_POINT ( 'NONE',  ( 181.0000000000000000, -95.49999999999998579, -340.0000000000001137 ) ) ;
#1272 = ORIENTED_EDGE ( 'NONE', *, *, #4241, .T. ) ;
#1273 = LINE ( 'NONE', #24619, #10109 ) ;
#1274 = ORIENTED_EDGE ( 'NONE', *, *, #16711, .T. ) ;
#1275 = EDGE_LOOP ( 'NONE', ( #17040, #2179, #4711 ) ) ;
#1276 = VECTOR ( 'NONE', #31120, 1000.000000000000000 ) ;
#1277 = VERTEX_POINT ( 'NONE', #31354 ) ;
#1278 = DIRECTION ( 'NONE',  ( 0.000000000000000000, 0.000000000000000000, -1.000000000000000000 ) ) ;
#1279 = CARTESIAN_POINT ( 'NONE',  ( 73.30402655318508209, 1.750000000000010658, -79.18171244307201562 ) ) ;
#1280 = ORIENTED_EDGE ( 'NONE', *, *, #31121, .T. ) ;
#1281 = CARTESIAN_POINT ( 'NONE',  ( 339.9999999999999432, -180.9999999999999432, 355.9999999999998295 ) ) ;
#1282 = DIRECTION ( 'NONE',  ( -0.000000000000000000, -1.000000000000000000, -0.000000000000000000 ) ) ;
#1283 = DIRECTION ( 'NONE',  ( -1.586032892321652482E-16, 0.000000000000000000, -1.000000000000000000 ) ) ;
#1284 = VECTOR ( 'NONE', #35273, 1000.000000000000000 ) ;
#1285 = CARTESIAN_POINT ( 'NONE',  ( -17.51065725283106644, 28.41934970907792390, -9.367992836599951190 ) ) ;
#1286 = ORIENTED_EDGE ( 'NONE', *, *, #1126, .T. ) ;
#1287 = DIRECTION ( 'NONE',  ( 1.000000000000000000, 0.000000000000000000, 0.000000000000000000 ) ) ;
#1288 = ORIENTED_EDGE ( 'NONE', *, *, #47195, .F. ) ;
#1289 = CARTESIAN_POINT ( 'NONE',  ( 80.00000000000061107, 17.00000000000000000, -54.99999999999999289 ) ) ;
#1290 = CARTESIAN_POINT ( 'NONE',  ( 358.0000000000000568, -167.8284271247462982, -342.8284271247463835 ) ) ;
#1291 = VECTOR ( 'NONE', #33544, 1000.000000000000000 ) ;
#1292 = EDGE_LOOP ( 'NONE', ( #10870, #27472, #30423, #39009 ) ) ;
#1293 = ORIENTED_EDGE ( 'NONE', *, *, #18051, .F. ) ;
#1294 = CARTESIAN_POINT ( 'NONE',  ( -194.9999999999999432, -173.0000000000000000, 112.0000000000000284 ) ) ;
#1295 = EDGE_CURVE ( 'NONE', #17662, #44875, #38456, .T. ) ;
#1296 = CYLINDRICAL_SURFACE ( 'NONE', #33237, 1.750000000000015543 ) ;
#1297 = ORIENTED_EDGE ( 'NONE', *, *, #29279, .F. ) ;
#1298 = VECTOR ( 'NONE', #22249, 1000.000000000000000 ) ;
#1299 = CARTESIAN_POINT ( 'NONE',  ( 210.0000000000000568, 0.000000000000000000, 80.81828755692798438 ) ) ;
#1300 = DIRECTION ( 'NONE',  ( -1.000000000000000000, 0.000000000000000000, 0.000000000000000000 ) ) ;
#1301 = DIRECTION ( 'NONE',  ( 0.000000000000000000, 1.000000000000000000, 0.000000000000000000 ) ) ;
#1302 =( BOUNDED_CURVE ( )  B_SPLINE_CURVE ( 3, ( #10478, #2526, #13567, #6129 ),
 .UNSPECIFIED., .F., .F. ) 
 B_SPLINE_CURVE_WITH_KNOTS ( ( 4, 4 ),
 ( 3.141592653589793116, 4.712388980384689674 ),
 .UNSPECIFIED. ) 
 CURVE ( )  GEOMETRIC_REPRESENTATION_ITEM ( )  RATIONAL_B_SPLINE_CURVE ( ( 1.000000000000000000, 0.8047378541243649375, 0.8047378541243649375, 1.000000000000000000 ) ) 
 REPRESENTATION_ITEM ( '' )  );
#1303 = CARTESIAN_POINT ( 'NONE',  ( 7.359817328027030925, 15.16751262232805431, 2.590526750877053086 ) ) ;
#1304 = ORIENTED_EDGE ( 'NONE', *, *, #7631, .F. ) ;
#1305 = CARTESIAN_POINT ( 'NONE',  ( 30.00000000000123279, 17.00000000000000000, 5.000000000000004441 ) ) ;
#1306 = CARTESIAN_POINT ( 'NONE',  ( 1.081517186030698241, -0.5722085955955613645, 9.993783931180535873 ) ) ;
#1307 =( BOUNDED_CURVE ( )  B_SPLINE_CURVE ( 3, ( #25709, #38540, #45167, #41355 ),
 .UNSPECIFIED., .F., .F. ) 
 B_SPLINE_CURVE_WITH_KNOTS ( ( 4, 4 ),
 ( 1.570796326794896558, 3.141592653589793116 ),
 .UNSPECIFIED. ) 
 CURVE ( )  GEOMETRIC_REPRESENTATION_ITEM ( )  RATIONAL_B_SPLINE_CURVE ( ( 1.000000000000000000, 0.8047378541243649375, 0.8047378541243649375, 1.000000000000000000 ) ) 
 REPRESENTATION_ITEM ( '' )  );
#1308 = CARTESIAN_POINT ( 'NONE',  ( 19.61585174098975770, -31.96834229807152283, -9.011255500499643745 ) ) ;
#1309 = ORIENTED_EDGE ( 'NONE', *, *, #16925, .F. ) ;
#1310 = ORIENTED_EDGE ( 'NONE', *, *, #255, .T. ) ;
#1311 = SHAPE_DEFINITION_REPRESENTATION ( #4067, #13952 ) ;
#1312 = CARTESIAN_POINT ( 'NONE',  ( -5.000000000000000000, -165.1999999999999602, -340.2000000000001592 ) ) ;
#1313 = CARTESIAN_POINT ( 'NONE',  ( 114.3291528190321173, -1.749999999999996669, -78.15658617722492352 ) ) ;
#1314 = VECTOR ( 'NONE', #13309, 1000.000000000000114 ) ;
#1316 = CIRCLE ( 'NONE', #14411, 2.000000000000001776 ) ;
#1315 = CARTESIAN_POINT ( 'NONE',  ( 341.9999999999999432, -169.0000000000001705, 344.0000000000000568 ) ) ;
#1317 = DIRECTION ( 'NONE',  ( -1.000000000000000000, 4.996003610813203446E-16, 1.586032878436834529E-16 ) ) ;
#1318 = ORIENTED_EDGE ( 'NONE', *, *, #3537, .T. ) ;
#1319 = DIRECTION ( 'NONE',  ( -1.000000000000000000, -0.000000000000000000, -0.000000000000000000 ) ) ;
#1320 = VECTOR ( 'NONE', #10755, 1000.000000000000000 ) ;
#1321 =( BOUNDED_CURVE ( )  B_SPLINE_CURVE ( 3, ( #15247, #104, #47003, #15738 ),
 .UNSPECIFIED., .F., .F. ) 
 B_SPLINE_CURVE_WITH_KNOTS ( ( 4, 4 ),
 ( 0.000000000000000000, 1.570796326794896558 ),
 .UNSPECIFIED. ) 
 CURVE ( )  GEOMETRIC_REPRESENTATION_ITEM ( )  RATIONAL_B_SPLINE_CURVE ( ( 1.000000000000000000, 0.8047378541243649375, 0.8047378541243649375, 1.000000000000000000 ) ) 
 REPRESENTATION_ITEM ( '' )  );
#1322 = FACE_OUTER_BOUND ( 'NONE', #22327, .T. ) ;
#1323 = DIRECTION ( 'NONE',  ( -1.000000000000000000, 0.000000000000000000, 2.312964634635843537E-16 ) ) ;
#1324 = CARTESIAN_POINT ( 'NONE',  ( 192.2789002873380184, 1.750000000000009548, -40.20683870891912193 ) ) ;
#1325 = EDGE_CURVE ( 'NONE', #33108, #17487, #26735, .T. ) ;
#1326 = ORIENTED_EDGE ( 'NONE', *, *, #18380, .F. ) ;
#1327 = CARTESIAN_POINT ( 'NONE',  ( -44.94597344681493922, -1.025126265847089213, -0.9317124430720324924 ) ) ;
#1328 = EDGE_LOOP ( 'NONE', ( #49208, #8539, #2407, #30372, #15839 ) ) ;
#1329 = CARTESIAN_POINT ( 'NONE',  ( 13.59579750444771307, -10.60877755095900632, 8.727788335465566760 ) ) ;
#1330 = ORIENTED_EDGE ( 'NONE', *, *, #36328, .F. ) ;
#1331 = FACE_OUTER_BOUND ( 'NONE', #22843, .T. ) ;
#1332 = LINE ( 'NONE', #2322, #36429 ) ;
#1333 = LINE ( 'NONE', #12605, #28974 ) ;
#1334 = EDGE_LOOP ( 'NONE', ( #25696, #12876, #33436 ) ) ;
#1335 = AXIS2_PLACEMENT_3D ( 'NONE', #7844, #641, #27597 ) ;
#1336 = DIRECTION ( 'NONE',  ( -0.000000000000000000, -1.000000000000000000, -0.000000000000000000 ) ) ;
#1337 = ORIENTED_EDGE ( 'NONE', *, *, #38708, .T. ) ;
#1338 = CARTESIAN_POINT ( 'NONE',  ( 168.9999999999999716, -164.9999999999999432, -340.0000000000001705 ) ) ;
#1339 = CARTESIAN_POINT ( 'NONE',  ( -125.6708471809678542, -1.749999999999996669, -0.2068387089191042749 ) ) ;
#1340 = DIRECTION ( 'NONE',  ( -1.000000000000000000, 0.000000000000000000, 0.000000000000000000 ) ) ;
#1341 = LINE ( 'NONE', #1837, #13601 ) ;
#1342 = CARTESIAN_POINT ( 'NONE',  ( 168.9999999999999716, -168.9999999999999432, -340.0000000000001137 ) ) ;
#1343 = ORIENTED_EDGE ( 'NONE', *, *, #6034, .T. ) ;
#1344 = ORIENTED_EDGE ( 'NONE', *, *, #33713, .T. ) ;
#1345 = DIRECTION ( 'NONE',  ( 0.000000000000000000, 0.000000000000000000, -1.000000000000000000 ) ) ;
#1346 = ORIENTED_EDGE ( 'NONE', *, *, #8118, .F. ) ;
#1347 = VECTOR ( 'NONE', #6757, 1000.000000000000114 ) ;
#1348 = CARTESIAN_POINT ( 'NONE',  ( -165.0000000000000284, 17.00000000000000000, -90.00000000000000000 ) ) ;
#1349 = PLANE ( 'NONE',  #45547 ) ;
#1350 = DIRECTION ( 'NONE',  ( -1.000000000000000000, 0.000000000000000000, 0.000000000000000000 ) ) ;
#1351 = AXIS2_PLACEMENT_3D ( 'NONE', #46682, #786, #27229 ) ;
#1352 = ORIENTED_EDGE ( 'NONE', *, *, #24699, .T. ) ;
#1353 = DIRECTION ( 'NONE',  ( 0.000000000000000000, -1.224646799147352961E-16, 1.000000000000000000 ) ) ;
#1354 = EDGE_CURVE ( 'NONE', #16979, #715, #36101, .T. ) ;
#1355 = CARTESIAN_POINT ( 'NONE',  ( 71.55402655318505367, 1.025126265847089213, -160.9317124430720014 ) ) ;
#1356 = CARTESIAN_POINT ( 'NONE',  ( 5.083187235775197266, 8.611690166631179366, 9.646707543097347681 ) ) ;
#1357 = CARTESIAN_POINT ( 'NONE',  ( -15.98719783915689163, 4.501063718205989161, 3.266473740018926541 ) ) ;
#1358 = DIRECTION ( 'NONE',  ( -1.000000000000000000, 0.000000000000000000, 0.000000000000000000 ) ) ;
#1360 = VECTOR ( 'NONE', #42599, 1000.000000000000000 ) ;
#1359 = DIRECTION ( 'NONE',  ( 1.000000000000000000, 0.000000000000000000, 0.000000000000000000 ) ) ;
#1361 = ORIENTED_EDGE ( 'NONE', *, *, #3520, .F. ) ;
#1362 = B_SPLINE_CURVE_WITH_KNOTS ( 'NONE', 3,
 ( #23325, #18447, #23843, #46889 ),
 .UNSPECIFIED., .F., .F.,
 ( 4, 4 ),
 ( 0.000000000000000000, 0.2545280377015988749 ),
 .UNSPECIFIED. ) ;
#1363 = ORIENTED_EDGE ( 'NONE', *, *, #40965, .F. ) ;
#1364 =( BOUNDED_CURVE ( )  B_SPLINE_CURVE ( 3, ( #17997, #5699, #49762, #14661 ),
 .UNSPECIFIED., .F., .F. ) 
 B_SPLINE_CURVE_WITH_KNOTS ( ( 4, 4 ),
 ( 1.570796326794896558, 3.141592653589793116 ),
 .UNSPECIFIED. ) 
 CURVE ( )  GEOMETRIC_REPRESENTATION_ITEM ( )  RATIONAL_B_SPLINE_CURVE ( ( 1.000000000000000000, 0.8047378541243649375, 0.8047378541243649375, 1.000000000000000000 ) ) 
 REPRESENTATION_ITEM ( '' )  );
#1365 = AXIS2_PLACEMENT_3D ( 'NONE', #3048, #30262, #37722 ) ;
#1366 = ORIENTED_EDGE ( 'NONE', *, *, #27702, .T. ) ;
#1367 = DIRECTION ( 'NONE',  ( 0.000000000000000000, -1.000000000000000000, 0.000000000000000000 ) ) ;
#1368 = CARTESIAN_POINT ( 'NONE',  ( 356.0000000000000000, 183.0000000000000284, -358.0000000000002842 ) ) ;
#1369 = EDGE_CURVE ( 'NONE', #19789, #23031, #22321, .T. ) ;
#1370 = PLANE ( 'NONE',  #15035 ) ;
#1371 = EDGE_CURVE ( 'NONE', #10844, #33292, #12098, .T. ) ;
#1372 = FACE_OUTER_BOUND ( 'NONE', #38774, .T. ) ;
#1373 = ORIENTED_EDGE ( 'NONE', *, *, #32808, .T. ) ;
#1374 = CARTESIAN_POINT ( 'NONE',  ( 9.696760411815720460, 2.443938934556958653, 0.000000000000000000 ) ) ;
#1375 = ORIENTED_EDGE ( 'NONE', *, *, #9884, .F. ) ;
#1376 = ADVANCED_FACE ( 'NONE', ( #40059 ), #40304, .F. ) ;
#1377 = CARTESIAN_POINT ( 'NONE',  ( 5.325040722962521400, -2.676059336580344006, 7.623296525288703052E-16 ) ) ;
#1378 = DIRECTION ( 'NONE',  ( -1.612977847700450206E-50, 0.000000000000000000, -1.000000000000000000 ) ) ;
#1379 = CARTESIAN_POINT ( 'NONE',  ( 151.5540265531850537, -1.025126265847089435, 39.06828755692797728 ) ) ;
#1380 = DIRECTION ( 'NONE',  ( -0.000000000000000000, -0.000000000000000000, -1.000000000000000000 ) ) ;
#1381 = VERTEX_POINT ( 'NONE', #24160 ) ;
#1382 = DIRECTION ( 'NONE',  ( -1.000000000000000000, 0.000000000000000000, -0.000000000000000000 ) ) ;
#1383 = CARTESIAN_POINT ( 'NONE',  ( -48.44597344681495343, 0.000000000000000000, 79.06828755692797017 ) ) ;
#1384 = DIRECTION ( 'NONE',  ( -0.000000000000000000, -0.000000000000000000, -1.000000000000000000 ) ) ;
#1385 = EDGE_CURVE ( 'NONE', #16019, #47057, #49932, .T. ) ;
#1386 = ADVANCED_FACE ( 'NONE', ( #562 ), #28506, .F. ) ;
#1387 = EDGE_CURVE ( 'NONE', #48005, #43486, #12216, .T. ) ;
#1388 = EDGE_CURVE ( 'NONE', #559, #40360, #45760, .T. ) ;
#1389 = PRESENTATION_STYLE_ASSIGNMENT (( #16527 ) ) ;
#1391 = ORIENTED_EDGE ( 'NONE', *, *, #49902, .T. ) ;
#1390 = AXIS2_PLACEMENT_3D ( 'NONE', #45292, #10176, #42469 ) ;
#1392 = CARTESIAN_POINT ( 'NONE',  ( 71.55402655318505367, 1.025126265847089657, -80.93171244307201562 ) ) ;
#1393 = ORIENTED_EDGE ( 'NONE', *, *, #33518, .F. ) ;
#1394 = CARTESIAN_POINT ( 'NONE',  ( 356.0000000000000568, 185.0000000000001137, 359.9999999999998295 ) ) ;
#1395 = CARTESIAN_POINT ( 'NONE',  ( 210.0000000000000568, 2.143131898507880377E-16, 159.0682875569279702 ) ) ;
#1396 = EDGE_CURVE ( 'NONE', #41719, #15554, #13342, .T. ) ;
#1397 = LINE ( 'NONE', #5476, #31278 ) ;
#1398 = VERTEX_POINT ( 'NONE', #44129 ) ;
#1399 = CARTESIAN_POINT ( 'NONE',  ( 30.21887974406487487, -14.69854701517530060, -8.016098858316205167 ) ) ;
#1400 = DIRECTION ( 'NONE',  ( 0.000000000000000000, 0.000000000000000000, 1.000000000000000000 ) ) ;
#1401 =( BOUNDED_CURVE ( )  B_SPLINE_CURVE ( 3, ( #35197, #47685, #294, #11834 ),
 .UNSPECIFIED., .F., .F. ) 
 B_SPLINE_CURVE_WITH_KNOTS ( ( 4, 4 ),
 ( 3.141592653589793116, 4.712388980384689674 ),
 .UNSPECIFIED. ) 
 CURVE ( )  GEOMETRIC_REPRESENTATION_ITEM ( )  RATIONAL_B_SPLINE_CURVE ( ( 1.000000000000000000, 0.8047378541243649375, 0.8047378541243649375, 1.000000000000000000 ) ) 
 REPRESENTATION_ITEM ( '' )  );
#1402 = DIRECTION ( 'NONE',  ( 1.000000000000000000, 0.000000000000000000, -0.000000000000000000 ) ) ;
#1403 = DIRECTION ( 'NONE',  ( -1.000000000000000000, -0.000000000000000000, -0.000000000000000000 ) ) ;
#1404 = ORIENTED_EDGE ( 'NONE', *, *, #36761, .F. ) ;
#1405 = VERTEX_POINT ( 'NONE', #16688 ) ;
#1406 = ADVANCED_FACE ( 'NONE', ( #805 ), #5140, .T. ) ;
#1407 = CARTESIAN_POINT ( 'NONE',  ( -2.945500763482280959, -16.64098165802040086, -9.008049429158102583 ) ) ;
#1408 = VECTOR ( 'NONE', #18293, 1000.000000000000000 ) ;
#1409 = DIRECTION ( 'NONE',  ( 0.000000000000000000, 0.000000000000000000, 1.000000000000000000 ) ) ;
#1410 = EDGE_CURVE ( 'NONE', #28349, #13625, #22863, .T. ) ;
#1411 = ORIENTED_EDGE ( 'NONE', *, *, #17073, .T. ) ;
#1412 = ADVANCED_FACE ( 'NONE', ( #40805 ), #8763, .F. ) ;
#1413 = ORIENTED_EDGE ( 'NONE', *, *, #36701, .F. ) ;
#1414 = LINE ( 'NONE', #32464, #28071 ) ;
#1415 = CARTESIAN_POINT ( 'NONE',  ( 14.76429217231961566, 8.192625680377691566, 9.178419661560148768 ) ) ;
#1416 = CARTESIAN_POINT ( 'NONE',  ( -126.6959734468149321, 0.000000000000000000, 165.0000000000000000 ) ) ;
#1417 = APPLICATION_CONTEXT ( 'automotive_design' ) ;
#1418 = EDGE_LOOP ( 'NONE', ( #24828, #1884, #25493, #14264, #8599, #47070 ) ) ;
#1419 = ORIENTED_EDGE ( 'NONE', *, *, #15155, .F. ) ;
#1420 = EDGE_CURVE ( 'NONE', #29366, #26020, #29016, .T. ) ;
#1421 = ORIENTED_EDGE ( 'NONE', *, *, #38820, .F. ) ;
#1422 = EDGE_CURVE ( 'NONE', #29654, #38683, #36217, .T. ) ;
#1423 = DIRECTION ( 'NONE',  ( -1.000000000000000000, 0.000000000000000000, 0.000000000000000000 ) ) ;
#1424 = AXIS2_PLACEMENT_3D ( 'NONE', #27930, #20227, #24090 ) ;
#1425 = CARTESIAN_POINT ( 'NONE',  ( -25.63461350838931807, 43.17876197216396861, -8.016098858316199838 ) ) ;
#1426 = VERTEX_POINT ( 'NONE', #1312 ) ;
#1427 = ORIENTED_EDGE ( 'NONE', *, *, #38703, .F. ) ;
#1428 = CARTESIAN_POINT ( 'NONE',  ( 360.0000000000000000, 169.0000000000000000, -344.0000000000001705 ) ) ;
#1429 = CARTESIAN_POINT ( 'NONE',  ( -556.8973046169135159, 54.43801056904003133, -64.63743994998280584 ) ) ;
#1430 = ORIENTED_EDGE ( 'NONE', *, *, #1388, .F. ) ;
#1431 = ORIENTED_EDGE ( 'NONE', *, *, #5538, .T. ) ;
#1432 = CARTESIAN_POINT ( 'NONE',  ( -239.0000000000000853, -153.6999999999999602, 250.3600000000000136 ) ) ;
#1433 = CARTESIAN_POINT ( 'NONE',  ( 0.1287570809895604018, 0.3962735484563146282, -10.00000000000000000 ) ) ;
#1434 = VERTEX_POINT ( 'NONE', #1052 ) ;
#1435 = PLANE ( 'NONE',  #19680 ) ;
#1436 = CARTESIAN_POINT ( 'NONE',  ( -86.69597344681494633, -1.750000000000009992, -159.1817124430720298 ) ) ;
#1437 = CARTESIAN_POINT ( 'NONE',  ( 155.0540265531850537, 1.025126265847089435, -157.4317124430720582 ) ) ;
#1438 = EDGE_CURVE ( 'NONE', #16652, #39156, #48204, .T. ) ;
#1439 = CARTESIAN_POINT ( 'NONE',  ( -44.94597344681493922, 2.143131898507880377E-16, -120.9317124430720725 ) ) ;
#1440 = VERTEX_POINT ( 'NONE', #28755 ) ;
#1441 = CARTESIAN_POINT ( 'NONE',  ( 2.052549611693792464, -0.2039603569406628347, 9.894754715216725671 ) ) ;
#1442 = CARTESIAN_POINT ( 'NONE',  ( 167.0000000000000000, 2.775557561562891351E-14, -111.0000000000001563 ) ) ;
#1443 = B_SPLINE_SURFACE_WITH_KNOTS ( 'NONE', 3, 3, ( 
 ( #32886, #21064, #17467, #8779 ),
 ( #20307, #48222, #39832, #16469 ),
 ( #36750, #28769, #20807, #1070 ),
 ( #1824, #13357, #1329, #21315 ) ),
 .UNSPECIFIED., .F., .F., .F.,
 ( 4, 4 ),
 ( 4, 4 ),
 ( 0.000000000000000000, 1.000000000000000000 ),
 ( 0.000000000000000000, 1.000000000000000000 ),
 .UNSPECIFIED. ) ;
#1444 = FACE_OUTER_BOUND ( 'NONE', #28602, .T. ) ;
#1445 = FACE_OUTER_BOUND ( 'NONE', #37012, .T. ) ;
#1446 = EDGE_CURVE ( 'NONE', #7572, #36969, #31859, .T. ) ;
#1447 = ADVANCED_FACE ( 'NONE', ( #43629 ), #8507, .F. ) ;
#1448 = EDGE_CURVE ( 'NONE', #3971, #2131, #35928, .T. ) ;
#1449 = LINE ( 'NONE', #40699, #40095 ) ;
#1450 = DIRECTION ( 'NONE',  ( 0.000000000000000000, 2.969158215481698263E-48, -1.000000000000000000 ) ) ;
#1451 = EDGE_CURVE ( 'NONE', #40407, #50112, #29507, .T. ) ;
#1452 = CARTESIAN_POINT ( 'NONE',  ( -165.6708471809677974, 1.750000000000009326, 161.8434138227750907 ) ) ;
#1453 = DIRECTION ( 'NONE',  ( -0.000000000000000000, -0.000000000000000000, -1.000000000000000000 ) ) ;
#1454 = EDGE_CURVE ( 'NONE', #19947, #30540, #41558, .T. ) ;
#1455 = EDGE_LOOP ( 'NONE', ( #11191, #5724, #8614, #8801, #38223, #46999 ) ) ;
#1456 = CARTESIAN_POINT ( 'NONE',  ( 20.20970188815904933, 31.63128376650817941, 3.209567239418972484 ) ) ;
#1457 = AXIS2_PLACEMENT_3D ( 'NONE', #19407, #34828, #31472 ) ;
#1458 = CYLINDRICAL_SURFACE ( 'NONE', #11513, 1.750000000000001554 ) ;
#1459 = ORIENTED_EDGE ( 'NONE', *, *, #28494, .T. ) ;
#1460 = DIRECTION ( 'NONE',  ( -0.000000000000000000, -0.000000000000000000, -1.000000000000000000 ) ) ;
#1461 = CARTESIAN_POINT ( 'NONE',  ( 5.505322767148756569, -37.09368438467003415, 8.914903342594564961 ) ) ;
#1462 = CARTESIAN_POINT ( 'NONE',  ( -3.893440188967678406, -0.6391102816410980658, 6.494306115488113207 ) ) ;
#1463 =( BOUNDED_CURVE ( )  B_SPLINE_CURVE ( 3, ( #9577, #49023, #10340, #2376 ),
 .UNSPECIFIED., .F., .F. ) 
 B_SPLINE_CURVE_WITH_KNOTS ( ( 4, 4 ),
 ( 3.141592653589793116, 4.712388980384689674 ),
 .UNSPECIFIED. ) 
 CURVE ( )  GEOMETRIC_REPRESENTATION_ITEM ( )  RATIONAL_B_SPLINE_CURVE ( ( 1.000000000000000000, 0.8047378541243649375, 0.8047378541243649375, 1.000000000000000000 ) ) 
 REPRESENTATION_ITEM ( '' )  );
#1464 = ORIENTED_EDGE ( 'NONE', *, *, #17426, .T. ) ;
#1465 = CARTESIAN_POINT ( 'NONE',  ( 0.000000000000000000, 0.000000000000000000, 900.0000000000000000 ) ) ;
#1466 = ORIENTED_EDGE ( 'NONE', *, *, #22101, .T. ) ;
#1467 = CARTESIAN_POINT ( 'NONE',  ( 4.641001526964560142, 33.28196331604080171, -8.016098858316199838 ) ) ;
#1468 = CARTESIAN_POINT ( 'NONE',  ( -166.6959734468149463, -1.750000000000010658, -79.18171244307201562 ) ) ;
#1469 = ORIENTED_EDGE ( 'NONE', *, *, #25027, .T. ) ;
#1470 = EDGE_CURVE ( 'NONE', #13625, #28349, #28185, .T. ) ;
#1471 = DIRECTION ( 'NONE',  ( -2.312964634635864737E-16, 0.000000000000000000, -1.000000000000000000 ) ) ;
#1472 = FACE_OUTER_BOUND ( 'NONE', #12433, .T. ) ;
#1473 = VERTEX_POINT ( 'NONE', #36989 ) ;
#1474 = VERTEX_POINT ( 'NONE', #49462 ) ;
#1475 = AXIS2_PLACEMENT_3D ( 'NONE', #39373, #4210, #35524 ) ;
#1476 = LINE ( 'NONE', #17109, #47212 ) ;
#1477 = ORIENTED_EDGE ( 'NONE', *, *, #34023, .T. ) ;
#1478 = FACE_OUTER_BOUND ( 'NONE', #18244, .T. ) ;
#1479 = CARTESIAN_POINT ( 'NONE',  ( 154.3291528190321458, 1.750000000000009326, 161.8434138227750907 ) ) ;
#1480 = FACE_OUTER_BOUND ( 'NONE', #35023, .T. ) ;
#1481 = VERTEX_POINT ( 'NONE', #33623 ) ;
#1482 = DIRECTION ( 'NONE',  ( -1.000000000000000000, -0.000000000000000000, -0.000000000000000000 ) ) ;
#1483 = ORIENTED_EDGE ( 'NONE', *, *, #9316, .F. ) ;
#1484 = ORIENTED_EDGE ( 'NONE', *, *, #39994, .T. ) ;
#1485 = ORIENTED_EDGE ( 'NONE', *, *, #21891, .T. ) ;
#1486 = CARTESIAN_POINT ( 'NONE',  ( -204.9459734468149463, 2.143131898507880377E-16, 122.5682875569279702 ) ) ;
#1487 = EDGE_CURVE ( 'NONE', #11190, #14077, #2552, .T. ) ;
#1488 = LINE ( 'NONE', #1981, #6990 ) ;
#1489 = EDGE_LOOP ( 'NONE', ( #35101, #41501, #18818, #26566 ) ) ;
#1490 = CARTESIAN_POINT ( 'NONE',  ( 181.0000000000000284, -174.9999999999999716, -95.00000000000014211 ) ) ;
#1491 = CARTESIAN_POINT ( 'NONE',  ( -0.1469336902871204442, -1.496274467947957376, 9.953784399990622589 ) ) ;
#1492 = LINE ( 'NONE', #20466, #38729 ) ;
#1493 = DIRECTION ( 'NONE',  ( 0.000000000000000000, 0.7071067811865475727, 0.7071067811865474617 ) ) ;
#1494 = DIRECTION ( 'NONE',  ( 0.000000000000000000, 0.000000000000000000, 1.000000000000000000 ) ) ;
#1495 = VECTOR ( 'NONE', #17389, 1000.000000000000000 ) ;
#1496 = DIRECTION ( 'NONE',  ( 0.000000000000000000, 0.000000000000000000, -1.000000000000000000 ) ) ;
#1497 = CARTESIAN_POINT ( 'NONE',  ( 22.69295089195473025, 45.31600496604705341, 7.455576670931136185 ) ) ;
#1498 = CARTESIAN_POINT ( 'NONE',  ( 31.55402655318503236, 1.025126265847089213, 42.56828755692799149 ) ) ;
#1499 = DIRECTION ( 'NONE',  ( -1.000000000000000000, -0.000000000000000000, -0.000000000000000000 ) ) ;
#1500 = CARTESIAN_POINT ( 'NONE',  ( -125.6708471809678542, -1.749999999999997113, 119.7931612910809065 ) ) ;
#1501 = CARTESIAN_POINT ( 'NONE',  ( -6.695973446814940111, 0.000000000000000000, 165.0000000000000000 ) ) ;
#1502 = EDGE_CURVE ( 'NONE', #35123, #48877, #11637, .T. ) ;
#1503 = EDGE_CURVE ( 'NONE', #46696, #38550, #18450, .T. ) ;
#1504 = CARTESIAN_POINT ( 'NONE',  ( -7.398363427652414614, 15.19415887381139108, -9.008049429158100807 ) ) ;
#1505 = ORIENTED_EDGE ( 'NONE', *, *, #34788, .T. ) ;
#1506 = DIRECTION ( 'NONE',  ( 0.000000000000000000, 0.000000000000000000, 1.000000000000000000 ) ) ;
#1507 = EDGE_CURVE ( 'NONE', #2019, #46289, #11808, .T. ) ;
#1508 = DIRECTION ( 'NONE',  ( 0.000000000000000000, -1.000000000000000000, 0.000000000000000000 ) ) ;
#1509 = CARTESIAN_POINT ( 'NONE',  ( -15.42815683172655028, -34.17926237904570996, 7.697694107796190899 ) ) ;
#1510 = CARTESIAN_POINT ( 'NONE',  ( -9.999999999999994671, -1.598124844265358068E-11, 9.303249460319950259 ) ) ;
#1511 = ADVANCED_FACE ( 'NONE', ( #37485 ), #21549, .F. ) ;
#1512 = EDGE_CURVE ( 'NONE', #49857, #7014, #14095, .T. ) ;
#1513 = ORIENTED_EDGE ( 'NONE', *, *, #38479, .T. ) ;
#1514 = LINE ( 'NONE', #36425, #23413 ) ;
#1515 = VERTEX_POINT ( 'NONE', #49713 ) ;
#1516 = CARTESIAN_POINT ( 'NONE',  ( 340.0000000000000000, 2.999999999999780176, -172.0000000000003126 ) ) ;
#1517 = CARTESIAN_POINT ( 'NONE',  ( 152.2789002873379900, 1.750000000000009548, -118.1565861772249519 ) ) ;
#1518 = LINE ( 'NONE', #31819, #42378 ) ;
#1519 = EDGE_CURVE ( 'NONE', #25904, #17310, #3074, .T. ) ;
#1520 = ORIENTED_EDGE ( 'NONE', *, *, #5204, .F. ) ;
#1521 = CARTESIAN_POINT ( 'NONE',  ( -208.4459734468148611, -1.025126265847089879, 122.5682875569280128 ) ) ;
#1522 = VERTEX_POINT ( 'NONE', #29757 ) ;
#1523 = ORIENTED_EDGE ( 'NONE', *, *, #41886, .T. ) ;
#1524 = VECTOR ( 'NONE', #37111, 1000.000000000000000 ) ;
#1525 = ORIENTED_EDGE ( 'NONE', *, *, #2062, .T. ) ;
#1526 = LINE ( 'NONE', #32071, #45024 ) ;
#1527 = CARTESIAN_POINT ( 'NONE',  ( -5.670847180967843570, -1.750000000000023981, -80.20683870891910772 ) ) ;
#1528 = VERTEX_POINT ( 'NONE', #48945 ) ;
#1529 = DIRECTION ( 'NONE',  ( 0.000000000000000000, 0.000000000000000000, -1.000000000000000000 ) ) ;
#1530 = CARTESIAN_POINT ( 'NONE',  ( -6.875132362119187768, 33.14667368551891258, 8.356839323120299312 ) ) ;
#1531 = LINE ( 'NONE', #48673, #24115 ) ;
#1532 = B_SPLINE_CURVE_WITH_KNOTS ( 'NONE', 3,
 ( #37436, #16713, #17656, #33324 ),
 .UNSPECIFIED., .F., .F.,
 ( 4, 4 ),
 ( 1.202632570208740988E-15, 0.0002520763768916307011 ),
 .UNSPECIFIED. ) ;
#1533 = CARTESIAN_POINT ( 'NONE',  ( -166.6959734468149463, -1.750000000000009992, 0.8182875569279768335 ) ) ;
#1534 = CLOSED_SHELL ( 'NONE', ( #35763, #10524, #38050, #13677, #45020, #8977, #29636, #25368 ) ) ;
#1535 = ORIENTED_EDGE ( 'NONE', *, *, #37841, .F. ) ;
#1536 = CARTESIAN_POINT ( 'NONE',  ( -210.0000000000000568, 0.000000000000000000, -79.18171244307201562 ) ) ;
#1537 = ORIENTED_EDGE ( 'NONE', *, *, #15885, .T. ) ;
#1538 = LINE ( 'NONE', #40533, #35833 ) ;
#1539 = LINE ( 'NONE', #14076, #755 ) ;
#1540 = ORIENTED_EDGE ( 'NONE', *, *, #24099, .F. ) ;
#1541 = ORIENTED_EDGE ( 'NONE', *, *, #27872, .T. ) ;
#1542 = ORIENTED_EDGE ( 'NONE', *, *, #23285, .F. ) ;
#1543 = CARTESIAN_POINT ( 'NONE',  ( -1.104609456715841986, -0.6504863887005195577, 9.948547179989617462 ) ) ;
#1544 = CARTESIAN_POINT ( 'NONE',  ( 168.9999999999999716, -77.49999999999997158, -350.0000000000001705 ) ) ;
#1545 = PRODUCT ( 'tire assembly', 'tire assembly', '', ( #8761 ) ) ;
#1546 = ORIENTED_EDGE ( 'NONE', *, *, #35417, .T. ) ;
#1547 = EDGE_CURVE ( 'NONE', #25771, #44889, #44722, .T. ) ;
#1548 = CARTESIAN_POINT ( 'NONE',  ( -128.4459734468149179, 0.000000000000000000, 119.0682875569279986 ) ) ;
#1549 = CARTESIAN_POINT ( 'NONE',  ( 135.0000000000006253, 17.00000000000000000, -54.99999999999999289 ) ) ;
#1550 = CARTESIAN_POINT ( 'NONE',  ( 193.3040265531851105, 0.000000000000000000, 165.0000000000000000 ) ) ;
#1551 = VERTEX_POINT ( 'NONE', #25409 ) ;
#1552 = CARTESIAN_POINT ( 'NONE',  ( 185.0000000000000568, 175.0000000000000284, 343.9999999999998863 ) ) ;
#1553 = DIRECTION ( 'NONE',  ( -0.000000000000000000, -0.000000000000000000, -1.000000000000000000 ) ) ;
#1554 = LINE ( 'NONE', #40548, #3495 ) ;
#1555 = ORIENTED_EDGE ( 'NONE', *, *, #40015, .F. ) ;
#1556 = ORIENTED_EDGE ( 'NONE', *, *, #33956, .F. ) ;
#1557 = VECTOR ( 'NONE', #22431, 1000.000000000000000 ) ;
#1558 = CARTESIAN_POINT ( 'NONE',  ( 113.3040265531850537, -1.749999999999997335, 120.8182875569279702 ) ) ;
#1559 = FACE_BOUND ( 'NONE', #31740, .T. ) ;
#1560 = VECTOR ( 'NONE', #24107, 1000.000000000000000 ) ;
#1561 = ADVANCED_FACE ( 'NONE', ( #6652 ), #17704, .T. ) ;
#1562 = CARTESIAN_POINT ( 'NONE',  ( 1.305887768059120768, -0.05395936524050352207, 9.945465957785110334 ) ) ;
#1563 = CARTESIAN_POINT ( 'NONE',  ( 166.9999999999999716, -81.49999999999988631, -115.0000000000001563 ) ) ;
#1564 = ORIENTED_EDGE ( 'NONE', *, *, #42492, .F. ) ;
#1565 = VECTOR ( 'NONE', #13665, 1000.000000000000000 ) ;
#1566 = CARTESIAN_POINT ( 'NONE',  ( 195.0540265531851105, 2.143131898507880377E-16, 42.56828755692798438 ) ) ;
#1567 = CARTESIAN_POINT ( 'NONE',  ( -31.28234235046239320, -11.28615439405757392, -3.760136334089591248 ) ) ;
#1568 = DIRECTION ( 'NONE',  ( 1.000000000000000000, 8.673617379884028076E-17, -0.000000000000000000 ) ) ;
#1569 = VECTOR ( 'NONE', #37477, 1000.000000000000000 ) ;
#1570 = LINE ( 'NONE', #25167, #3304 ) ;
#1571 = EDGE_CURVE ( 'NONE', #23819, #8288, #25666, .T. ) ;
#1572 = EDGE_CURVE ( 'NONE', #24608, #2518, #38179, .T. ) ;
#1573 = AXIS2_PLACEMENT_3D ( 'NONE', #18165, #48670, #2769 ) ;
#1574 = ORIENTED_EDGE ( 'NONE', *, *, #47710, .F. ) ;
#1575 = CARTESIAN_POINT ( 'NONE',  ( 0.000000000000000000, 184.8000000000000114, -340.2000000000001592 ) ) ;
#1576 = ORIENTED_EDGE ( 'NONE', *, *, #48562, .F. ) ;
#1577 = CARTESIAN_POINT ( 'NONE',  ( 6.204997580903516941, 7.611558401714507482, 225.0000000000000000 ) ) ;
#1578 = ORIENTED_EDGE ( 'NONE', *, *, #38465, .F. ) ;
#1579 = ADVANCED_FACE ( 'NONE', ( #42810 ), #39243, .T. ) ;
#1580 = LINE ( 'NONE', #41075, #49952 ) ;
#1581 = DIRECTION ( 'NONE',  ( -0.000000000000000000, -0.000000000000000000, -1.000000000000000000 ) ) ;
#1582 = CARTESIAN_POINT ( 'NONE',  ( 34.32915281903212446, 1.750000000000010214, 79.79316129108087807 ) ) ;
#1583 = ORIENTED_EDGE ( 'NONE', *, *, #30240, .F. ) ;
#1584 = CARTESIAN_POINT ( 'NONE',  ( -8.445973446814976526, 0.000000000000000000, -77.43171244307198720 ) ) ;
#1585 = ORIENTED_EDGE ( 'NONE', *, *, #10780, .F. ) ;
#1586 = CYLINDRICAL_SURFACE ( 'NONE', #35227, 1.750000000000015543 ) ;
#1587 = CARTESIAN_POINT ( 'NONE',  ( -9.970345420962654970, 0.8985218257325405800, 2.778652340039163171 ) ) ;
#1588 = FACE_OUTER_BOUND ( 'NONE', #19756, .T. ) ;
#1589 = CARTESIAN_POINT ( 'NONE',  ( -5.000000000000000000, 175.0000000000000284, -350.0000000000002274 ) ) ;
#1590 = DIRECTION ( 'NONE',  ( -1.000000000000000000, -0.000000000000000000, -0.000000000000000000 ) ) ;
#1591 = EDGE_LOOP ( 'NONE', ( #7982, #46133, #48902, #23547, #10690, #1872 ) ) ;
#1592 = ORIENTED_EDGE ( 'NONE', *, *, #5961, .F. ) ;
#1593 = CARTESIAN_POINT ( 'NONE',  ( 135.0000000000015632, 17.00000000000000000, 35.00000000000000000 ) ) ;
#1594 =( BOUNDED_CURVE ( )  B_SPLINE_CURVE ( 3, ( #48627, #41480, #48878, #13516 ),
 .UNSPECIFIED., .F., .F. ) 
 B_SPLINE_CURVE_WITH_KNOTS ( ( 4, 4 ),
 ( 3.141592653589793116, 4.712388980384689674 ),
 .UNSPECIFIED. ) 
 CURVE ( )  GEOMETRIC_REPRESENTATION_ITEM ( )  RATIONAL_B_SPLINE_CURVE ( ( 1.000000000000000000, 0.8047378541243649375, 0.8047378541243649375, 1.000000000000000000 ) ) 
 REPRESENTATION_ITEM ( '' )  );
#1595 = AXIS2_PLACEMENT_3D ( 'NONE', #29390, #45260, #29643 ) ;
#1596 = ORIENTED_EDGE ( 'NONE', *, *, #17680, .T. ) ;
#1597 = CARTESIAN_POINT ( 'NONE',  ( -164.9999999999997442, 17.00000000000000000, -84.99999999999998579 ) ) ;
#1598 = CARTESIAN_POINT ( 'NONE',  ( -194.9999999999999432, 173.0000000000000000, 252.0000000000000000 ) ) ;
#1599 = ORIENTED_EDGE ( 'NONE', *, *, #39802, .T. ) ;
#1600 = DIRECTION ( 'NONE',  ( 0.000000000000000000, 0.000000000000000000, -1.000000000000000000 ) ) ;
#1601 = VECTOR ( 'NONE', #37906, 1000.000000000000000 ) ;
#1602 = VECTOR ( 'NONE', #41002, 1000.000000000000000 ) ;
#1603 =( BOUNDED_CURVE ( )  B_SPLINE_CURVE ( 3, ( #5591, #14040, #45324, #13543 ),
 .UNSPECIFIED., .F., .F. ) 
 B_SPLINE_CURVE_WITH_KNOTS ( ( 4, 4 ),
 ( 4.712388980384689674, 6.283185307179586232 ),
 .UNSPECIFIED. ) 
 CURVE ( )  GEOMETRIC_REPRESENTATION_ITEM ( )  RATIONAL_B_SPLINE_CURVE ( ( 1.000000000000000000, 0.8047378541243649375, 0.8047378541243649375, 1.000000000000000000 ) ) 
 REPRESENTATION_ITEM ( '' )  );
#1604 = DIRECTION ( 'NONE',  ( 0.000000000000000000, 0.000000000000000000, 1.000000000000000000 ) ) ;
#1605 = VERTEX_POINT ( 'NONE', #42557 ) ;
#1606 = CARTESIAN_POINT ( 'NONE',  ( 168.9999999999999716, -256.4999999999999432, -349.9999999999999432 ) ) ;
#1607 = EDGE_CURVE ( 'NONE', #31600, #29622, #248, .T. ) ;
#1608 = CARTESIAN_POINT ( 'NONE',  ( 214.9999999999999432, -173.0000000000000000, 352.0000000000001137 ) ) ;
#1609 = CARTESIAN_POINT ( 'NONE',  ( 183.0000000000000284, 2.775557561562891351E-14, -111.0000000000001563 ) ) ;
#1610 = AXIS2_PLACEMENT_3D ( 'NONE', #47849, #48853, #16594 ) ;
#1611 = CYLINDRICAL_SURFACE ( 'NONE', #46841, 1.750000000000015543 ) ;
#1612 = ORIENTED_EDGE ( 'NONE', *, *, #40096, .F. ) ;
#1613 = ORIENTED_EDGE ( 'NONE', *, *, #42830, .T. ) ;
#1614 = ORIENTED_EDGE ( 'NONE', *, *, #14576, .T. ) ;
#1615 = CYLINDRICAL_SURFACE ( 'NONE', #5829, 4.000000000000003553 ) ;
#1616 = DIRECTION ( 'NONE',  ( 0.000000000000000000, 0.000000000000000000, 1.000000000000000000 ) ) ;
#1617 = CARTESIAN_POINT ( 'NONE',  ( 129.9999999999999432, 17.00000000000000000, -114.9999999999999858 ) ) ;
#1618 =( BOUNDED_CURVE ( )  B_SPLINE_CURVE ( 3, ( #30631, #42408, #38595, #3414 ),
 .UNSPECIFIED., .F., .F. ) 
 B_SPLINE_CURVE_WITH_KNOTS ( ( 4, 4 ),
 ( 3.141592653589793116, 4.712388980384689674 ),
 .UNSPECIFIED. ) 
 CURVE ( )  GEOMETRIC_REPRESENTATION_ITEM ( )  RATIONAL_B_SPLINE_CURVE ( ( 1.000000000000000000, 0.8047378541243649375, 0.8047378541243649375, 1.000000000000000000 ) ) 
 REPRESENTATION_ITEM ( '' )  );
#1619 = DIRECTION ( 'NONE',  ( 0.000000000000000000, -0.3846153846153845812, -0.9230769230769231282 ) ) ;
#1620 = ORIENTED_EDGE ( 'NONE', *, *, #34416, .F. ) ;
#1621 = PLANE ( 'NONE',  #37359 ) ;
#1622 = ORIENTED_EDGE ( 'NONE', *, *, #18111, .T. ) ;
#1623 = DIRECTION ( 'NONE',  ( 0.9999999999999998890, 0.000000000000000000, 0.000000000000000000 ) ) ;
#1624 = CARTESIAN_POINT ( 'NONE',  ( 9.281355226777661116, -3.722424633806168615, 0.000000000000000000 ) ) ;
#1625 = DIRECTION ( 'NONE',  ( 0.000000000000000000, 0.000000000000000000, 1.000000000000000000 ) ) ;
#1626 = DIRECTION ( 'NONE',  ( 1.000000000000000000, 0.000000000000000000, 0.000000000000000000 ) ) ;
#1627 = CARTESIAN_POINT ( 'NONE',  ( 210.0000000000000568, 0.000000000000000000, -77.43171244307200141 ) ) ;
#1628 = LINE ( 'NONE', #17272, #16605 ) ;
#1629 = ORIENTED_EDGE ( 'NONE', *, *, #19967, .T. ) ;
#1630 = CARTESIAN_POINT ( 'NONE',  ( 1.250000000000000222, 0.000000000000000000, 10.00000000000000000 ) ) ;
#1631 = CARTESIAN_POINT ( 'NONE',  ( -44.94597344681493922, 2.143131898507880377E-16, 165.0000000000000000 ) ) ;
#1632 = DIRECTION ( 'NONE',  ( -0.000000000000000000, -0.000000000000000000, -1.000000000000000000 ) ) ;
#1633 = CIRCLE ( 'NONE', #43400, 22.00000000000000000 ) ;
#1634 = VECTOR ( 'NONE', #50677, 1000.000000000000000 ) ;
#1635 = VECTOR ( 'NONE', #46203, 1000.000000000000000 ) ;
#1636 = CARTESIAN_POINT ( 'NONE',  ( -46.69597344681494633, 0.000000000000000000, 165.0000000000000000 ) ) ;
#1637 = ORIENTED_EDGE ( 'NONE', *, *, #40941, .F. ) ;
#1638 = PLANE ( 'NONE',  #22895 ) ;
#1639 = VERTEX_POINT ( 'NONE', #35403 ) ;
#1640 = ADVANCED_FACE ( 'NONE', ( #18697 ), #19729, .F. ) ;
#1641 = AXIS2_PLACEMENT_3D ( 'NONE', #31335, #27725, #27222 ) ;
#1642 = CARTESIAN_POINT ( 'NONE',  ( 2.500000000000000444, 224.9999999999999716, -240.0000000000000000 ) ) ;
#1643 = DIRECTION ( 'NONE',  ( -1.000000000000000000, 0.000000000000000000, 0.000000000000000000 ) ) ;
#1644 = CARTESIAN_POINT ( 'NONE',  ( 181.0000000000000284, -9.999999999999953815, -97.00000000000014211 ) ) ;
#1645 = ORIENTED_EDGE ( 'NONE', *, *, #40228, .T. ) ;
#1646 = CIRCLE ( 'NONE', #12289, 0.4999999999999997224 ) ;
#1647 = DIRECTION ( 'NONE',  ( -0.000000000000000000, -0.000000000000000000, 1.000000000000000000 ) ) ;
#1648 = CARTESIAN_POINT ( 'NONE',  ( 20.37409433807990666, 26.28007012093483397, -2.408242355805840784 ) ) ;
#1649 = CARTESIAN_POINT ( 'NONE',  ( -16.15814872688569181, -4.048305257546697788, -2.870787844569587133 ) ) ;
#1650 = DIRECTION ( 'NONE',  ( 0.000000000000000000, 0.000000000000000000, 1.000000000000000000 ) ) ;
#1651 = ORIENTED_EDGE ( 'NONE', *, *, #23469, .T. ) ;
#1652 = ORIENTED_EDGE ( 'NONE', *, *, #46034, .F. ) ;
#1653 = CARTESIAN_POINT ( 'NONE',  ( 135.0000000000009663, 17.00000000000000000, -24.99999999999999289 ) ) ;
#1654 = CARTESIAN_POINT ( 'NONE',  ( -18.38319608353667434, 32.68498281710182596, -8.192531242611268638 ) ) ;
#1655 = ORIENTED_EDGE ( 'NONE', *, *, #46232, .F. ) ;
#1656 = ORIENTED_EDGE ( 'NONE', *, *, #833, .F. ) ;
#1657 = CARTESIAN_POINT ( 'NONE',  ( -86.69597344681496054, 0.000000000000000000, 165.0000000000000000 ) ) ;
#1658 = CARTESIAN_POINT ( 'NONE',  ( -64.99999999999815259, 16.00000000000000000, 90.00000000000000000 ) ) ;
#1659 = DIRECTION ( 'NONE',  ( 0.000000000000000000, 2.537652627714642000E-15, 1.000000000000000000 ) ) ;
#1660 = CARTESIAN_POINT ( 'NONE',  ( -1.552956552085981379, -0.2464513101957222507, 9.945241992664930919 ) ) ;
#1661 = ORIENTED_EDGE ( 'NONE', *, *, #43378, .T. ) ;
#1662 = VERTEX_POINT ( 'NONE', #15882 ) ;
#1663 = VERTEX_POINT ( 'NONE', #31551 ) ;
#1664 = EDGE_CURVE ( 'NONE', #10051, #46359, #30516, .T. ) ;
#1665 = B_SPLINE_CURVE_WITH_KNOTS ( 'NONE', 3,
 ( #1927, #30132, #5767, #29372 ),
 .UNSPECIFIED., .F., .F.,
 ( 4, 4 ),
 ( 1.788112030672749005E-18, 0.009404691289023351872 ),
 .UNSPECIFIED. ) ;
#1666 = VECTOR ( 'NONE', #34213, 1000.000000000000000 ) ;
#1667 = EDGE_CURVE ( 'NONE', #10095, #32209, #7435, .T. ) ;
#1668 = CARTESIAN_POINT ( 'NONE',  ( 169.0000000000000000, -174.9999999999999716, -115.0000000000001563 ) ) ;
#1669 = VECTOR ( 'NONE', #37747, 1000.000000000000000 ) ;
#1670 = ORIENTED_EDGE ( 'NONE', *, *, #18646, .F. ) ;
#1671 = ORIENTED_EDGE ( 'NONE', *, *, #6376, .T. ) ;
#1672 = CARTESIAN_POINT ( 'NONE',  ( 35.05402655318504657, -1.025126265847089213, -0.9317124430720324924 ) ) ;
#1673 = AXIS2_PLACEMENT_3D ( 'NONE', #47188, #4871, #27484 ) ;
#1674 = CARTESIAN_POINT ( 'NONE',  ( 210.0000000000000568, 0.000000000000000000, 42.56828755692799149 ) ) ;
#1675 = ORIENTED_EDGE ( 'NONE', *, *, #11798, .F. ) ;
#1676 = VERTEX_POINT ( 'NONE', #42057 ) ;
#1677 = LINE ( 'NONE', #29126, #7788 ) ;
#1678 = CARTESIAN_POINT ( 'NONE',  ( -128.4459734468149179, 0.000000000000000000, 82.56828755692795596 ) ) ;
#1679 = ORIENTED_EDGE ( 'NONE', *, *, #13074, .F. ) ;
#1680 = CARTESIAN_POINT ( 'NONE',  ( 185.0000000000000000, -93.49999999999997158, -115.0000000000001563 ) ) ;
#1681 = DIRECTION ( 'NONE',  ( -1.000000000000000000, 0.000000000000000000, 0.000000000000000000 ) ) ;
#1682 = CARTESIAN_POINT ( 'NONE',  ( -206.6959734468149463, 1.750000000000010214, 40.81828755692798438 ) ) ;
#1683 = CARTESIAN_POINT ( 'NONE',  ( -20.00000000000003197, 17.00000000000000000, -90.00000000000000000 ) ) ;
#1684 = CARTESIAN_POINT ( 'NONE',  ( 152.2789002873379900, -1.750000000000009548, 1.843413822775065825 ) ) ;
#1685 = ORIENTED_EDGE ( 'NONE', *, *, #39068, .F. ) ;
#1686 = DIRECTION ( 'NONE',  ( -1.000000000000000000, -0.000000000000000000, -0.000000000000000000 ) ) ;
#1687 = FACE_OUTER_BOUND ( 'NONE', #16486, .T. ) ;
#1688 = CARTESIAN_POINT ( 'NONE',  ( 341.9999999999999432, -169.0000000000001137, -344.0000000000002842 ) ) ;
#1689 = CARTESIAN_POINT ( 'NONE',  ( 20.21530556545302559, -31.58467066308217497, -9.422646554964174470 ) ) ;
#1690 = EDGE_CURVE ( 'NONE', #32484, #24437, #16703, .T. ) ;
#1691 = ADVANCED_FACE ( 'NONE', ( #22813 ), #15118, .F. ) ;
#1692 = LINE ( 'NONE', #37373, #33868 ) ;
#1693 = CARTESIAN_POINT ( 'NONE',  ( 151.5540265531850537, 0.000000000000000000, 82.56828755692798438 ) ) ;
#1694 = EDGE_CURVE ( 'NONE', #25157, #35762, #23369, .T. ) ;
#1695 = CYLINDRICAL_SURFACE ( 'NONE', #26203, 1.750000000000001554 ) ;
#1696 = CARTESIAN_POINT ( 'NONE',  ( 17.67745476136639482, 37.99701471135983155, 7.544061037322996377 ) ) ;
#1697 = ADVANCED_FACE ( 'NONE', ( #38733 ), #46388, .F. ) ;
#1698 = AXIS2_PLACEMENT_3D ( 'NONE', #6620, #22275, #38696 ) ;
#1699 = EDGE_LOOP ( 'NONE', ( #15444, #5119, #18178, #21063, #5514, #12297 ) ) ;
#1700 = EDGE_CURVE ( 'NONE', #4161, #27522, #26915, .T. ) ;
#1701 = DIRECTION ( 'NONE',  ( -0.000000000000000000, -1.000000000000000000, -0.000000000000000000 ) ) ;
#1702 = CIRCLE ( 'NONE', #49186, 2.000000000000001776 ) ;
#1703 = CARTESIAN_POINT ( 'NONE',  ( -15.44803555374685189, -6.237487519713257100, -3.546734833711462365 ) ) ;
#1704 = CYLINDRICAL_SURFACE ( 'NONE', #1610, 1.750000000000008438 ) ;
#1705 = CARTESIAN_POINT ( 'NONE',  ( 6.174150299305392053, -50.00000000000000000, 8.807470649214879543 ) ) ;
#1706 = CARTESIAN_POINT ( 'NONE',  ( 31.55402655318503236, 1.025126265847089435, 39.06828755692797728 ) ) ;
#1707 = AXIS2_PLACEMENT_3D ( 'NONE', #46684, #11062, #3101 ) ;
#1708 = ORIENTED_EDGE ( 'NONE', *, *, #46797, .T. ) ;
#1709 = DIRECTION ( 'NONE',  ( 0.000000000000000000, 6.938893903907221278E-15, -1.000000000000000000 ) ) ;
#1710 = VECTOR ( 'NONE', #40010, 1000.000000000000000 ) ;
#1711 = ORIENTED_EDGE ( 'NONE', *, *, #30976, .F. ) ;
#1712 = DIRECTION ( 'NONE',  ( -1.000000000000000000, -0.000000000000000000, 0.000000000000000000 ) ) ;
#1713 = CARTESIAN_POINT ( 'NONE',  ( -166.6959734468149463, -1.750000000000010658, 120.8182875569279702 ) ) ;
#1714 = ORIENTED_EDGE ( 'NONE', *, *, #45469, .F. ) ;
#1715 = CYLINDRICAL_SURFACE ( 'NONE', #30337, 1.750000000000001554 ) ;
#1716 = CARTESIAN_POINT ( 'NONE',  ( 370.7621192902014968, 70.03596893647589638, -93.79675437945476801 ) ) ;
#1717 = VERTEX_POINT ( 'NONE', #3556 ) ;
#1718 = ORIENTED_EDGE ( 'NONE', *, *, #38682, .T. ) ;
#1719 = EDGE_CURVE ( 'NONE', #25392, #44652, #50206, .T. ) ;
#1720 = EDGE_CURVE ( 'NONE', #12850, #13383, #4738, .T. ) ;
#1721 = CARTESIAN_POINT ( 'NONE',  ( -0.6812154050773484570, -2.552002810692194590, 9.847478953136988622 ) ) ;
#1722 = FACE_OUTER_BOUND ( 'NONE', #20432, .T. ) ;
#1723 = DIRECTION ( 'NONE',  ( -1.542934785277626909E-15, 0.9749645535258950613, 0.2223603367690656918 ) ) ;
#1724 = ADVANCED_FACE ( 'NONE', ( #23579 ), #22557, .T. ) ;
#1725 = ORIENTED_EDGE ( 'NONE', *, *, #46852, .T. ) ;
#1726 = EDGE_CURVE ( 'NONE', #13717, #19110, #49961, .T. ) ;
#1727 = CARTESIAN_POINT ( 'NONE',  ( 115.0540265531850395, 2.143131898507847836E-16, 79.06828755692798438 ) ) ;
#1728 = DIRECTION ( 'NONE',  ( 0.000000000000000000, 0.000000000000000000, 1.000000000000000000 ) ) ;
#1729 = ORIENTED_EDGE ( 'NONE', *, *, #43705, .F. ) ;
#1730 = ORIENTED_EDGE ( 'NONE', *, *, #33079, .T. ) ;
#1731 = ORIENTED_EDGE ( 'NONE', *, *, #10149, .F. ) ;
#1732 = CARTESIAN_POINT ( 'NONE',  ( 1.769963848780946369, -9.842115015280432644, 0.000000000000000000 ) ) ;
#1733 = EDGE_CURVE ( 'NONE', #27742, #2419, #8705, .T. ) ;
#1734 = EDGE_CURVE ( 'NONE', #3452, #11387, #40498, .T. ) ;
#1735 = DIRECTION ( 'NONE',  ( -1.000000000000000000, -0.000000000000000000, -0.000000000000000000 ) ) ;
#1736 = ORIENTED_EDGE ( 'NONE', *, *, #9293, .T. ) ;
#1737 = CIRCLE ( 'NONE', #6632, 10.00000000000000000 ) ;
#1738 = CARTESIAN_POINT ( 'NONE',  ( -88.44597344681494633, -1.025126265847089657, -120.9317124430720440 ) ) ;
#1739 = LINE ( 'NONE', #41487, #7585 ) ;
#1740 = PLANE ( 'NONE',  #4006 ) ;
#1741 = CARTESIAN_POINT ( 'NONE',  ( -205.6708471809678827, -1.750000000000010436, -120.2068387089191219 ) ) ;
#1742 = LINE ( 'NONE', #9179, #8730 ) ;
#1743 = VECTOR ( 'NONE', #7024, 1000.000000000000000 ) ;
#1744 = DIRECTION ( 'NONE',  ( 0.000000000000000000, 0.000000000000000000, 1.000000000000000000 ) ) ;
#1745 = CYLINDRICAL_SURFACE ( 'NONE', #44480, 1.750000000000015543 ) ;
#1746 = CARTESIAN_POINT ( 'NONE',  ( 33.08717642956892746, 5.870837526465160217, -8.016098858316199838 ) ) ;
#1747 = EDGE_CURVE ( 'NONE', #14468, #4061, #20996, .T. ) ;
#1748 = FACE_OUTER_BOUND ( 'NONE', #29837, .T. ) ;
#1749 = EDGE_CURVE ( 'NONE', #8266, #33773, #42921, .T. ) ;
#1750 = ADVANCED_FACE ( 'NONE', ( #36154 ), #24355, .T. ) ;
#1751 = CARTESIAN_POINT ( 'NONE',  ( 85.00000000000123634, 17.00000000000000000, 30.00000000000000000 ) ) ;
#1752 = ORIENTED_EDGE ( 'NONE', *, *, #22020, .F. ) ;
#1753 = LINE ( 'NONE', #10453, #28621 ) ;
#1754 =( BOUNDED_CURVE ( )  B_SPLINE_CURVE ( 3, ( #9067, #31680, #620, #16014 ),
 .UNSPECIFIED., .F., .F. ) 
 B_SPLINE_CURVE_WITH_KNOTS ( ( 4, 4 ),
 ( 3.141592653589793116, 4.712388980384689674 ),
 .UNSPECIFIED. ) 
 CURVE ( )  GEOMETRIC_REPRESENTATION_ITEM ( )  RATIONAL_B_SPLINE_CURVE ( ( 1.000000000000000000, 0.8047378541243649375, 0.8047378541243649375, 1.000000000000000000 ) ) 
 REPRESENTATION_ITEM ( '' )  );
#1755 = CARTESIAN_POINT ( 'NONE',  ( -40.00000000000000000, 7.564790863224932771, 897.6604670114604687 ) ) ;
#1756 = LINE ( 'NONE', #16389, #30760 ) ;
#1757 = CARTESIAN_POINT ( 'NONE',  ( 168.9999999999999716, -5.999999999999950262, 339.9999999999998295 ) ) ;
#1758 = ORIENTED_EDGE ( 'NONE', *, *, #29451, .T. ) ;
#1759 = CARTESIAN_POINT ( 'NONE',  ( 135.0000000000009663, 16.00000000000000000, -24.99999999999999289 ) ) ;
#1760 = DIRECTION ( 'NONE',  ( 0.000000000000000000, -1.000000000000000000, 0.000000000000000000 ) ) ;
#1761 = ORIENTED_EDGE ( 'NONE', *, *, #13263, .F. ) ;
#1762 = CARTESIAN_POINT ( 'NONE',  ( -12.16428377685542195, -11.73151505502925929, -9.008049429158102583 ) ) ;
#1764 = EDGE_CURVE ( 'NONE', #43746, #42197, #37215, .T. ) ;
#1763 = DIRECTION ( 'NONE',  ( -1.000000000000000000, 0.000000000000000000, 0.000000000000000000 ) ) ;
#1765 = CARTESIAN_POINT ( 'NONE',  ( -45.67084718096785423, -1.750000000000009548, -40.20683870891912193 ) ) ;
#1766 = AXIS2_PLACEMENT_3D ( 'NONE', #6164, #29765, #40809 ) ;
#1767 = ORIENTED_EDGE ( 'NONE', *, *, #19317, .F. ) ;
#1768 = DIRECTION ( 'NONE',  ( 0.000000000000000000, 0.000000000000000000, 1.000000000000000000 ) ) ;
#1769 = ORIENTED_EDGE ( 'NONE', *, *, #14706, .T. ) ;
#1770 = EDGE_LOOP ( 'NONE', ( #6940, #12949, #39459, #6702 ) ) ;
#1771 = DIRECTION ( 'NONE',  ( 0.000000000000000000, 1.000000000000000000, 0.000000000000000000 ) ) ;
#1772 = ORIENTED_EDGE ( 'NONE', *, *, #25237, .T. ) ;
#1773 = DIRECTION ( 'NONE',  ( 0.000000000000000000, 0.000000000000000000, 1.000000000000000000 ) ) ;
#1774 = CARTESIAN_POINT ( 'NONE',  ( -12.78770032058971395, -31.68259716188267916, 7.455576670931136185 ) ) ;
#1775 = EDGE_CURVE ( 'NONE', #28153, #21400, #32556, .T. ) ;
#1776 = ORIENTED_EDGE ( 'NONE', *, *, #3846, .F. ) ;
#1777 = CARTESIAN_POINT ( 'NONE',  ( 44.99506233596247995, 23.32283626942318833, 7.455576670931136185 ) ) ;
#1778 = CARTESIAN_POINT ( 'NONE',  ( 29.99999999999998579, 17.00000000000000000, -114.9999999999999858 ) ) ;
#1779 = DIRECTION ( 'NONE',  ( -0.000000000000000000, -1.000000000000000000, -0.000000000000000000 ) ) ;
#1780 = AXIS2_PLACEMENT_3D ( 'NONE', #25486, #49289, #14172 ) ;
#1781 = DIRECTION ( 'NONE',  ( 1.000000000000000000, 0.000000000000000000, 0.000000000000000000 ) ) ;
#1782 = ORIENTED_EDGE ( 'NONE', *, *, #10448, .T. ) ;
#1783 = LINE ( 'NONE', #33099, #13291 ) ;
#1784 = ADVANCED_FACE ( 'NONE', ( #43576 ), #5072, .T. ) ;
#1785 = ORIENTED_EDGE ( 'NONE', *, *, #33974, .F. ) ;
#1786 = ADVANCED_FACE ( 'NONE', ( #24847 ), #20480, .T. ) ;
#1787 = DIRECTION ( 'NONE',  ( 0.000000000000000000, 0.000000000000000000, 1.000000000000000000 ) ) ;
#1788 = ORIENTED_EDGE ( 'NONE', *, *, #23940, .F. ) ;
#1789 = ORIENTED_EDGE ( 'NONE', *, *, #37137, .F. ) ;
#1790 = VERTEX_POINT ( 'NONE', #17144 ) ;
#1791 = DIRECTION ( 'NONE',  ( 0.000000000000000000, 1.000000000000000000, 3.186989995019654210E-49 ) ) ;
#1792 = EDGE_CURVE ( 'NONE', #35881, #24944, #10954, .T. ) ;
#1793 = CARTESIAN_POINT ( 'NONE',  ( -46.69597344681494633, 1.750000000000010214, 40.81828755692798438 ) ) ;
#1794 = ORIENTED_EDGE ( 'NONE', *, *, #9385, .F. ) ;
#1795 = ADVANCED_FACE ( 'NONE', ( #994, #12278 ), #500, .F. ) ;
#1796 = CARTESIAN_POINT ( 'NONE',  ( 168.9999999999999716, -180.9999999999999716, -340.0000000000001137 ) ) ;
#1797 = CARTESIAN_POINT ( 'NONE',  ( 1.250000000000000222, 0.000000000000000000, -3.333333333333333481 ) ) ;
#1798 = ADVANCED_FACE ( 'NONE', ( #32050 ), #48395, .T. ) ;
#1799 = DIRECTION ( 'NONE',  ( 4.759647537211363479E-16, -5.772796816983493182E-42, 1.000000000000000000 ) ) ;
#1800 = ORIENTED_EDGE ( 'NONE', *, *, #24123, .F. ) ;
#1801 = CARTESIAN_POINT ( 'NONE',  ( -6.695973446814940111, -1.750000000000024203, -79.18171244307201562 ) ) ;
#1802 = CARTESIAN_POINT ( 'NONE',  ( 36.28567981536807707, 9.465698090293649614, -9.422646554964174470 ) ) ;
#1803 = VECTOR ( 'NONE', #28805, 1000.000000000000000 ) ;
#1804 = EDGE_CURVE ( 'NONE', #31856, #4890, #4338, .T. ) ;
#1805 = CARTESIAN_POINT ( 'NONE',  ( -46.10908423965022251, -19.89422939639105437, 1.847720168420772691 ) ) ;
#1806 = ORIENTED_EDGE ( 'NONE', *, *, #46982, .T. ) ;
#1807 = B_SPLINE_CURVE_WITH_KNOTS ( 'NONE', 3,
 ( #29286, #12875, #24690, #17482 ),
 .UNSPECIFIED., .F., .F.,
 ( 4, 4 ),
 ( 3.469446951953614189E-18, 8.326314924666544353E-06 ),
 .UNSPECIFIED. ) ;
#1808 = ORIENTED_EDGE ( 'NONE', *, *, #7338, .T. ) ;
#1809 = PRODUCT_CONTEXT ( 'NONE', #435, 'mechanical' ) ;
#1810 = CARTESIAN_POINT ( 'NONE',  ( 210.0000000000000568, 0.000000000000000000, -39.18171244307202983 ) ) ;
#1811 = CARTESIAN_POINT ( 'NONE',  ( 350.0000000000000000, -180.9999999999999716, -342.0000000000001705 ) ) ;
#1812 = AXIS2_PLACEMENT_3D ( 'NONE', #17777, #25735, #6236 ) ;
#1813 = CARTESIAN_POINT ( 'NONE',  ( 0.4402108221923025089, -2.015156302359150331, 9.891980816076525684 ) ) ;
#1814 = CYLINDRICAL_SURFACE ( 'NONE', #15023, 1.750000000000001554 ) ;
#1815 = EDGE_LOOP ( 'NONE', ( #38601, #5434, #31334 ) ) ;
#1816 = CARTESIAN_POINT ( 'NONE',  ( 111.5540265531850679, 0.000000000000000000, -80.93171244307201562 ) ) ;
#1817 = FACE_OUTER_BOUND ( 'NONE', #16806, .T. ) ;
#1818 = CARTESIAN_POINT ( 'NONE',  ( -42.51732812238059722, -47.49695244670218131, 5.000000000000000000 ) ) ;
#1819 = CYLINDRICAL_SURFACE ( 'NONE', #30724, 1.750000000000015543 ) ;
#1820 = DIRECTION ( 'NONE',  ( 1.000000000000000000, -0.000000000000000000, -0.000000000000000000 ) ) ;
#1821 = ORIENTED_EDGE ( 'NONE', *, *, #4553, .F. ) ;
#1822 = CARTESIAN_POINT ( 'NONE',  ( 3.451199899302578977, -1.973209700276733480, 3.247138913692424467 ) ) ;
#1823 = VERTEX_POINT ( 'NONE', #35663 ) ;
#1824 = CARTESIAN_POINT ( 'NONE',  ( 36.08557433729230723, -35.58569447144768105, 7.455576670931136185 ) ) ;
#1825 = ORIENTED_EDGE ( 'NONE', *, *, #41293, .T. ) ;
#1826 = PLANE ( 'NONE',  #26243 ) ;
#1827 = PLANE ( 'NONE',  #9378 ) ;
#1828 = VECTOR ( 'NONE', #15724, 1000.000000000000000 ) ;
#1829 = CARTESIAN_POINT ( 'NONE',  ( -114.9999999999991047, 16.00000000000000000, 0.000000000000000000 ) ) ;
#1830 = EDGE_LOOP ( 'NONE', ( #15260, #39633, #17503, #99 ) ) ;
#1831 = EDGE_CURVE ( 'NONE', #2097, #37129, #16137, .T. ) ;
#1832 = DIRECTION ( 'NONE',  ( 0.000000000000000000, 0.000000000000000000, -1.000000000000000000 ) ) ;
#1833 = ORIENTED_EDGE ( 'NONE', *, *, #29322, .T. ) ;
#1834 = DIRECTION ( 'NONE',  ( 0.000000000000000000, 0.000000000000000000, 1.000000000000000000 ) ) ;
#1835 = FACE_OUTER_BOUND ( 'NONE', #10491, .T. ) ;
#1836 = CARTESIAN_POINT ( 'NONE',  ( -35.51846793572368455, 35.99772139009146343, 7.906207997025717304 ) ) ;
#1837 = CARTESIAN_POINT ( 'NONE',  ( -64.99999999999971578, 17.00000000000000000, -84.99999999999998579 ) ) ;
#1838 = VECTOR ( 'NONE', #35519, 1000.000000000000000 ) ;
#1839 = FACE_OUTER_BOUND ( 'NONE', #12739, .T. ) ;
#1840 = EDGE_LOOP ( 'NONE', ( #2850, #9840, #48262, #41892 ) ) ;
#1841 = ORIENTED_EDGE ( 'NONE', *, *, #15312, .T. ) ;
#1842 = CARTESIAN_POINT ( 'NONE',  ( -0.2050626648094178439, 1.807624707194796843, 9.903764339332081335 ) ) ;
#1843 = CIRCLE ( 'NONE', #32181, 0.4999999999999997224 ) ;
#1844 = EDGE_CURVE ( 'NONE', #27666, #42474, #27940, .T. ) ;
#1845 = ORIENTED_EDGE ( 'NONE', *, *, #9182, .T. ) ;
#1846 = EDGE_CURVE ( 'NONE', #34157, #42077, #39752, .T. ) ;
#1847 = AXIS2_PLACEMENT_3D ( 'NONE', #32204, #47802, #21146 ) ;
#1848 = CARTESIAN_POINT ( 'NONE',  ( 0.000000000000000000, 397.9839762253770346, 197.0020682315616796 ) ) ;
#1849 = CYLINDRICAL_SURFACE ( 'NONE', #5146, 1.750000000000001554 ) ;
#1850 = EDGE_LOOP ( 'NONE', ( #41128, #43176, #714, #3952, #8728 ) ) ;
#1851 = LINE ( 'NONE', #48748, #13088 ) ;
#1852 = EDGE_CURVE ( 'NONE', #22517, #47093, #8348, .T. ) ;
#1853 = CARTESIAN_POINT ( 'NONE',  ( -3.087186397306470820, -2.514307945609864259, -2.642742795433417058E-16 ) ) ;
#1854 = ORIENTED_EDGE ( 'NONE', *, *, #32860, .T. ) ;
#1855 = DIRECTION ( 'NONE',  ( 0.000000000000000000, 0.000000000000000000, -1.000000000000000000 ) ) ;
#1856 = CARTESIAN_POINT ( 'NONE',  ( -168.4459734468149463, 0.000000000000000000, 42.56828755692798438 ) ) ;
#1857 = EDGE_CURVE ( 'NONE', #12663, #29500, #44070, .T. ) ;
#1858 = DIRECTION ( 'NONE',  ( 0.000000000000000000, 0.000000000000000000, -1.000000000000000000 ) ) ;
#1859 = EDGE_CURVE ( 'NONE', #29900, #14767, #13571, .T. ) ;
#1860 = CARTESIAN_POINT ( 'NONE',  ( 75.05402655318509630, 2.143131898507880377E-16, -157.4317124430720014 ) ) ;
#1861 = VERTEX_POINT ( 'NONE', #10199 ) ;
#1862 = EDGE_LOOP ( 'NONE', ( #10679, #24004, #17988, #47529, #29113, #6209 ) ) ;
#1863 = PLANE ( 'NONE',  #11373 ) ;
#1864 = PLANE ( 'NONE',  #2561 ) ;
#1865 = EDGE_CURVE ( 'NONE', #12549, #9233, #37577, .T. ) ;
#1866 = DIRECTION ( 'NONE',  ( 1.000000000000000000, 0.000000000000000000, -0.000000000000000000 ) ) ;
#1867 = FACE_OUTER_BOUND ( 'NONE', #40919, .T. ) ;
#1868 = VECTOR ( 'NONE', #24949, 1000.000000000000000 ) ;
#1869 = FACE_OUTER_BOUND ( 'NONE', #41521, .T. ) ;
#1870 = ORIENTED_EDGE ( 'NONE', *, *, #39322, .T. ) ;
#1871 = DIRECTION ( 'NONE',  ( 1.000000000000000000, 0.000000000000000000, 0.000000000000000000 ) ) ;
#1872 = ORIENTED_EDGE ( 'NONE', *, *, #3267, .F. ) ;
#1873 = CARTESIAN_POINT ( 'NONE',  ( 210.0000000000000568, 0.000000000000000000, 40.81828755692798438 ) ) ;
#1874 = CARTESIAN_POINT ( 'NONE',  ( 224.9999999999999432, -175.0000000000000000, 500.0000000000000000 ) ) ;
#1875 = CARTESIAN_POINT ( 'NONE',  ( 153.3040265531850537, -1.750000000000010214, 40.81828755692798438 ) ) ;
#1876 = PLANE ( 'NONE',  #43014 ) ;
#1877 = CARTESIAN_POINT ( 'NONE',  ( -4.945973446814916130, -1.025126265847097207, -117.4317124430720014 ) ) ;
#1878 = VERTEX_POINT ( 'NONE', #33812 ) ;
#1879 = DIRECTION ( 'NONE',  ( 3.172065745548403743E-16, 1.000000000000000000, 0.000000000000000000 ) ) ;
#1880 = VECTOR ( 'NONE', #42551, 1000.000000000000000 ) ;
#1881 = DIRECTION ( 'NONE',  ( -1.000000000000000000, -0.000000000000000000, -0.000000000000000000 ) ) ;
#1882 = CARTESIAN_POINT ( 'NONE',  ( -44.94597344681493922, 2.143131898507880377E-16, 165.0000000000000000 ) ) ;
#1883 = CARTESIAN_POINT ( 'NONE',  ( -0.7849184246622071814, 1.242376769534369041, 9.958264684458713489 ) ) ;
#1884 = ORIENTED_EDGE ( 'NONE', *, *, #43377, .T. ) ;
#1885 = CIRCLE ( 'NONE', #37936, 4.000000000000003553 ) ;
#1886 = CYLINDRICAL_SURFACE ( 'NONE', #26163, 1.750000000000008438 ) ;
#1887 = ORIENTED_EDGE ( 'NONE', *, *, #32928, .T. ) ;
#1889 = ADVANCED_FACE ( 'NONE', ( #2243 ), #41176, .T. ) ;
#1888 = CARTESIAN_POINT ( 'NONE',  ( -7.303893058183219544, 3.196590768179758069, 3.455894424797545383E-16 ) ) ;
#1890 = CARTESIAN_POINT ( 'NONE',  ( 113.3040265531850537, 1.749999999999997335, 120.8182875569279702 ) ) ;
#1891 = LINE ( 'NONE', #18273, #4237 ) ;
#1892 = EDGE_CURVE ( 'NONE', #41332, #44274, #10449, .T. ) ;
#1893 = ORIENTED_EDGE ( 'NONE', *, *, #9050, .T. ) ;
#1894 =( BOUNDED_CURVE ( )  B_SPLINE_CURVE ( 3, ( #41568, #34150, #37741, #30036 ),
 .UNSPECIFIED., .F., .F. ) 
 B_SPLINE_CURVE_WITH_KNOTS ( ( 4, 4 ),
 ( 3.141592653589793116, 4.712388980384689674 ),
 .UNSPECIFIED. ) 
 CURVE ( )  GEOMETRIC_REPRESENTATION_ITEM ( )  RATIONAL_B_SPLINE_CURVE ( ( 1.000000000000000000, 0.8047378541243649375, 0.8047378541243649375, 1.000000000000000000 ) ) 
 REPRESENTATION_ITEM ( '' )  );
#1895 = CARTESIAN_POINT ( 'NONE',  ( -114.9999999999994031, 17.00000000000000000, -30.00000000000000000 ) ) ;
#1896 = DIRECTION ( 'NONE',  ( -1.000000000000000000, -0.000000000000000000, -0.000000000000000000 ) ) ;
#1897 = CARTESIAN_POINT ( 'NONE',  ( 191.5540265531851105, 0.000000000000000000, 122.5682875569279702 ) ) ;
#1898 = CYLINDRICAL_SURFACE ( 'NONE', #47107, 1.750000000000015543 ) ;
#1899 =( BOUNDED_CURVE ( )  B_SPLINE_CURVE ( 3, ( #48724, #49230, #21568, #2085 ),
 .UNSPECIFIED., .F., .F. ) 
 B_SPLINE_CURVE_WITH_KNOTS ( ( 4, 4 ),
 ( 1.570796326794896558, 3.141592653589793116 ),
 .UNSPECIFIED. ) 
 CURVE ( )  GEOMETRIC_REPRESENTATION_ITEM ( )  RATIONAL_B_SPLINE_CURVE ( ( 1.000000000000000000, 0.8047378541243649375, 0.8047378541243649375, 1.000000000000000000 ) ) 
 REPRESENTATION_ITEM ( '' )  );
#1900 = ORIENTED_EDGE ( 'NONE', *, *, #7055, .T. ) ;
#1901 = ORIENTED_EDGE ( 'NONE', *, *, #25875, .F. ) ;
#1902 = CARTESIAN_POINT ( 'NONE',  ( -2.538055338523173443, -33.28424297489108596, -9.367992836599951190 ) ) ;
#1903 = DIRECTION ( 'NONE',  ( -1.654361225106055350E-24, -1.654361225106055350E-24, 1.000000000000000000 ) ) ;
#1904 = VERTEX_POINT ( 'NONE', #5846 ) ;
#1905 = ORIENTED_EDGE ( 'NONE', *, *, #23688, .T. ) ;
#1906 = DIRECTION ( 'NONE',  ( 0.000000000000000000, 2.537652627714642000E-15, 1.000000000000000000 ) ) ;
#1907 = CARTESIAN_POINT ( 'NONE',  ( 181.0000000000000000, 165.0000000000000000, -342.0000000000001137 ) ) ;
#1908 = DIRECTION ( 'NONE',  ( -1.000000000000000000, 0.000000000000000000, 1.860490536778032451E-50 ) ) ;
#1909 = AXIS2_PLACEMENT_3D ( 'NONE', #12057, #9, #266 ) ;
#1910 = CARTESIAN_POINT ( 'NONE',  ( 195.0540265531851105, 2.143131898507880377E-16, 165.0000000000000000 ) ) ;
#1911 = ORIENTED_EDGE ( 'NONE', *, *, #42272, .T. ) ;
#1912 = VERTEX_POINT ( 'NONE', #14290 ) ;
#1913 = AXIS2_PLACEMENT_3D ( 'NONE', #28622, #40183, #13223 ) ;
#1914 = VERTEX_POINT ( 'NONE', #29443 ) ;
#1915 =( BOUNDED_CURVE ( )  B_SPLINE_CURVE ( 3, ( #26416, #22314, #37990, #2808 ),
 .UNSPECIFIED., .F., .F. ) 
 B_SPLINE_CURVE_WITH_KNOTS ( ( 4, 4 ),
 ( 4.712388980384689674, 6.283185307179586232 ),
 .UNSPECIFIED. ) 
 CURVE ( )  GEOMETRIC_REPRESENTATION_ITEM ( )  RATIONAL_B_SPLINE_CURVE ( ( 1.000000000000000000, 0.8047378541243649375, 0.8047378541243649375, 1.000000000000000000 ) ) 
 REPRESENTATION_ITEM ( '' )  );
#1916 = VECTOR ( 'NONE', #48903, 1000.000000000000000 ) ;
#1917 = CARTESIAN_POINT ( 'NONE',  ( 358.0000000000001137, 181.0000000000000284, 355.9999999999998295 ) ) ;
#1918 = DIRECTION ( 'NONE',  ( 5.473822126268816076E-48, -1.000000000000000000, -1.654361225106055350E-24 ) ) ;
#1919 = AXIS2_PLACEMENT_3D ( 'NONE', #37490, #44623, #28758 ) ;
#1920 = ORIENTED_EDGE ( 'NONE', *, *, #36078, .T. ) ;
#1921 = ORIENTED_EDGE ( 'NONE', *, *, #20459, .T. ) ;
#1922 = EDGE_CURVE ( 'NONE', #43357, #31210, #34071, .T. ) ;
#1923 = DIRECTION ( 'NONE',  ( 0.000000000000000000, 1.000000000000000000, 0.000000000000000000 ) ) ;
#1924 = CARTESIAN_POINT ( 'NONE',  ( 191.5540265531850537, -1.025126265847089213, -0.9317124430720324924 ) ) ;
#1925 = ORIENTED_EDGE ( 'NONE', *, *, #50399, .T. ) ;
#1926 = ORIENTED_EDGE ( 'NONE', *, *, #34329, .T. ) ;
#1927 = CARTESIAN_POINT ( 'NONE',  ( -3.231548175622898089, 9.463461120997347820, 9.282506307616472441 ) ) ;
#1928 = CARTESIAN_POINT ( 'NONE',  ( -30.21887974406478250, 14.69854701517551021, -8.016098858316205167 ) ) ;
#1929 = ORIENTED_EDGE ( 'NONE', *, *, #31783, .F. ) ;
#1930 = CARTESIAN_POINT ( 'NONE',  ( 164.9999999999999716, -174.9999999999999716, -344.0000000000001137 ) ) ;
#1931 = DIRECTION ( 'NONE',  ( -1.000000000000000000, 0.000000000000000000, 0.000000000000000000 ) ) ;
#1932 = LINE ( 'NONE', #10389, #25219 ) ;
#1933 = CARTESIAN_POINT ( 'NONE',  ( 169.0000000000000284, 165.0000000000000000, 355.9999999999998863 ) ) ;
#1934 = VECTOR ( 'NONE', #20913, 1000.000000000000000 ) ;
#1935 = CARTESIAN_POINT ( 'NONE',  ( -64.99999999999877787, 16.00000000000000000, 5.000000000000004441 ) ) ;
#1936 = EDGE_LOOP ( 'NONE', ( #15982, #1788, #659, #23682 ) ) ;
#1937 = DIRECTION ( 'NONE',  ( 0.000000000000000000, 0.000000000000000000, -1.000000000000000000 ) ) ;
#1938 = DIRECTION ( 'NONE',  ( -0.000000000000000000, -1.000000000000000000, -0.000000000000000000 ) ) ;
#1939 = CARTESIAN_POINT ( 'NONE',  ( 169.0000000000000284, -164.9999999999999432, 357.9999999999998863 ) ) ;
#1940 = CARTESIAN_POINT ( 'NONE',  ( 164.9999999999999716, -81.49999999999997158, -350.0000000000001705 ) ) ;
#1941 = DIRECTION ( 'NONE',  ( 0.000000000000000000, 0.000000000000000000, -1.000000000000000000 ) ) ;
#1942 = CYLINDRICAL_SURFACE ( 'NONE', #24536, 2.000000000000001776 ) ;
#1943 = VECTOR ( 'NONE', #24188, 1000.000000000000000 ) ;
#1944 = CARTESIAN_POINT ( 'NONE',  ( 181.0000000000000000, -81.49999999999997158, -340.0000000000001137 ) ) ;
#1945 = VECTOR ( 'NONE', #17455, 1000.000000000000000 ) ;
#1946 = FACE_OUTER_BOUND ( 'NONE', #38863, .T. ) ;
#1947 = DIRECTION ( 'NONE',  ( -1.000000000000000000, 0.000000000000000000, 0.000000000000000000 ) ) ;
#1948 = AXIS2_PLACEMENT_3D ( 'NONE', #12120, #40325, #32122 ) ;
#1949 = VECTOR ( 'NONE', #31036, 1000.000000000000000 ) ;
#1950 = ORIENTED_EDGE ( 'NONE', *, *, #18975, .T. ) ;
#1951 = CYLINDRICAL_SURFACE ( 'NONE', #46917, 1.750000000000001554 ) ;
#1952 = CARTESIAN_POINT ( 'NONE',  ( -0.3862712429686895876, 1.188820645368940720, 3.333333333333333481 ) ) ;
#1953 = CARTESIAN_POINT ( 'NONE',  ( -19.00512336303680883, 32.33518880947672614, -8.600750091277037157 ) ) ;
#1954 = DIRECTION ( 'NONE',  ( -0.000000000000000000, -0.000000000000000000, -1.000000000000000000 ) ) ;
#1955 = DIRECTION ( 'NONE',  ( -0.000000000000000000, -0.000000000000000000, -1.000000000000000000 ) ) ;
#1956 = ORIENTED_EDGE ( 'NONE', *, *, #49060, .F. ) ;
#1957 = B_SPLINE_SURFACE_WITH_KNOTS ( 'NONE', 3, 3, ( 
 ( #18458, #14611, #14873, #42562 ),
 ( #11539, #7441, #34382, #49719 ),
 ( #30788, #19210, #26677, #41811 ),
 ( #30522, #23065, #38740, #50212 ) ),
 .UNSPECIFIED., .F., .F., .F.,
 ( 4, 4 ),
 ( 4, 4 ),
 ( 0.000000000000000000, 1.000000000000000000 ),
 ( 0.000000000000000000, 1.000000000000000000 ),
 .UNSPECIFIED. ) ;
#1958 = ORIENTED_EDGE ( 'NONE', *, *, #22698, .T. ) ;
#1959 = CARTESIAN_POINT ( 'NONE',  ( -49.46074318306826001, 9.578883844007169301, 8.807470649214879543 ) ) ;
#1960 = CYLINDRICAL_SURFACE ( 'NONE', #905, 4.000000000000003553 ) ;
#1961 = AXIS2_PLACEMENT_3D ( 'NONE', #37355, #34239, #45491 ) ;
#1962 = ORIENTED_EDGE ( 'NONE', *, *, #5488, .T. ) ;
#1963 = CARTESIAN_POINT ( 'NONE',  ( 6.174150299305392053, -50.00000000000000711, 8.807470649214879543 ) ) ;
#1964 = DIRECTION ( 'NONE',  ( 1.000000000000000000, 0.000000000000000000, -2.312964634635864737E-16 ) ) ;
#1965 = ORIENTED_EDGE ( 'NONE', *, *, #42761, .F. ) ;
#1966 = ORIENTED_EDGE ( 'NONE', *, *, #5485, .F. ) ;
#1967 = CARTESIAN_POINT ( 'NONE',  ( 210.0000000000000568, 2.143131898507881116E-16, -40.93171244307203693 ) ) ;
#1968 = CARTESIAN_POINT ( 'NONE',  ( 80.00000000000186162, 17.00000000000000000, 90.00000000000000000 ) ) ;
#1969 = DIRECTION ( 'NONE',  ( -1.000000000000000000, 4.996003610813203446E-16, -1.033975765691284226E-24 ) ) ;
#1970 = ORIENTED_EDGE ( 'NONE', *, *, #23753, .T. ) ;
#1971 = CARTESIAN_POINT ( 'NONE',  ( 40.00000000000000000, 4.898587196589413026E-15, 897.6604670114603550 ) ) ;
#1972 = AXIS2_PLACEMENT_3D ( 'NONE', #21850, #37515, #2333 ) ;
#1973 = CARTESIAN_POINT ( 'NONE',  ( 33.30402655318503946, 1.750000000000010658, 120.8182875569279702 ) ) ;
#1974 = CARTESIAN_POINT ( 'NONE',  ( -114.9999999999997158, 17.00000000000000000, -60.00000000000000000 ) ) ;
#1975 = VERTEX_POINT ( 'NONE', #13532 ) ;
#1976 = EDGE_LOOP ( 'NONE', ( #15294, #42100, #49619, #25944 ) ) ;
#1977 = ORIENTED_EDGE ( 'NONE', *, *, #7701, .T. ) ;
#1978 = DIRECTION ( 'NONE',  ( 1.000000000000000000, 0.000000000000000000, 0.000000000000000000 ) ) ;
#1979 = EDGE_CURVE ( 'NONE', #16294, #12217, #29956, .T. ) ;
#1980 = VECTOR ( 'NONE', #46135, 1000.000000000000000 ) ;
#1981 = CARTESIAN_POINT ( 'NONE',  ( 169.0000000000000000, -174.9999999999999716, -97.00000000000014211 ) ) ;
#1982 = ORIENTED_EDGE ( 'NONE', *, *, #10169, .F. ) ;
#1983 = EDGE_CURVE ( 'NONE', #7644, #20370, #41239, .T. ) ;
#1984 = CARTESIAN_POINT ( 'NONE',  ( 210.0000000000000568, 2.143131898507881856E-16, 79.06828755692797017 ) ) ;
#1985 = CARTESIAN_POINT ( 'NONE',  ( -0.2401930789658029419, -1.414287202658127685, 9.950105812514292936 ) ) ;
#1986 = ADVANCED_FACE ( 'NONE', ( #25345 ), #40750, .F. ) ;
#1987 = CARTESIAN_POINT ( 'NONE',  ( 0.000000000000000000, -175.0000000000000284, 350.0000000000002274 ) ) ;
#1988 = CARTESIAN_POINT ( 'NONE',  ( 169.0000000000000000, -174.9999999999999716, -95.00000000000014211 ) ) ;
#1989 = CARTESIAN_POINT ( 'NONE',  ( 36.62549812225761769, 8.082823558958848409, -8.600750091277037157 ) ) ;
#1990 = PLANE ( 'NONE',  #14461 ) ;
#1991 = ADVANCED_FACE ( 'NONE', ( #1748 ), #9635, .T. ) ;
#1992 = DIRECTION ( 'NONE',  ( -0.000000000000000000, -0.000000000000000000, -1.000000000000000000 ) ) ;
#1993 = FACE_OUTER_BOUND ( 'NONE', #14346, .T. ) ;
#1994 = ADVANCED_FACE ( 'NONE', ( #23255 ), #26608, .T. ) ;
#1995 = CARTESIAN_POINT ( 'NONE',  ( 0.000000000000000000, -62.49999999999998579, 0.000000000000000000 ) ) ;
#1996 = ADVANCED_FACE ( 'NONE', ( #30458 ), #10695, .T. ) ;
#1997 = CARTESIAN_POINT ( 'NONE',  ( 112.2789002873379758, 1.749999999999996225, -158.1565861772249377 ) ) ;
#1998 = DIRECTION ( 'NONE',  ( 1.000000000000000000, 0.000000000000000000, 0.000000000000000000 ) ) ;
#1999 = EDGE_LOOP ( 'NONE', ( #37853, #12484 ) ) ;
#2000 = CARTESIAN_POINT ( 'NONE',  ( -164.4973046169135955, -66.40178110878292728, -93.79675437945473959 ) ) ;
#2001 = DIRECTION ( 'NONE',  ( -1.000000000000000000, -0.000000000000000000, -0.000000000000000000 ) ) ;
#2002 = EDGE_CURVE ( 'NONE', #37195, #28486, #15058, .T. ) ;
#2003 = ADVANCED_FACE ( 'NONE', ( #30721 ), #22499, .T. ) ;
#2004 = FACE_OUTER_BOUND ( 'NONE', #22418, .T. ) ;
#2006 = ORIENTED_EDGE ( 'NONE', *, *, #12062, .T. ) ;
#2005 = EDGE_CURVE ( 'NONE', #47191, #2839, #26858, .T. ) ;
#2007 = CARTESIAN_POINT ( 'NONE',  ( -86.69597344681494633, 1.750000000000010658, -119.1817124430720440 ) ) ;
#2008 = EDGE_CURVE ( 'NONE', #36250, #23942, #18637, .T. ) ;
#2009 = DIRECTION ( 'NONE',  ( 0.000000000000000000, 0.000000000000000000, 1.000000000000000000 ) ) ;
#2010 = VECTOR ( 'NONE', #2165, 1000.000000000000000 ) ;
#2011 = ORIENTED_EDGE ( 'NONE', *, *, #2047, .T. ) ;
#2012 = CYLINDRICAL_SURFACE ( 'NONE', #25510, 1.750000000000001554 ) ;
#2013 = ADVANCED_FACE ( 'NONE', ( #42003 ), #22754, .T. ) ;
#2014 = CARTESIAN_POINT ( 'NONE',  ( -14.99999999999970868, 16.00000000000000000, -84.99999999999998579 ) ) ;
#2015 = AXIS2_PLACEMENT_3D ( 'NONE', #44272, #17345, #9648 ) ;
#2016 = CARTESIAN_POINT ( 'NONE',  ( 151.5540265531850537, 0.000000000000000000, -117.4317124430720725 ) ) ;
#2017 = DIRECTION ( 'NONE',  ( 0.000000000000000000, -1.000000000000000000, 0.000000000000000000 ) ) ;
#2018 = EDGE_CURVE ( 'NONE', #19301, #5374, #45810, .T. ) ;
#2019 = VERTEX_POINT ( 'NONE', #22997 ) ;
#2020 = CARTESIAN_POINT ( 'NONE',  ( 75.05402655318509630, 2.143131898507880377E-16, -117.4317124430720156 ) ) ;
#2021 = VERTEX_POINT ( 'NONE', #7112 ) ;
#2022 = VERTEX_POINT ( 'NONE', #50418 ) ;
#2023 = CARTESIAN_POINT ( 'NONE',  ( -14.99999999999782041, 17.00000000000000000, 95.00000000000000000 ) ) ;
#2024 = ORIENTED_EDGE ( 'NONE', *, *, #18436, .T. ) ;
#2025 = CARTESIAN_POINT ( 'NONE',  ( 4.592425496802573972E-16, 23.48684210526316107, 3.750000000000000000 ) ) ;
#2026 = ORIENTED_EDGE ( 'NONE', *, *, #48076, .T. ) ;
#2027 = DIRECTION ( 'NONE',  ( -3.364279341222521245E-16, -0.7071067811865474617, 0.7071067811865476838 ) ) ;
#2028 = CYLINDRICAL_SURFACE ( 'NONE', #21636, 1.749999999999987566 ) ;
#2029 = DIRECTION ( 'NONE',  ( -1.000000000000000000, 0.000000000000000000, -0.000000000000000000 ) ) ;
#2030 = EDGE_CURVE ( 'NONE', #19110, #1049, #17178, .T. ) ;
#2031 = ORIENTED_EDGE ( 'NONE', *, *, #39450, .F. ) ;
#2032 = LINE ( 'NONE', #36962, #2633 ) ;
#2033 = VECTOR ( 'NONE', #32426, 1000.000000000000000 ) ;
#2034 = ADVANCED_FACE ( 'NONE', ( #2995 ), #40768, .T. ) ;
#2035 = VERTEX_POINT ( 'NONE', #4525 ) ;
#2036 = EDGE_CURVE ( 'NONE', #34157, #44875, #35350, .T. ) ;
#2037 = CARTESIAN_POINT ( 'NONE',  ( 42.99990394833793061, 47.95759300784327905, -5.000000000000000000 ) ) ;
#2038 = CARTESIAN_POINT ( 'NONE',  ( 344.0000000000000000, 165.0000000000000000, -340.0000000000001137 ) ) ;
#2039 = VERTEX_POINT ( 'NONE', #35599 ) ;
#2040 = AXIS2_PLACEMENT_3D ( 'NONE', #24732, #40384, #5220 ) ;
#2041 = ORIENTED_EDGE ( 'NONE', *, *, #38374, .F. ) ;
#2042 = VERTEX_POINT ( 'NONE', #31993 ) ;
#2043 = DIRECTION ( 'NONE',  ( -0.000000000000000000, -1.000000000000000000, -0.000000000000000000 ) ) ;
#2044 = EDGE_CURVE ( 'NONE', #38025, #4851, #20418, .T. ) ;
#2045 = LINE ( 'NONE', #47938, #29961 ) ;
#2046 = EDGE_LOOP ( 'NONE', ( #43481, #9210, #37838, #21818, #19453, #27829, #8404, #30225 ) ) ;
#2047 = EDGE_CURVE ( 'NONE', #35257, #35256, #8875, .T. ) ;
#2048 = DIRECTION ( 'NONE',  ( 0.000000000000000000, -2.537652627714643577E-15, -1.000000000000000000 ) ) ;
#2049 = CARTESIAN_POINT ( 'NONE',  ( 7.500000000000000000, 224.9999999999999716, -240.0000000000000000 ) ) ;
#2050 = FACE_OUTER_BOUND ( 'NONE', #45912, .T. ) ;
#2051 = EDGE_LOOP ( 'NONE', ( #4881, #9393, #45610, #17203, #16422, #32497, #38156, #30559 ) ) ;
#2052 = AXIS2_PLACEMENT_3D ( 'NONE', #21375, #33699, #25745 ) ;
#2053 = CARTESIAN_POINT ( 'NONE',  ( -7.241383964640739634, -3.469446951953614189E-15, -5.000000000000000000 ) ) ;
#2054 = FACE_OUTER_BOUND ( 'NONE', #36715, .T. ) ;
#2055 =( BOUNDED_CURVE ( )  B_SPLINE_CURVE ( 3, ( #37071, #21383, #17037, #25753 ),
 .UNSPECIFIED., .F., .F. ) 
 B_SPLINE_CURVE_WITH_KNOTS ( ( 4, 4 ),
 ( 3.141592653589793116, 4.712388980384689674 ),
 .UNSPECIFIED. ) 
 CURVE ( )  GEOMETRIC_REPRESENTATION_ITEM ( )  RATIONAL_B_SPLINE_CURVE ( ( 1.000000000000000000, 0.8047378541243649375, 0.8047378541243649375, 1.000000000000000000 ) ) 
 REPRESENTATION_ITEM ( '' )  );
#2056 = CARTESIAN_POINT ( 'NONE',  ( -14.86945752723352498, -7.944783388878907004, 2.590526750877053086 ) ) ;
#2057 = AXIS2_PLACEMENT_3D ( 'NONE', #20662, #32722, #16822 ) ;
#2058 = ADVANCED_FACE ( 'NONE', ( #39693 ), #31486, .F. ) ;
#2059 = VERTEX_POINT ( 'NONE', #47332 ) ;
#2060 = CARTESIAN_POINT ( 'NONE',  ( 72.27890028733797578, 1.750000000000009548, -78.15658617722490931 ) ) ;
#2061 = B_SPLINE_CURVE_WITH_KNOTS ( 'NONE', 3,
 ( #46805, #2973, #50648, #27619 ),
 .UNSPECIFIED., .F., .F.,
 ( 4, 4 ),
 ( 0.0008438930667322229028, 0.001027058643692256579 ),
 .UNSPECIFIED. ) ;
#2062 = EDGE_CURVE ( 'NONE', #44581, #5075, #47588, .T. ) ;
#2063 = CARTESIAN_POINT ( 'NONE',  ( -45.42829307628559832, -21.98948915213271960, 8.356839323120299312 ) ) ;
#2064 = FACE_OUTER_BOUND ( 'NONE', #10931, .T. ) ;
#2065 = ORIENTED_EDGE ( 'NONE', *, *, #1387, .F. ) ;
#2066 = CARTESIAN_POINT ( 'NONE',  ( -8.445973446814964092, 1.025126265847097207, 122.5682875569280128 ) ) ;
#2067 = CARTESIAN_POINT ( 'NONE',  ( 0.1475726264153646716, 1.496347932843221429, 9.927319414211224213 ) ) ;
#2068 = LINE ( 'NONE', #13349, #48206 ) ;
#2069 = CARTESIAN_POINT ( 'NONE',  ( -2.462075149652696027, 16.57295996686994499, 9.403735324607438884 ) ) ;
#2070 = DIRECTION ( 'NONE',  ( 0.000000000000000000, 0.000000000000000000, -1.000000000000000000 ) ) ;
#2072 = ORIENTED_EDGE ( 'NONE', *, *, #5771, .T. ) ;
#2071 = EDGE_CURVE ( 'NONE', #43863, #40138, #23778, .T. ) ;
#2073 = VECTOR ( 'NONE', #34325, 1000.000000000000000 ) ;
#2074 = LINE ( 'NONE', #40570, #4337 ) ;
#2075 = ADVANCED_FACE ( 'NONE', ( #43515 ), #35854, .T. ) ;
#2076 = ORIENTED_EDGE ( 'NONE', *, *, #10770, .F. ) ;
#2077 = CYLINDRICAL_SURFACE ( 'NONE', #20479, 1.750000000000010214 ) ;
#2078 = VECTOR ( 'NONE', #9444, 1000.000000000000227 ) ;
#2079 = ORIENTED_EDGE ( 'NONE', *, *, #4226, .T. ) ;
#2080 = EDGE_CURVE ( 'NONE', #26957, #35927, #31747, .T. ) ;
#2081 = DIRECTION ( 'NONE',  ( 0.000000000000000000, -1.000000000000000000, -0.000000000000000000 ) ) ;
#2082 = CARTESIAN_POINT ( 'NONE',  ( 210.0000000000000568, 2.143131898507881856E-16, -80.93171244307202983 ) ) ;
#2083 = EDGE_CURVE ( 'NONE', #11343, #22517, #18803, .T. ) ;
#2084 = AXIS2_PLACEMENT_3D ( 'NONE', #35793, #19594, #621 ) ;
#2085 = CARTESIAN_POINT ( 'NONE',  ( -164.9459734468149747, 0.000000000000000000, 162.5682875569279702 ) ) ;
#2086 = VERTEX_POINT ( 'NONE', #15819 ) ;
#2087 = EDGE_CURVE ( 'NONE', #46411, #12768, #49540, .T. ) ;
#2088 = LINE ( 'NONE', #17475, #45768 ) ;
#2089 = ORIENTED_EDGE ( 'NONE', *, *, #43773, .T. ) ;
#2090 = FACE_OUTER_BOUND ( 'NONE', #16667, .T. ) ;
#2091 = CARTESIAN_POINT ( 'NONE',  ( 0.9001353430043829151, 1.054615064032355498, 9.960027343377989340 ) ) ;
#2092 = AXIS2_PLACEMENT_3D ( 'NONE', #39484, #32035, #23299 ) ;
#2093 = CARTESIAN_POINT ( 'NONE',  ( 115.0540265531850395, 1.025126265847081664, -157.4317124430720582 ) ) ;
#2094 = CARTESIAN_POINT ( 'NONE',  ( -19.99999999999878142, 16.00000000000000000, 5.000000000000004441 ) ) ;
#2095 = CARTESIAN_POINT ( 'NONE',  ( -46.69597344681494633, 0.000000000000000000, 165.0000000000000000 ) ) ;
#2096 = ORIENTED_EDGE ( 'NONE', *, *, #29840, .F. ) ;
#2097 = VERTEX_POINT ( 'NONE', #4278 ) ;
#2098 = CARTESIAN_POINT ( 'NONE',  ( 191.5540265531850537, 1.025126265847089213, 159.0682875569279418 ) ) ;
#2099 = VECTOR ( 'NONE', #44927, 1000.000000000000000 ) ;
#2100 = ORIENTED_EDGE ( 'NONE', *, *, #4279, .T. ) ;
#2101 = EDGE_CURVE ( 'NONE', #9119, #32429, #27886, .T. ) ;
#2102 = DIRECTION ( 'NONE',  ( -0.000000000000000000, -0.000000000000000000, -1.000000000000000000 ) ) ;
#2103 = CARTESIAN_POINT ( 'NONE',  ( 168.9999999999999716, -93.49999999999997158, -115.0000000000001563 ) ) ;
#2104 = ORIENTED_EDGE ( 'NONE', *, *, #2924, .F. ) ;
#2105 = CARTESIAN_POINT ( 'NONE',  ( -19.99999999999783995, 17.00000000000000000, 95.00000000000000000 ) ) ;
#2106 = CARTESIAN_POINT ( 'NONE',  ( 344.0000000000000568, 165.0000000000000000, 339.9999999999998295 ) ) ;
#2107 = ORIENTED_EDGE ( 'NONE', *, *, #15288, .T. ) ;
#2108 = CARTESIAN_POINT ( 'NONE',  ( 80.00000000000186162, 16.00000000000000000, 65.00000000000000000 ) ) ;
#2109 = CARTESIAN_POINT ( 'NONE',  ( -46.11867747200562917, 19.86470446310265103, -8.016098858316199838 ) ) ;
#2110 = CARTESIAN_POINT ( 'NONE',  ( 9.760995290733820440, -2.173239732351728293, 9.646707543097347681 ) ) ;
#2111 = CARTESIAN_POINT ( 'NONE',  ( -1.104609456715841986, -0.6504863887005195577, 9.948547179989617462 ) ) ;
#2112 = VECTOR ( 'NONE', #2639, 1000.000000000000000 ) ;
#2113 = ORIENTED_EDGE ( 'NONE', *, *, #11138, .T. ) ;
#2114 = ORIENTED_EDGE ( 'NONE', *, *, #45262, .T. ) ;
#2115 = CARTESIAN_POINT ( 'NONE',  ( 168.9999999999999716, -184.9999999999999716, -360.0000000000002274 ) ) ;
#2116 = B_SPLINE_CURVE_WITH_KNOTS ( 'NONE', 3,
 ( #28303, #36783, #31916, #32662 ),
 .UNSPECIFIED., .F., .F.,
 ( 4, 4 ),
 ( 3.127317220692750759E-18, 0.002458791966311098948 ),
 .UNSPECIFIED. ) ;
#2117 = DIRECTION ( 'NONE',  ( 0.000000000000000000, -0.9253776417389547593, -0.3790464617558786942 ) ) ;
#2118 = EDGE_CURVE ( 'NONE', #35523, #46762, #44012, .T. ) ;
#2119 = DIRECTION ( 'NONE',  ( -1.000000000000000000, 0.000000000000000000, 0.000000000000000000 ) ) ;
#2120 = VECTOR ( 'NONE', #33876, 1000.000000000000000 ) ;
#2121 = CARTESIAN_POINT ( 'NONE',  ( -46.69597344681494633, 1.750000000000010658, -79.18171244307201562 ) ) ;
#2122 = ORIENTED_EDGE ( 'NONE', *, *, #44011, .T. ) ;
#2123 = LINE ( 'NONE', #49009, #11921 ) ;
#2124 = ORIENTED_EDGE ( 'NONE', *, *, #7316, .T. ) ;
#2125 =( GEOMETRIC_REPRESENTATION_CONTEXT ( 3 ) GLOBAL_UNCERTAINTY_ASSIGNED_CONTEXT ( ( #15805 ) ) GLOBAL_UNIT_ASSIGNED_CONTEXT ( ( #47360, #50706, #15603 ) ) REPRESENTATION_CONTEXT ( 'NONE', 'WORKASPACE' ) );
#2126 = FACE_OUTER_BOUND ( 'NONE', #28340, .T. ) ;
#2127 = DIRECTION ( 'NONE',  ( 1.000000000000000000, -0.000000000000000000, -0.000000000000000000 ) ) ;
#2128 = CARTESIAN_POINT ( 'NONE',  ( 224.9999999999999716, -164.9999999999999716, 444.9999999999998295 ) ) ;
#2129 = CARTESIAN_POINT ( 'NONE',  ( -4.945973446814903696, 2.143131898507912917E-16, -117.4317124430720156 ) ) ;
#2130 = CARTESIAN_POINT ( 'NONE',  ( -45.67084718096785423, 1.750000000000010214, -120.2068387089191219 ) ) ;
#2131 = VERTEX_POINT ( 'NONE', #8637 ) ;
#2132 = CARTESIAN_POINT ( 'NONE',  ( 356.0000000000000000, 183.0000000000000284, -358.0000000000002842 ) ) ;
#2133 = PLANE ( 'NONE',  #45719 ) ;
#2134 = DIRECTION ( 'NONE',  ( 1.000000000000000000, 0.000000000000000000, -0.000000000000000000 ) ) ;
#2135 = VECTOR ( 'NONE', #16795, 1000.000000000000000 ) ;
#2136 = ADVANCED_FACE ( 'NONE', ( #39943 ), #33418, .T. ) ;
#2137 = CARTESIAN_POINT ( 'NONE',  ( -0.7604583772867632430, 1.297021979207275466, 9.944962737436837230 ) ) ;
#2138 = EDGE_CURVE ( 'NONE', #27259, #5809, #11372, .T. ) ;
#2139 = VERTEX_POINT ( 'NONE', #50063 ) ;
#2140 =( BOUNDED_CURVE ( )  B_SPLINE_CURVE ( 3, ( #33015, #47850, #44517, #12741 ),
 .UNSPECIFIED., .F., .F. ) 
 B_SPLINE_CURVE_WITH_KNOTS ( ( 4, 4 ),
 ( 1.570796326794896558, 3.141592653589793116 ),
 .UNSPECIFIED. ) 
 CURVE ( )  GEOMETRIC_REPRESENTATION_ITEM ( )  RATIONAL_B_SPLINE_CURVE ( ( 1.000000000000000000, 0.8047378541243649375, 0.8047378541243649375, 1.000000000000000000 ) ) 
 REPRESENTATION_ITEM ( '' )  );
#2141 = FACE_OUTER_BOUND ( 'NONE', #19435, .T. ) ;
#2142 = ORIENTED_EDGE ( 'NONE', *, *, #40307, .F. ) ;
#2143 = CARTESIAN_POINT ( 'NONE',  ( 72.27890028733797578, -1.750000000000010214, -78.15658617722490931 ) ) ;
#2144 = CARTESIAN_POINT ( 'NONE',  ( 0.9358216137850741134, -0.9039474357314646324, 9.986087673579140400 ) ) ;
#2145 = ADVANCED_FACE ( 'NONE', ( #38849 ), #14973, .T. ) ;
#2146 = CARTESIAN_POINT ( 'NONE',  ( -0.3370904143228927730, -0.2449105217885335917, -10.00000000000000000 ) ) ;
#2147 = EDGE_CURVE ( 'NONE', #4051, #45035, #26522, .T. ) ;
#2148 = ADVANCED_FACE ( 'NONE', ( #22919 ), #46235, .T. ) ;
#2149 = AXIS2_PLACEMENT_3D ( 'NONE', #39779, #12555, #7716 ) ;
#2150 = VECTOR ( 'NONE', #4374, 1000.000000000000000 ) ;
#2151 = CARTESIAN_POINT ( 'NONE',  ( 46.76852358249013975, -17.86468378716709182, -9.367992836599951190 ) ) ;
#2152 = LINE ( 'NONE', #37326, #22207 ) ;
#2153 = AXIS2_PLACEMENT_3D ( 'NONE', #23373, #24400, #27731 ) ;
#2154 = LINE ( 'NONE', #26261, #29470 ) ;
#2155 = CARTESIAN_POINT ( 'NONE',  ( -6.695973446814940111, -1.750000000000023315, 0.8182875569279768335 ) ) ;
#2156 = ADVANCED_FACE ( 'NONE', ( #11635 ), #23175, .F. ) ;
#2157 = ORIENTED_EDGE ( 'NONE', *, *, #8118, .T. ) ;
#2158 = VERTEX_POINT ( 'NONE', #43184 ) ;
#2159 = CARTESIAN_POINT ( 'NONE',  ( -225.0000000000000568, 175.0000000000000000, 500.0000000000000000 ) ) ;
#2160 = CARTESIAN_POINT ( 'NONE',  ( 48.33712804702526000, 13.03701565032775456, -9.367992836599954742 ) ) ;
#2161 = VECTOR ( 'NONE', #28800, 1000.000000000000000 ) ;
#2162 = EDGE_LOOP ( 'NONE', ( #42165, #11431, #22910, #39612 ) ) ;
#2163 = EDGE_LOOP ( 'NONE', ( #44906, #42703, #11861, #33184 ) ) ;
#2164 = CARTESIAN_POINT ( 'NONE',  ( 155.0540265531850537, 2.143131898507880377E-16, -77.43171244307204404 ) ) ;
#2165 = DIRECTION ( 'NONE',  ( 0.000000000000000000, -2.265761274745217480E-16, 1.000000000000000000 ) ) ;
#2166 = CARTESIAN_POINT ( 'NONE',  ( 34.32915281903212446, -1.750000000000009548, -78.15658617722490931 ) ) ;
#2167 = CARTESIAN_POINT ( 'NONE',  ( 339.9999999999999432, 169.0000000000000000, -360.0000000000002274 ) ) ;
#2168 = VECTOR ( 'NONE', #40547, 1000.000000000000000 ) ;
#2169 = ORIENTED_EDGE ( 'NONE', *, *, #17078, .F. ) ;
#2170 = ORIENTED_EDGE ( 'NONE', *, *, #41182, .T. ) ;
#2171 = CIRCLE ( 'NONE', #12823, 1.750000000000015543 ) ;
#2172 = FACE_OUTER_BOUND ( 'NONE', #36485, .T. ) ;
#2173 = DIRECTION ( 'NONE',  ( -0.000000000000000000, -1.000000000000000000, -0.000000000000000000 ) ) ;
#2174 = ORIENTED_EDGE ( 'NONE', *, *, #25665, .F. ) ;
#2175 = ORIENTED_EDGE ( 'NONE', *, *, #25307, .F. ) ;
#2176 = LINE ( 'NONE', #11381, #9477 ) ;
#2177 = LINE ( 'NONE', #10380, #18316 ) ;
#2178 = ORIENTED_EDGE ( 'NONE', *, *, #39801, .T. ) ;
#2179 = ORIENTED_EDGE ( 'NONE', *, *, #7975, .F. ) ;
#2180 = EDGE_CURVE ( 'NONE', #169, #35061, #50319, .T. ) ;
#2181 = CARTESIAN_POINT ( 'NONE',  ( 135.0000000000021600, 16.00000000000000000, 115.0000000000000142 ) ) ;
#2182 = DIRECTION ( 'NONE',  ( -1.000000000000000000, -0.000000000000000000, -0.000000000000000000 ) ) ;
#2183 = ORIENTED_EDGE ( 'NONE', *, *, #7997, .F. ) ;
#2184 = CARTESIAN_POINT ( 'NONE',  ( -48.44597344681496054, -1.025126265847089879, -77.43171244307200141 ) ) ;
#2185 = PLANE ( 'NONE',  #27691 ) ;
#2186 = PLANE ( 'NONE',  #50543 ) ;
#2187 = CYLINDRICAL_SURFACE ( 'NONE', #42517, 4.000000000000003553 ) ;
#2188 = CARTESIAN_POINT ( 'NONE',  ( 168.9999999999999716, -184.9999999999999716, -342.0000000000001137 ) ) ;
#2189 = PRESENTATION_LAYER_ASSIGNMENT (  '', '', ( #15308 ) ) ;
#2190 = ORIENTED_EDGE ( 'NONE', *, *, #135, .T. ) ;
#2191 = CARTESIAN_POINT ( 'NONE',  ( -204.9459734468149463, 2.143131898507880377E-16, 165.0000000000000000 ) ) ;
#2192 = CARTESIAN_POINT ( 'NONE',  ( 240.0000000000000000, -175.0000000000000000, 62.29650858650038003 ) ) ;
#2193 = FACE_OUTER_BOUND ( 'NONE', #40521, .T. ) ;
#2194 = FACE_OUTER_BOUND ( 'NONE', #13713, .T. ) ;
#2195 =( BOUNDED_CURVE ( )  B_SPLINE_CURVE ( 3, ( #16084, #47336, #19672, #35358 ),
 .UNSPECIFIED., .F., .F. ) 
 B_SPLINE_CURVE_WITH_KNOTS ( ( 4, 4 ),
 ( 0.000000000000000000, 1.570796326794896558 ),
 .UNSPECIFIED. ) 
 CURVE ( )  GEOMETRIC_REPRESENTATION_ITEM ( )  RATIONAL_B_SPLINE_CURVE ( ( 1.000000000000000000, 0.8047378541243649375, 0.8047378541243649375, 1.000000000000000000 ) ) 
 REPRESENTATION_ITEM ( '' )  );
#2196 = DIRECTION ( 'NONE',  ( 0.000000000000000000, -1.000000000000000000, -3.186989995019654210E-49 ) ) ;
#2197 = CARTESIAN_POINT ( 'NONE',  ( 72.27890028733797578, -1.750000000000010214, 121.8434138227750623 ) ) ;
#2198 = CYLINDRICAL_SURFACE ( 'NONE', #5680, 2.000000000000001776 ) ;
#2199 = CARTESIAN_POINT ( 'NONE',  ( 344.0000000000000000, 185.0000000000000284, -360.0000000000002274 ) ) ;
#2200 =( BOUNDED_CURVE ( )  B_SPLINE_CURVE ( 3, ( #18719, #41836, #11041, #45146 ),
 .UNSPECIFIED., .F., .F. ) 
 B_SPLINE_CURVE_WITH_KNOTS ( ( 4, 4 ),
 ( 1.570796326794896558, 3.141592653589793116 ),
 .UNSPECIFIED. ) 
 CURVE ( )  GEOMETRIC_REPRESENTATION_ITEM ( )  RATIONAL_B_SPLINE_CURVE ( ( 1.000000000000000000, 0.8047378541243649375, 0.8047378541243649375, 1.000000000000000000 ) ) 
 REPRESENTATION_ITEM ( '' )  );
#2201 = FACE_OUTER_BOUND ( 'NONE', #47299, .T. ) ;
#2202 = VECTOR ( 'NONE', #33848, 1000.000000000000000 ) ;
#2203 = EDGE_CURVE ( 'NONE', #37192, #42338, #42157, .T. ) ;
#2204 = EDGE_LOOP ( 'NONE', ( #30820, #13242, #49742, #5430 ) ) ;
#2205 = CARTESIAN_POINT ( 'NONE',  ( 24.19621561048219149, 28.69654500124514129, -5.338708898921616708 ) ) ;
#2206 = CARTESIAN_POINT ( 'NONE',  ( -15.00099850811941948, -7.462898891544107016, 9.403735324607438884 ) ) ;
#2207 = CARTESIAN_POINT ( 'NONE',  ( 210.0000000000000568, 0.000000000000000000, 122.5682875569279844 ) ) ;
#2208 = EDGE_CURVE ( 'NONE', #44283, #11192, #19323, .T. ) ;
#2209 = CARTESIAN_POINT ( 'NONE',  ( 30.25247992116058526, -39.82368563463805344, -3.760136334089591248 ) ) ;
#2210 = DIRECTION ( 'NONE',  ( 0.000000000000000000, 0.000000000000000000, 1.000000000000000000 ) ) ;
#2211 = ORIENTED_EDGE ( 'NONE', *, *, #2519, .F. ) ;
#2212 = VERTEX_POINT ( 'NONE', #27023 ) ;
#2213 = CARTESIAN_POINT ( 'NONE',  ( -5.647304616913629616, 160.1880105690400171, 472.8425600500173118 ) ) ;
#2214 = CARTESIAN_POINT ( 'NONE',  ( 185.0000000000000000, -81.49999999999997158, -340.0000000000001137 ) ) ;
#2215 = AXIS2_PLACEMENT_3D ( 'NONE', #38167, #22491, #25842 ) ;
#2216 = ORIENTED_EDGE ( 'NONE', *, *, #21301, .F. ) ;
#2217 = CARTESIAN_POINT ( 'NONE',  ( -0.3370904143228943828, -0.2449105217885308716, 10.00000000000000000 ) ) ;
#2218 = DIRECTION ( 'NONE',  ( 0.000000000000000000, 0.000000000000000000, 1.000000000000000000 ) ) ;
#2219 = ORIENTED_EDGE ( 'NONE', *, *, #45089, .F. ) ;
#2220 = EDGE_LOOP ( 'NONE', ( #34116, #19277, #21719, #1477 ) ) ;
#2221 = ORIENTED_EDGE ( 'NONE', *, *, #5750, .F. ) ;
#2222 = CARTESIAN_POINT ( 'NONE',  ( 193.3040265531851105, -1.750000000000010658, 120.8182875569279702 ) ) ;
#2223 = CARTESIAN_POINT ( 'NONE',  ( 37.27397286063867199, -4.111076158911552092, 7.697694107796188234 ) ) ;
#2224 = LINE ( 'NONE', #40973, #47164 ) ;
#2225 = ORIENTED_EDGE ( 'NONE', *, *, #29896, .T. ) ;
#2226 = LINE ( 'NONE', #6578, #11231 ) ;
#2227 = DIRECTION ( 'NONE',  ( 1.000000000000000000, -4.758098676964956461E-16, -8.975803739141899931E-48 ) ) ;
#2228 = VERTEX_POINT ( 'NONE', #15237 ) ;
#2229 = ORIENTED_EDGE ( 'NONE', *, *, #21930, .T. ) ;
#2230 = CARTESIAN_POINT ( 'NONE',  ( 112.2789002873379758, -1.749999999999996669, 159.7931612910809065 ) ) ;
#2231 = CARTESIAN_POINT ( 'NONE',  ( 341.9999999999999432, 169.0000000000000568, -344.0000000000002842 ) ) ;
#2232 = CARTESIAN_POINT ( 'NONE',  ( -204.9459734468149463, 2.143131898507880377E-16, -160.9317124430720014 ) ) ;
#2233 = ORIENTED_EDGE ( 'NONE', *, *, #16780, .F. ) ;
#2234 = ADVANCED_FACE ( 'NONE', ( #38594 ), #34751, .T. ) ;
#2235 = CARTESIAN_POINT ( 'NONE',  ( 111.5540265531850537, -1.025126265847082108, 42.56828755692797017 ) ) ;
#2236 = CARTESIAN_POINT ( 'NONE',  ( -35.35872492446279125, 12.59883863067526910, -2.490396854064192755 ) ) ;
#2237 = CARTESIAN_POINT ( 'NONE',  ( 50.24128791297869867, 41.04536285977714982, 5.000000000000000000 ) ) ;
#2238 = CARTESIAN_POINT ( 'NONE',  ( -1.250000000000000222, 0.000000000000000000, 3.333333333333333481 ) ) ;
#2239 = CARTESIAN_POINT ( 'NONE',  ( 168.9999999999999716, -9.999999999999953815, -340.0000000000001137 ) ) ;
#2240 = CARTESIAN_POINT ( 'NONE',  ( 10.69268279052430159, 12.77266927778462779, -2.870787844569587133 ) ) ;
#2241 = DIRECTION ( 'NONE',  ( 0.000000000000000000, 5.664403186863042467E-17, 1.000000000000000000 ) ) ;
#2242 = CARTESIAN_POINT ( 'NONE',  ( -166.6959734468149463, -1.750000000000009992, -159.1817124430720298 ) ) ;
#2243 = FACE_OUTER_BOUND ( 'NONE', #8427, .T. ) ;
#2244 = B_SPLINE_CURVE_WITH_KNOTS ( 'NONE', 3,
 ( #22400, #45715, #45467, #38331 ),
 .UNSPECIFIED., .F., .F.,
 ( 4, 4 ),
 ( 0.000000000000000000, 0.2562577668812812681 ),
 .UNSPECIFIED. ) ;
#2245 = CARTESIAN_POINT ( 'NONE',  ( -5.000000000000000000, 165.2000000000000171, -359.8000000000002387 ) ) ;
#2246 = ORIENTED_EDGE ( 'NONE', *, *, #40382, .T. ) ;
#2247 = DIRECTION ( 'NONE',  ( -0.000000000000000000, -0.000000000000000000, -1.000000000000000000 ) ) ;
#2248 = CARTESIAN_POINT ( 'NONE',  ( -29.61572577327014955, -16.11461842845715253, 8.807470649214879543 ) ) ;
#2249 = CARTESIAN_POINT ( 'NONE',  ( -86.69597344681494633, 1.750000000000009992, -159.1817124430720298 ) ) ;
#2250 = ORIENTED_EDGE ( 'NONE', *, *, #6688, .F. ) ;
#2251 = DIRECTION ( 'NONE',  ( 0.000000000000000000, 4.687818848539279227E-49, -1.000000000000000000 ) ) ;
#2252 = CARTESIAN_POINT ( 'NONE',  ( 358.0000000000000568, 3.000000000000086153, 177.9999999999998295 ) ) ;
#2253 = ORIENTED_EDGE ( 'NONE', *, *, #43738, .T. ) ;
#2254 = DIRECTION ( 'NONE',  ( -1.000000000000000000, -0.000000000000000000, -0.000000000000000000 ) ) ;
#2255 = DIRECTION ( 'NONE',  ( -0.000000000000000000, -0.000000000000000000, -1.000000000000000000 ) ) ;
#2256 = EDGE_CURVE ( 'NONE', #44339, #18412, #42918, .T. ) ;
#2257 = CARTESIAN_POINT ( 'NONE',  ( 8.176860274785711979, -5.756644512789521606, 9.282506307616484875 ) ) ;
#2258 = DIRECTION ( 'NONE',  ( -1.000000000000000000, -0.000000000000000000, -0.000000000000000000 ) ) ;
#2259 = VERTEX_POINT ( 'NONE', #19062 ) ;
#2260 = FACE_OUTER_BOUND ( 'NONE', #4386, .T. ) ;
#2261 = B_SPLINE_SURFACE_WITH_KNOTS ( 'NONE', 3, 3, ( 
 ( #1959, #20698, #12985, #17603 ),
 ( #40712, #28647, #29164, #9653 ),
 ( #5549, #5297, #44277, #33020 ),
 ( #9404, #44780, #45025, #8898 ) ),
 .UNSPECIFIED., .F., .F., .F.,
 ( 4, 4 ),
 ( 4, 4 ),
 ( 0.000000000000000000, 1.000000000000000000 ),
 ( 0.000000000000000000, 1.000000000000000000 ),
 .UNSPECIFIED. ) ;
#2262 = ORIENTED_EDGE ( 'NONE', *, *, #42212, .T. ) ;
#2263 = ORIENTED_EDGE ( 'NONE', *, *, #26257, .F. ) ;
#2264 = CARTESIAN_POINT ( 'NONE',  ( -10.01251772323708700, 8.486842105263161073, 18.46084505325461578 ) ) ;
#2265 = ORIENTED_EDGE ( 'NONE', *, *, #48091, .T. ) ;
#2266 = CARTESIAN_POINT ( 'NONE',  ( -128.4459734468149179, 0.000000000000000000, 39.06828755692801280 ) ) ;
#2267 = CYLINDRICAL_SURFACE ( 'NONE', #3574, 1.750000000000001554 ) ;
#2268 = VERTEX_POINT ( 'NONE', #7796 ) ;
#2269 = LINE ( 'NONE', #21775, #35286 ) ;
#2270 = EDGE_CURVE ( 'NONE', #43944, #27545, #39351, .T. ) ;
#2271 = CARTESIAN_POINT ( 'NONE',  ( -166.6959734468149463, 1.750000000000010658, 80.81828755692798438 ) ) ;
#2272 = DIRECTION ( 'NONE',  ( -7.793956916774524585E-48, 0.000000000000000000, -1.000000000000000000 ) ) ;
#2273 = ORIENTED_EDGE ( 'NONE', *, *, #32773, .F. ) ;
#2274 = DIRECTION ( 'NONE',  ( 0.000000000000000000, -1.000000000000000000, -3.186989995019654210E-49 ) ) ;
#2275 = FACE_OUTER_BOUND ( 'NONE', #44624, .T. ) ;
#2276 = EDGE_CURVE ( 'NONE', #40766, #23064, #38342, .T. ) ;
#2277 = PLANE ( 'NONE',  #41450 ) ;
#2278 = ORIENTED_EDGE ( 'NONE', *, *, #5208, .F. ) ;
#2279 = AXIS2_PLACEMENT_3D ( 'NONE', #44315, #4588, #1254 ) ;
#2280 = LINE ( 'NONE', #48431, #50475 ) ;
#2281 = FACE_BOUND ( 'NONE', #45381, .T. ) ;
#2282 = VERTEX_POINT ( 'NONE', #48738 ) ;
#2283 = ORIENTED_EDGE ( 'NONE', *, *, #31995, .T. ) ;
#2284 = ORIENTED_EDGE ( 'NONE', *, *, #38775, .F. ) ;
#2285 = DIRECTION ( 'NONE',  ( -1.000000000000000000, -0.000000000000000000, -0.000000000000000000 ) ) ;
#2286 = CARTESIAN_POINT ( 'NONE',  ( 168.9999999999999716, -256.5000000000000000, -114.9999999999999574 ) ) ;
#2287 = ADVANCED_FACE ( 'NONE', ( #1839 ), #41087, .T. ) ;
#2288 = VERTEX_POINT ( 'NONE', #44899 ) ;
#2289 = ADVANCED_FACE ( 'NONE', ( #25185 ), #28884, .T. ) ;
#2290 = CARTESIAN_POINT ( 'NONE',  ( -166.6959734468149463, 0.000000000000000000, 165.0000000000000000 ) ) ;
#2291 = CYLINDRICAL_SURFACE ( 'NONE', #32009, 1.750000000000036193 ) ;
#2292 = CARTESIAN_POINT ( 'NONE',  ( 22.69295089195473736, 45.31600496604706052, 7.455576670931136185 ) ) ;
#2293 = ADVANCED_FACE ( 'NONE', ( #48232 ), #25439, .T. ) ;
#2294 = EDGE_CURVE ( 'NONE', #19943, #37516, #21076, .T. ) ;
#2295 = ORIENTED_EDGE ( 'NONE', *, *, #4223, .T. ) ;
#2296 = DIRECTION ( 'NONE',  ( -1.000000000000000000, -0.000000000000000000, -0.000000000000000000 ) ) ;
#2297 = CARTESIAN_POINT ( 'NONE',  ( -164.9459734468149463, 2.143131898507880377E-16, 165.0000000000000000 ) ) ;
#2298 = DIRECTION ( 'NONE',  ( -1.000000000000000000, 4.758098676964957447E-16, 1.586032892321651989E-16 ) ) ;
#2299 = ORIENTED_EDGE ( 'NONE', *, *, #34194, .T. ) ;
#2300 = CONTEXT_DEPENDENT_SHAPE_REPRESENTATION ( #8305, #27841 ) ;
#2301 = CARTESIAN_POINT ( 'NONE',  ( 350.0000000000001137, 169.0000000000000000, 339.9999999999997726 ) ) ;
#2302 = CARTESIAN_POINT ( 'NONE',  ( 1.197382828408165567, -0.5140992728903442943, 9.961922210043278270 ) ) ;
#2303 = CARTESIAN_POINT ( 'NONE',  ( -13.59579750444763668, 10.60877755095910935, 8.727788335465566760 ) ) ;
#2304 = CARTESIAN_POINT ( 'NONE',  ( 0.3862712429686810944, 1.188820645368943607, -3.333333333333333481 ) ) ;
#2305 = ORIENTED_EDGE ( 'NONE', *, *, #1512, .F. ) ;
#2306 = CARTESIAN_POINT ( 'NONE',  ( 350.0000000000000000, 165.0000000000000000, -356.0000000000002274 ) ) ;
#2307 = FACE_OUTER_BOUND ( 'NONE', #7610, .T. ) ;
#2308 = CARTESIAN_POINT ( 'NONE',  ( 168.9999999999999716, -272.4999999999999432, -343.9999999999999432 ) ) ;
#2309 = CARTESIAN_POINT ( 'NONE',  ( -7.576114424932982594, 50.00000000000000711, 7.906207997025717304 ) ) ;
#2310 = EDGE_CURVE ( 'NONE', #49578, #37522, #40337, .T. ) ;
#2311 =( LENGTH_UNIT ( ) NAMED_UNIT ( * ) SI_UNIT ( .MILLI., .METRE. ) );
#2312 = ORIENTED_EDGE ( 'NONE', *, *, #46993, .T. ) ;
#2313 = EDGE_CURVE ( 'NONE', #26016, #29839, #45378, .T. ) ;
#2314 = LINE ( 'NONE', #17954, #23145 ) ;
#2316 = ORIENTED_EDGE ( 'NONE', *, *, #9028, .T. ) ;
#2315 = VECTOR ( 'NONE', #33438, 1000.000000000000000 ) ;
#2317 = ADVANCED_FACE ( 'NONE', ( #37271 ), #33159, .T. ) ;
#2318 = CARTESIAN_POINT ( 'NONE',  ( 210.0000000000000568, 0.000000000000000000, 0.8182875569279768335 ) ) ;
#2319 = ORIENTED_EDGE ( 'NONE', *, *, #36924, .T. ) ;
#2320 = DIRECTION ( 'NONE',  ( 1.000000000000000000, 0.000000000000000000, 0.000000000000000000 ) ) ;
#2321 = EDGE_CURVE ( 'NONE', #13085, #5639, #43096, .T. ) ;
#2322 = CARTESIAN_POINT ( 'NONE',  ( -5.000000000000000000, 184.8000000000000114, 340.1999999999997044 ) ) ;
#2323 = PRESENTATION_STYLE_ASSIGNMENT (( #30046 ) ) ;
#2324 = VERTEX_POINT ( 'NONE', #13376 ) ;
#2325 = ADVANCED_FACE ( 'NONE', ( #28785, #24942 ), #13863, .T. ) ;
#2326 =( BOUNDED_CURVE ( )  B_SPLINE_CURVE ( 3, ( #7322, #10911, #26567, #34798 ),
 .UNSPECIFIED., .F., .F. ) 
 B_SPLINE_CURVE_WITH_KNOTS ( ( 4, 4 ),
 ( 0.000000000000000000, 1.570796326794896558 ),
 .UNSPECIFIED. ) 
 CURVE ( )  GEOMETRIC_REPRESENTATION_ITEM ( )  RATIONAL_B_SPLINE_CURVE ( ( 1.000000000000000000, 0.8047378541243649375, 0.8047378541243649375, 1.000000000000000000 ) ) 
 REPRESENTATION_ITEM ( '' )  );
#2327 = FACE_OUTER_BOUND ( 'NONE', #43838, .T. ) ;
#2328 = ORIENTED_EDGE ( 'NONE', *, *, #11109, .F. ) ;
#2329 = DIRECTION ( 'NONE',  ( -0.000000000000000000, -0.000000000000000000, 1.000000000000000000 ) ) ;
#2330 = LINE ( 'NONE', #17480, #1147 ) ;
#2331 = CARTESIAN_POINT ( 'NONE',  ( 113.3040265531850537, 1.749999999999996891, -159.1817124430720298 ) ) ;
#2332 = CARTESIAN_POINT ( 'NONE',  ( -0.4430828623856294946, -1.527151971571945266, 9.933337059263825708 ) ) ;
#2333 = DIRECTION ( 'NONE',  ( 0.000000000000000000, 0.000000000000000000, 1.000000000000000000 ) ) ;
#2334 = ORIENTED_EDGE ( 'NONE', *, *, #7131, .T. ) ;
#2335 = ORIENTED_EDGE ( 'NONE', *, *, #44178, .F. ) ;
#2336 = CARTESIAN_POINT ( 'NONE',  ( -16.76006782980216059, 2.050259795448645228, 9.178419661560148768 ) ) ;
#2337 = B_SPLINE_CURVE_WITH_KNOTS ( 'NONE', 3,
 ( #12521, #39239, #27679, #36149 ),
 .UNSPECIFIED., .F., .F.,
 ( 4, 4 ),
 ( 0.000000000000000000, 0.2562577668812813791 ),
 .UNSPECIFIED. ) ;
#2338 = ORIENTED_EDGE ( 'NONE', *, *, #25664, .F. ) ;
#2339 = DIRECTION ( 'NONE',  ( -7.793956916774524585E-48, 0.000000000000000000, -1.000000000000000000 ) ) ;
#2340 = ADVANCED_FACE ( 'NONE', ( #45151 ), #6193, .F. ) ;
#2341 = ORIENTED_EDGE ( 'NONE', *, *, #41912, .F. ) ;
#2342 = CARTESIAN_POINT ( 'NONE',  ( 168.9999999999999716, -95.49999999999998579, -350.0000000000001705 ) ) ;
#2343 =( BOUNDED_CURVE ( )  B_SPLINE_CURVE ( 3, ( #23743, #20137, #35827, #12436 ),
 .UNSPECIFIED., .F., .F. ) 
 B_SPLINE_CURVE_WITH_KNOTS ( ( 4, 4 ),
 ( 3.141592653589793116, 4.712388980384689674 ),
 .UNSPECIFIED. ) 
 CURVE ( )  GEOMETRIC_REPRESENTATION_ITEM ( )  RATIONAL_B_SPLINE_CURVE ( ( 1.000000000000000000, 0.8047378541243649375, 0.8047378541243649375, 1.000000000000000000 ) ) 
 REPRESENTATION_ITEM ( '' )  );
#2344 = PLANE ( 'NONE',  #23482 ) ;
#2345 = ORIENTED_EDGE ( 'NONE', *, *, #1694, .F. ) ;
#2346 = EDGE_CURVE ( 'NONE', #29795, #10907, #33649, .T. ) ;
#2347 = CARTESIAN_POINT ( 'NONE',  ( 168.9999999999999716, -174.9999999999999716, -344.0000000000001137 ) ) ;
#2348 = PLANE ( 'NONE',  #18537 ) ;
#2349 = CARTESIAN_POINT ( 'NONE',  ( 155.0540265531850537, 2.143131898507880377E-16, -117.4317124430720725 ) ) ;
#2350 = CARTESIAN_POINT ( 'NONE',  ( -127.7210997126620242, -1.749999999999996669, 159.7931612910809065 ) ) ;
#2351 = CARTESIAN_POINT ( 'NONE',  ( 73.30402655318508209, -1.750000000000009992, -159.1817124430720298 ) ) ;
#2352 = EDGE_CURVE ( 'NONE', #28177, #387, #24089, .T. ) ;
#2354 = ORIENTED_EDGE ( 'NONE', *, *, #33928, .T. ) ;
#2353 = ADVANCED_FACE ( 'NONE', ( #7465 ), #38275, .T. ) ;
#2355 = AXIS2_PLACEMENT_3D ( 'NONE', #30400, #50607, #11660 ) ;
#2356 = ORIENTED_EDGE ( 'NONE', *, *, #31937, .F. ) ;
#2357 = ORIENTED_EDGE ( 'NONE', *, *, #32200, .F. ) ;
#2358 = EDGE_CURVE ( 'NONE', #7036, #16858, #9980, .T. ) ;
#2359 = CARTESIAN_POINT ( 'NONE',  ( -0.3862712429686729343, -1.188820645368946050, -10.00000000000000000 ) ) ;
#2360 = PLANE ( 'NONE',  #30682 ) ;
#2361 = EDGE_CURVE ( 'NONE', #14253, #47520, #3083, .T. ) ;
#2362 = CARTESIAN_POINT ( 'NONE',  ( -4.999999999999948486, -204.9999999999999716, -234.7500000000000000 ) ) ;
#2363 = CLOSED_SHELL ( 'NONE', ( #3342, #14419, #2748, #34512, #34172, #9170, #15477, #49367, #30911, #4283, #29578, #33056, #33074, #22732, #2145, #35939, #19462, #13002 ) ) ;
#2364 = VERTEX_POINT ( 'NONE', #14898 ) ;
#2365 = CARTESIAN_POINT ( 'NONE',  ( 185.0000000000000000, -272.5000000000000000, -98.99999999999874944 ) ) ;
#2366 = ORIENTED_EDGE ( 'NONE', *, *, #34383, .T. ) ;
#2367 =( LENGTH_UNIT ( ) NAMED_UNIT ( * ) SI_UNIT ( .MILLI., .METRE. ) );
#2368 = CARTESIAN_POINT ( 'NONE',  ( 344.0000000000000000, 175.0000000000000284, -90.00000000000018474 ) ) ;
#2369 = DIRECTION ( 'NONE',  ( -2.220446049250312588E-16, -0.7071067811865475727, -0.7071067811865474617 ) ) ;
#2370 = DIRECTION ( 'NONE',  ( -0.000000000000000000, -0.000000000000000000, -1.000000000000000000 ) ) ;
#2371 = DIRECTION ( 'NONE',  ( 0.000000000000000000, 1.000000000000000000, 0.000000000000000000 ) ) ;
#2372 = DIRECTION ( 'NONE',  ( -4.755310728521421461E-16, 0.000000000000000000, -1.000000000000000000 ) ) ;
#2373 = CARTESIAN_POINT ( 'NONE',  ( -114.9999999999981526, 17.00000000000000000, 65.00000000000000000 ) ) ;
#2374 = ORIENTED_EDGE ( 'NONE', *, *, #30806, .F. ) ;
#2375 = B_SPLINE_SURFACE_WITH_KNOTS ( 'NONE', 3, 3, ( 
 ( #29137, #13476, #28881, #8871 ),
 ( #20929, #36614, #5526, #1193 ),
 ( #28620, #20414, #44256, #44501 ),
 ( #39939, #36349, #32236, #33000 ) ),
 .UNSPECIFIED., .F., .F., .F.,
 ( 4, 4 ),
 ( 4, 4 ),
 ( 0.000000000000000000, 1.000000000000000000 ),
 ( 0.000000000000000000, 1.000000000000000000 ),
 .UNSPECIFIED. ) ;
#2376 = CARTESIAN_POINT ( 'NONE',  ( 73.30402655318508209, 1.750000000000009992, -159.1817124430720298 ) ) ;
#2377 = PLANE ( 'NONE',  #19234 ) ;
#2378 = DIRECTION ( 'NONE',  ( 1.000000000000000000, 0.000000000000000000, -1.132880637372608740E-16 ) ) ;
#2379 = ORIENTED_EDGE ( 'NONE', *, *, #11745, .T. ) ;
#2380 = EDGE_CURVE ( 'NONE', #47565, #36849, #41841, .T. ) ;
#2381 = CARTESIAN_POINT ( 'NONE',  ( 168.9999999999999716, 175.0000000000000284, -344.0000000000001137 ) ) ;
#2382 = ORIENTED_EDGE ( 'NONE', *, *, #42487, .T. ) ;
#2383 = CYLINDRICAL_SURFACE ( 'NONE', #27076, 0.5000000000000004441 ) ;
#2384 = LINE ( 'NONE', #29339, #15161 ) ;
#2385 = DIRECTION ( 'NONE',  ( 0.000000000000000000, 0.000000000000000000, 1.000000000000000000 ) ) ;
#2386 = EDGE_LOOP ( 'NONE', ( #42573, #21078, #47318, #22481 ) ) ;
#2387 = CIRCLE ( 'NONE', #17935, 4.000000000000003553 ) ;
#2388 = AXIS2_PLACEMENT_3D ( 'NONE', #2308, #25931, #45386 ) ;
#2389 = CARTESIAN_POINT ( 'NONE',  ( 13.92102703536701114, 30.85732372859822803, 8.356839323120299312 ) ) ;
#2390 = ORIENTED_EDGE ( 'NONE', *, *, #31295, .T. ) ;
#2391 = CARTESIAN_POINT ( 'NONE',  ( 33.30402655318503946, 0.000000000000000000, 165.0000000000000000 ) ) ;
#2392 = DIRECTION ( 'NONE',  ( 0.000000000000000000, -3.186989995019654210E-49, -1.000000000000000000 ) ) ;
#2393 = VECTOR ( 'NONE', #7981, 1000.000000000000000 ) ;
#2394 = CARTESIAN_POINT ( 'NONE',  ( -208.4459734468148611, -1.025126265847089435, -40.93171244307204404 ) ) ;
#2395 = EDGE_CURVE ( 'NONE', #44892, #32574, #23276, .T. ) ;
#2396 = AXIS2_PLACEMENT_3D ( 'NONE', #6923, #46891, #27436 ) ;
#2397 = EDGE_LOOP ( 'NONE', ( #43510, #31402, #50616, #4938 ) ) ;
#2398 = ORIENTED_EDGE ( 'NONE', *, *, #9205, .F. ) ;
#2399 = LINE ( 'NONE', #2159, #50424 ) ;
#2400 = DIRECTION ( 'NONE',  ( -1.000000000000000000, 0.000000000000000000, 0.000000000000000000 ) ) ;
#2401 = EDGE_LOOP ( 'NONE', ( #45203, #22728, #47305, #23767 ) ) ;
#2402 = ORIENTED_EDGE ( 'NONE', *, *, #20620, .T. ) ;
#2403 = CARTESIAN_POINT ( 'NONE',  ( -0.2776613828612424784, 1.251395203515897503, 9.967237415621765351 ) ) ;
#2404 = LINE ( 'NONE', #6504, #16910 ) ;
#2405 = CARTESIAN_POINT ( 'NONE',  ( 85.00000000000029843, 17.00000000000000000, -84.99999999999998579 ) ) ;
#2406 = EDGE_CURVE ( 'NONE', #45654, #13485, #8049, .T. ) ;
#2407 = ORIENTED_EDGE ( 'NONE', *, *, #26303, .T. ) ;
#2408 = LINE ( 'NONE', #34746, #30082 ) ;
#2409 = ORIENTED_EDGE ( 'NONE', *, *, #22387, .F. ) ;
#2410 = CARTESIAN_POINT ( 'NONE',  ( -46.69597344681494633, 0.000000000000000000, 165.0000000000000000 ) ) ;
#2411 = PLANE ( 'NONE',  #25717 ) ;
#2412 = EDGE_CURVE ( 'NONE', #43496, #12984, #18225, .T. ) ;
#2413 = ADVANCED_FACE ( 'NONE', ( #42342 ), #49994, .T. ) ;
#2414 = VERTEX_POINT ( 'NONE', #19238 ) ;
#2415 = ORIENTED_EDGE ( 'NONE', *, *, #42173, .F. ) ;
#2416 = CARTESIAN_POINT ( 'NONE',  ( 85.00000000000029843, 16.00000000000000000, -84.99999999999998579 ) ) ;
#2417 = LINE ( 'NONE', #37094, #7683 ) ;
#2418 = EDGE_CURVE ( 'NONE', #38616, #43903, #6155, .T. ) ;
#2419 = VERTEX_POINT ( 'NONE', #38768 ) ;
#2420 = LINE ( 'NONE', #18066, #10038 ) ;
#2421 = B_SPLINE_CURVE_WITH_KNOTS ( 'NONE', 3,
 ( #9540, #32647, #37520, #21337 ),
 .UNSPECIFIED., .F., .F.,
 ( 4, 4 ),
 ( 5.641302087951259315E-05, 0.0003272669002642556607 ),
 .UNSPECIFIED. ) ;
#2423 = VERTEX_POINT ( 'NONE', #45407 ) ;
#2422 = VECTOR ( 'NONE', #2823, 1000.000000000000000 ) ;
#2424 = EDGE_CURVE ( 'NONE', #26016, #15667, #10789, .T. ) ;
#2425 = PLANE ( 'NONE',  #10262 ) ;
#2427 = ORIENTED_EDGE ( 'NONE', *, *, #18054, .F. ) ;
#2426 = AXIS2_PLACEMENT_3D ( 'NONE', #37433, #21497, #6610 ) ;
#2428 = EDGE_CURVE ( 'NONE', #26536, #46696, #22335, .T. ) ;
#2429 = CARTESIAN_POINT ( 'NONE',  ( 35.00000000000216716, 16.00000000000000000, 115.0000000000000142 ) ) ;
#2430 = CARTESIAN_POINT ( 'NONE',  ( -166.6959734468149463, -1.750000000000010214, -39.18171244307202983 ) ) ;
#2431 = CARTESIAN_POINT ( 'NONE',  ( -0.9598058911017687267, -1.847159827636240426, 9.888808121373918070 ) ) ;
#2432 = DIRECTION ( 'NONE',  ( -0.000000000000000000, -0.000000000000000000, -1.000000000000000000 ) ) ;
#2433 = AXIS2_PLACEMENT_3D ( 'NONE', #14749, #5587, #48149 ) ;
#2434 =( BOUNDED_CURVE ( )  B_SPLINE_CURVE ( 3, ( #20078, #46227, #27017, #43177 ),
 .UNSPECIFIED., .F., .F. ) 
 B_SPLINE_CURVE_WITH_KNOTS ( ( 4, 4 ),
 ( 1.570796326794896558, 3.141592653589793116 ),
 .UNSPECIFIED. ) 
 CURVE ( )  GEOMETRIC_REPRESENTATION_ITEM ( )  RATIONAL_B_SPLINE_CURVE ( ( 1.000000000000000000, 0.8047378541243649375, 0.8047378541243649375, 1.000000000000000000 ) ) 
 REPRESENTATION_ITEM ( '' )  );
#2435 = DIRECTION ( 'NONE',  ( -1.000000000000000000, -0.000000000000000000, -0.000000000000000000 ) ) ;
#2436 = VERTEX_POINT ( 'NONE', #34168 ) ;
#2438 = AXIS2_PLACEMENT_3D ( 'NONE', #35705, #23368, #545 ) ;
#2437 = DIRECTION ( 'NONE',  ( -1.000000000000000000, 0.000000000000000000, 0.000000000000000000 ) ) ;
#2439 = CARTESIAN_POINT ( 'NONE',  ( 0.4548599190037341811, 1.225298710497799703, 9.945465957785110334 ) ) ;
#2440 = ADVANCED_FACE ( 'NONE', ( #14391 ), #6685, .T. ) ;
#2441 = CARTESIAN_POINT ( 'NONE',  ( 72.27890028733797578, 1.750000000000009548, -118.1565861772249519 ) ) ;
#2442 = LINE ( 'NONE', #49831, #6222 ) ;
#2443 = VECTOR ( 'NONE', #28402, 1000.000000000000000 ) ;
#2444 = LINE ( 'NONE', #29144, #11728 ) ;
#2445 = DIRECTION ( 'NONE',  ( -1.000000000000000000, 0.000000000000000000, 0.000000000000000000 ) ) ;
#2446 = CARTESIAN_POINT ( 'NONE',  ( 112.2789002873379758, 1.749999999999997113, 119.7931612910809065 ) ) ;
#2447 = DIRECTION ( 'NONE',  ( -1.000000000000000000, 0.000000000000000000, 0.000000000000000000 ) ) ;
#2448 = DIRECTION ( 'NONE',  ( -0.000000000000000000, 0.000000000000000000, 1.000000000000000000 ) ) ;
#2449 = VERTEX_POINT ( 'NONE', #46150 ) ;
#2450 = LINE ( 'NONE', #29155, #45062 ) ;
#2451 = FACE_OUTER_BOUND ( 'NONE', #397, .T. ) ;
#2452 = CARTESIAN_POINT ( 'NONE',  ( -69.99999999999909051, 17.00000000000000000, 0.000000000000000000 ) ) ;
#2453 = ORIENTED_EDGE ( 'NONE', *, *, #25212, .F. ) ;
#2454 = ORIENTED_EDGE ( 'NONE', *, *, #37265, .T. ) ;
#2455 = AXIS2_PLACEMENT_3D ( 'NONE', #15350, #35622, #7647 ) ;
#2456 = CARTESIAN_POINT ( 'NONE',  ( 115.0540265531850395, 2.143131898507847836E-16, 165.0000000000000000 ) ) ;
#2457 = EDGE_CURVE ( 'NONE', #48255, #46544, #10294, .T. ) ;
#2458 = CARTESIAN_POINT ( 'NONE',  ( 1.780557400379557231, 1.041314823045442095, 9.889206917020299414 ) ) ;
#2459 = VECTOR ( 'NONE', #48852, 1000.000000000000000 ) ;
#2460 = ORIENTED_EDGE ( 'NONE', *, *, #35958, .T. ) ;
#2461 = CARTESIAN_POINT ( 'NONE',  ( -25.61277432017861955, 22.36370378792854297, 7.906207997025717304 ) ) ;
#2462 = FACE_OUTER_BOUND ( 'NONE', #40549, .T. ) ;
#2463 = ORIENTED_EDGE ( 'NONE', *, *, #45939, .T. ) ;
#2464 = ORIENTED_EDGE ( 'NONE', *, *, #7471, .F. ) ;
#2465 = VECTOR ( 'NONE', #10680, 1000.000000000000000 ) ;
#2466 = ORIENTED_EDGE ( 'NONE', *, *, #39946, .F. ) ;
#2467=STYLED_ITEM('',(#50747),#5021);
#2468 = DIRECTION ( 'NONE',  ( -1.000000000000000000, -0.000000000000000000, -0.000000000000000000 ) ) ;
#2469 = PLANE ( 'NONE',  #47155 ) ;
#2470 = DIRECTION ( 'NONE',  ( -1.000000000000000000, 0.000000000000000000, 0.000000000000000000 ) ) ;
#2471 = AXIS2_PLACEMENT_3D ( 'NONE', #7256, #39587, #3909 ) ;
#2472 = VERTEX_POINT ( 'NONE', #37761 ) ;
#2473 = EDGE_CURVE ( 'NONE', #449, #46833, #29413, .T. ) ;
#2474 = CARTESIAN_POINT ( 'NONE',  ( 210.0000000000000568, 0.000000000000000000, 0.8182875569279768335 ) ) ;
#2475 = EDGE_CURVE ( 'NONE', #11215, #9008, #2578, .T. ) ;
#2476 = CARTESIAN_POINT ( 'NONE',  ( 75.05402655318509630, 2.143131898507880377E-16, 82.56828755692799859 ) ) ;
#2477 = CARTESIAN_POINT ( 'NONE',  ( -5.000000000000000000, 184.8000000000000114, -340.2000000000001592 ) ) ;
#2478 = ORIENTED_EDGE ( 'NONE', *, *, #4027, .F. ) ;
#2479 = ORIENTED_EDGE ( 'NONE', *, *, #42053, .F. ) ;
#2480 = CARTESIAN_POINT ( 'NONE',  ( 111.5540265531850679, 0.000000000000000000, -40.93171244307202983 ) ) ;
#2481 = CARTESIAN_POINT ( 'NONE',  ( 38.83576208387757589, 47.08801056904012228, 741.9425600500172777 ) ) ;
#2482 = ORIENTED_EDGE ( 'NONE', *, *, #13416, .F. ) ;
#2483 = EDGE_CURVE ( 'NONE', #43501, #26701, #32077, .T. ) ;
#2484 = FACE_OUTER_BOUND ( 'NONE', #34875, .T. ) ;
#2485 = SURFACE_STYLE_FILL_AREA ( #30970 ) ;
#2486 = EDGE_CURVE ( 'NONE', #29488, #7843, #23607, .T. ) ;
#2487 =( BOUNDED_CURVE ( )  B_SPLINE_CURVE ( 3, ( #46976, #11618, #23920, #38581 ),
 .UNSPECIFIED., .F., .F. ) 
 B_SPLINE_CURVE_WITH_KNOTS ( ( 4, 4 ),
 ( 1.570796326794896558, 3.141592653589793116 ),
 .UNSPECIFIED. ) 
 CURVE ( )  GEOMETRIC_REPRESENTATION_ITEM ( )  RATIONAL_B_SPLINE_CURVE ( ( 1.000000000000000000, 0.8047378541243649375, 0.8047378541243649375, 1.000000000000000000 ) ) 
 REPRESENTATION_ITEM ( '' )  );
#2488 = CARTESIAN_POINT ( 'NONE',  ( 344.0000000000000000, -166.9999999999999716, 341.9999999999998295 ) ) ;
#2489 = CARTESIAN_POINT ( 'NONE',  ( 55.00000000000002132, -52.50000000000000711, 5.000000000000000000 ) ) ;
#2490 = CARTESIAN_POINT ( 'NONE',  ( -1.250000000000000222, 0.000000000000000000, -10.00000000000000000 ) ) ;
#2492 = EDGE_CURVE ( 'NONE', #30746, #40029, #27211, .T. ) ;
#2491 =( NAMED_UNIT ( * ) PLANE_ANGLE_UNIT ( ) SI_UNIT ( $, .RADIAN. ) );
#2493 = CARTESIAN_POINT ( 'NONE',  ( 339.9999999999999432, -169.0000000000001137, -349.9999999999998863 ) ) ;
#2494 =( BOUNDED_CURVE ( )  B_SPLINE_CURVE ( 3, ( #33761, #6547, #22202, #15008 ),
 .UNSPECIFIED., .F., .F. ) 
 B_SPLINE_CURVE_WITH_KNOTS ( ( 4, 4 ),
 ( 1.346561575685802925, 1.570796326794893671 ),
 .UNSPECIFIED. ) 
 CURVE ( )  GEOMETRIC_REPRESENTATION_ITEM ( )  RATIONAL_B_SPLINE_CURVE ( ( 1.000000000000000000, 0.9958142854328209115, 0.9958142854328209115, 1.000000000000000000 ) ) 
 REPRESENTATION_ITEM ( '' )  );
#2495 = CARTESIAN_POINT ( 'NONE',  ( 1.172603113866929725, 0.3455467477709275870, 9.987567862361069970 ) ) ;
#2496 = CIRCLE ( 'NONE', #16462, 2.000000000000001776 ) ;
#2497 = CARTESIAN_POINT ( 'NONE',  ( 50.11058929355270664, -7.578863168071591438, 7.455576670931136185 ) ) ;
#2498 = VECTOR ( 'NONE', #50224, 1000.000000000000000 ) ;
#2499 = DIRECTION ( 'NONE',  ( -0.000000000000000000, -0.000000000000000000, -1.000000000000000000 ) ) ;
#2500 = ORIENTED_EDGE ( 'NONE', *, *, #41569, .F. ) ;
#2501 = VECTOR ( 'NONE', #18867, 1000.000000000000000 ) ;
#2502 = CARTESIAN_POINT ( 'NONE',  ( 168.9999999999999716, -184.9999999999999716, -344.0000000000001137 ) ) ;
#2503 = VECTOR ( 'NONE', #23758, 1000.000000000000000 ) ;
#2504 = DIRECTION ( 'NONE',  ( -0.000000000000000000, -1.000000000000000000, -0.000000000000000000 ) ) ;
#2505 = AXIS2_PLACEMENT_3D ( 'NONE', #5657, #21558, #20802 ) ;
#2506 = CARTESIAN_POINT ( 'NONE',  ( 164.9999999999999716, 17.00000000000000000, 59.99999999999999289 ) ) ;
#2507 = VERTEX_POINT ( 'NONE', #24383 ) ;
#2508 = FACE_OUTER_BOUND ( 'NONE', #19419, .T. ) ;
#2509 = LINE ( 'NONE', #25356, #48276 ) ;
#2510 = ORIENTED_EDGE ( 'NONE', *, *, #26162, .F. ) ;
#2511 = CARTESIAN_POINT ( 'NONE',  ( -44.94597344681493922, 2.143131898507880377E-16, -40.93171244307205825 ) ) ;
#2512 = PLANE ( 'NONE',  #24670 ) ;
#2513 = CARTESIAN_POINT ( 'NONE',  ( -14.99999999999812594, 17.00000000000000000, 65.00000000000000000 ) ) ;
#2514 = CARTESIAN_POINT ( 'NONE',  ( 34.99999999999997868, 17.00000000000000000, -90.00000000000000000 ) ) ;
#2515 = ORIENTED_EDGE ( 'NONE', *, *, #16148, .F. ) ;
#2516 = LINE ( 'NONE', #17163, #37250 ) ;
#2517 = ORIENTED_EDGE ( 'NONE', *, *, #44457, .F. ) ;
#2518 = VERTEX_POINT ( 'NONE', #8734 ) ;
#2519 = EDGE_CURVE ( 'NONE', #29402, #34186, #39530, .T. ) ;
#2520 = CARTESIAN_POINT ( 'NONE',  ( -5.670847180967843570, -1.750000000000023981, -120.2068387089191219 ) ) ;
#2521 = VERTEX_POINT ( 'NONE', #24134 ) ;
#2522 = DIRECTION ( 'NONE',  ( 0.000000000000000000, 0.000000000000000000, -1.000000000000000000 ) ) ;
#2523 = FACE_OUTER_BOUND ( 'NONE', #1862, .T. ) ;
#2524 = CARTESIAN_POINT ( 'NONE',  ( -5.000000000000000000, 0.000000000000000000, 0.000000000000000000 ) ) ;
#2525 = CARTESIAN_POINT ( 'NONE',  ( 73.30402655318508209, -1.750000000000009992, 0.8182875569279768335 ) ) ;
#2526 = CARTESIAN_POINT ( 'NONE',  ( 31.55402655318503236, 1.025126265847088991, 2.568287556927986159 ) ) ;
#2527 = VERTEX_POINT ( 'NONE', #15916 ) ;
#2528 = FACE_OUTER_BOUND ( 'NONE', #1334, .T. ) ;
#2529 = CIRCLE ( 'NONE', #36175, 4.000000000000003553 ) ;
#2530 = DIRECTION ( 'NONE',  ( -0.000000000000000000, -0.000000000000000000, -1.000000000000000000 ) ) ;
#2531 = DIRECTION ( 'NONE',  ( -1.000000000000000000, -0.000000000000000000, -0.000000000000000000 ) ) ;
#2532 = ORIENTED_EDGE ( 'NONE', *, *, #20272, .T. ) ;
#2533 = CARTESIAN_POINT ( 'NONE',  ( -8.813458710706198573, -4.724716452304520864, 0.000000000000000000 ) ) ;
#2534 = CARTESIAN_POINT ( 'NONE',  ( 153.3040265531850537, 1.750000000000010658, -119.1817124430720440 ) ) ;
#2535 = EDGE_LOOP ( 'NONE', ( #31786, #44451, #48293, #20274, #5994, #14410 ) ) ;
#2536 = ORIENTED_EDGE ( 'NONE', *, *, #50341, .F. ) ;
#2537 = ORIENTED_EDGE ( 'NONE', *, *, #31216, .T. ) ;
#2538 = CARTESIAN_POINT ( 'NONE',  ( 191.5540265531851105, 0.000000000000000000, 165.0000000000000000 ) ) ;
#2539 = CARTESIAN_POINT ( 'NONE',  ( 33.30402655318503946, 0.000000000000000000, 165.0000000000000000 ) ) ;
#2540 = AXIS2_PLACEMENT_3D ( 'NONE', #23259, #35857, #19920 ) ;
#2541 = VERTEX_POINT ( 'NONE', #42839 ) ;
#2542 = DIRECTION ( 'NONE',  ( -0.000000000000000000, -0.000000000000000000, -1.000000000000000000 ) ) ;
#2543 = CARTESIAN_POINT ( 'NONE',  ( -86.69597344681494633, -1.750000000000010658, 80.81828755692798438 ) ) ;
#2544 = FACE_BOUND ( 'NONE', #50410, .T. ) ;
#2545 = CYLINDRICAL_SURFACE ( 'NONE', #3046, 3.749999999999975575 ) ;
#2546 = ORIENTED_EDGE ( 'NONE', *, *, #32505, .T. ) ;
#2547 = CARTESIAN_POINT ( 'NONE',  ( -14.99999999999782041, 16.00000000000000000, 95.00000000000000000 ) ) ;
#2548 = ADVANCED_FACE ( 'NONE', ( #4623 ), #20009, .T. ) ;
#2549 = CARTESIAN_POINT ( 'NONE',  ( 210.0000000000000568, 0.000000000000000000, 42.56828755692799149 ) ) ;
#2550 = B_SPLINE_CURVE_WITH_KNOTS ( 'NONE', 3,
 ( #46621, #11008, #50466, #15374 ),
 .UNSPECIFIED., .F., .F.,
 ( 4, 4 ),
 ( 1.760159736610854221E-18, 0.0009539133080775338879 ),
 .UNSPECIFIED. ) ;
#2551 = VERTEX_POINT ( 'NONE', #20268 ) ;
#2552 = LINE ( 'NONE', #14358, #38851 ) ;
#2553 = LINE ( 'NONE', #37983, #38904 ) ;
#2554 = CARTESIAN_POINT ( 'NONE',  ( -1.011271242968683426, -0.7347315653655928092, -10.00000000000000000 ) ) ;
#2555 = CARTESIAN_POINT ( 'NONE',  ( -0.2773062244624664441, 1.251557370488897813, 9.948547179989621014 ) ) ;
#2556 = ORIENTED_EDGE ( 'NONE', *, *, #807, .F. ) ;
#2557 = CARTESIAN_POINT ( 'NONE',  ( 168.9999999999999716, -164.9999999999999432, -342.0000000000001137 ) ) ;
#2558 = DIRECTION ( 'NONE',  ( 0.000000000000000000, 0.000000000000000000, 1.000000000000000000 ) ) ;
#2559 = CARTESIAN_POINT ( 'NONE',  ( -44.94597344681493922, 1.025126265847089435, -157.4317124430720582 ) ) ;
#2560 = CARTESIAN_POINT ( 'NONE',  ( 183.0000000000000000, -268.4999999999999432, -349.9999999999999432 ) ) ;
#2561 = AXIS2_PLACEMENT_3D ( 'NONE', #36529, #1367, #20344 ) ;
#2562 = ORIENTED_EDGE ( 'NONE', *, *, #16697, .T. ) ;
#2563 = CARTESIAN_POINT ( 'NONE',  ( -48.44597344681496054, -1.025126265847089879, 122.5682875569280128 ) ) ;
#2564 = ORIENTED_EDGE ( 'NONE', *, *, #49638, .F. ) ;
#2565 = CARTESIAN_POINT ( 'NONE',  ( 1.250000000000000222, 0.000000000000000000, 10.00000000000000000 ) ) ;
#2566 = VERTEX_POINT ( 'NONE', #39026 ) ;
#2567 = CARTESIAN_POINT ( 'NONE',  ( 1.258633725701695294, -0.04081300982073039069, 9.974012008644017158 ) ) ;
#2568 = VECTOR ( 'NONE', #24294, 1000.000000000000000 ) ;
#2569 = DIRECTION ( 'NONE',  ( -1.000000000000000000, -0.000000000000000000, -0.000000000000000000 ) ) ;
#2570 = AXIS2_PLACEMENT_3D ( 'NONE', #20119, #8583, #24239 ) ;
#2571 = EDGE_LOOP ( 'NONE', ( #46749, #13467, #29657, #17898, #34645, #15068 ) ) ;
#2572 = CARTESIAN_POINT ( 'NONE',  ( -18.38319608353667434, 32.68498281710182596, -8.192531242611268638 ) ) ;
#2573 = ORIENTED_EDGE ( 'NONE', *, *, #11718, .F. ) ;
#2574 = LINE ( 'NONE', #10289, #3246 ) ;
#2575 = CARTESIAN_POINT ( 'NONE',  ( 135.0000000000012790, 17.00000000000000000, 30.00000000000000000 ) ) ;
#2576 = CARTESIAN_POINT ( 'NONE',  ( -34.95136153415531766, 36.40974830873496870, 8.356839323120299312 ) ) ;
#2577 = LINE ( 'NONE', #18223, #6215 ) ;
#2578 = LINE ( 'NONE', #35436, #32315 ) ;
#2579 = ORIENTED_EDGE ( 'NONE', *, *, #19259, .T. ) ;
#2580 = EDGE_LOOP ( 'NONE', ( #21869, #13993, #23994, #18416 ) ) ;
#2581 = DIRECTION ( 'NONE',  ( 1.000000000000000000, -0.000000000000000000, -0.000000000000000000 ) ) ;
#2582 = ORIENTED_EDGE ( 'NONE', *, *, #14692, .T. ) ;
#2583 = CARTESIAN_POINT ( 'NONE',  ( -164.4973046169135955, 53.53801056904005407, -18.45589678844777382 ) ) ;
#2584 = CARTESIAN_POINT ( 'NONE',  ( 0.000000000000000000, 169.0000000000000000, -340.0000000000001705 ) ) ;
#2585 = ORIENTED_EDGE ( 'NONE', *, *, #25789, .T. ) ;
#2586 = LINE ( 'NONE', #41347, #40139 ) ;
#2587 = CIRCLE ( 'NONE', #50049, 6.000000000000000888 ) ;
#2588 = LINE ( 'NONE', #49506, #26736 ) ;
#2589 = ORIENTED_EDGE ( 'NONE', *, *, #525, .T. ) ;
#2590 = CYLINDRICAL_SURFACE ( 'NONE', #2970, 4.000000000000003553 ) ;
#2591 = CARTESIAN_POINT ( 'NONE',  ( 31.55402655318503236, 0.000000000000000000, -165.0000000000000000 ) ) ;
#2592 = CARTESIAN_POINT ( 'NONE',  ( -4.997592503980432532, -3.246827225423192687, 1.992221491942114397E-15 ) ) ;
#2593 = CARTESIAN_POINT ( 'NONE',  ( 155.0540265531850537, 2.143131898507880377E-16, 79.06828755692797017 ) ) ;
#2594 = EDGE_CURVE ( 'NONE', #30805, #19380, #4112, .T. ) ;
#2595 = AXIS2_PLACEMENT_3D ( 'NONE', #29831, #45444, #49528 ) ;
#2596 = ORIENTED_EDGE ( 'NONE', *, *, #44123, .T. ) ;
#2597 = LINE ( 'NONE', #7737, #5617 ) ;
#2599 = ADVANCED_FACE ( 'NONE', ( #8478 ), #16173, .F. ) ;
#2598 = CARTESIAN_POINT ( 'NONE',  ( 15.45175104485250728, -6.222373774239001065, -2.870787844569587133 ) ) ;
#2600 = CARTESIAN_POINT ( 'NONE',  ( 183.0000000000000284, -174.9999999999999716, -111.0000000000001563 ) ) ;
#2601 = VERTEX_POINT ( 'NONE', #27716 ) ;
#2602 = EDGE_CURVE ( 'NONE', #3325, #48435, #48297, .T. ) ;
#2603 = LINE ( 'NONE', #50203, #34893 ) ;
#2604 = ORIENTED_EDGE ( 'NONE', *, *, #16925, .T. ) ;
#2605 = ADVANCED_FACE ( 'NONE', ( #535 ), #28227, .T. ) ;
#2606 = FACE_OUTER_BOUND ( 'NONE', #42301, .T. ) ;
#2607 = PLANE ( 'NONE',  #17875 ) ;
#2608 = LINE ( 'NONE', #33933, #3718 ) ;
#2609 = DIRECTION ( 'NONE',  ( 0.000000000000000000, 0.000000000000000000, 1.000000000000000000 ) ) ;
#2610 = DIRECTION ( 'NONE',  ( -1.586032892321651989E-16, 8.666415220619855873E-32, -1.000000000000000000 ) ) ;
#2611 = CARTESIAN_POINT ( 'NONE',  ( 4.204997580903516941, -7.388441598285492518, 229.0000000000000000 ) ) ;
#2612 = ORIENTED_EDGE ( 'NONE', *, *, #49052, .T. ) ;
#2613 = FACE_OUTER_BOUND ( 'NONE', #2220, .T. ) ;
#2614 = EDGE_CURVE ( 'NONE', #34400, #46777, #40033, .T. ) ;
#2615 = CARTESIAN_POINT ( 'NONE',  ( -5.000000000000000000, 175.0000000000000284, 350.0000000000002274 ) ) ;
#2616 = DIRECTION ( 'NONE',  ( 0.000000000000000000, -1.000000000000000000, -3.186989995019654210E-49 ) ) ;
#2617 =( BOUNDED_CURVE ( )  B_SPLINE_CURVE ( 3, ( #23273, #18914, #15346, #27653 ),
 .UNSPECIFIED., .F., .F. ) 
 B_SPLINE_CURVE_WITH_KNOTS ( ( 4, 4 ),
 ( 0.000000000000000000, 1.570796326794896558 ),
 .UNSPECIFIED. ) 
 CURVE ( )  GEOMETRIC_REPRESENTATION_ITEM ( )  RATIONAL_B_SPLINE_CURVE ( ( 1.000000000000000000, 0.8047378541243649375, 0.8047378541243649375, 1.000000000000000000 ) ) 
 REPRESENTATION_ITEM ( '' )  );
#2618 = CARTESIAN_POINT ( 'NONE',  ( 49.67735855322978011, -8.912210285361751971, 8.356839323120299312 ) ) ;
#2619 = ORIENTED_EDGE ( 'NONE', *, *, #19864, .F. ) ;
#2620 = DIRECTION ( 'NONE',  ( 1.000000000000000000, 0.000000000000000000, -0.000000000000000000 ) ) ;
#2621 = ORIENTED_EDGE ( 'NONE', *, *, #16201, .F. ) ;
#2622 = FACE_OUTER_BOUND ( 'NONE', #44189, .T. ) ;
#2623 =( BOUNDED_CURVE ( )  B_SPLINE_CURVE ( 3, ( #29682, #44808, #40985, #26348 ),
 .UNSPECIFIED., .F., .F. ) 
 B_SPLINE_CURVE_WITH_KNOTS ( ( 4, 4 ),
 ( 1.570796326794896558, 3.141592653589793116 ),
 .UNSPECIFIED. ) 
 CURVE ( )  GEOMETRIC_REPRESENTATION_ITEM ( )  RATIONAL_B_SPLINE_CURVE ( ( 1.000000000000000000, 0.8047378541243649375, 0.8047378541243649375, 1.000000000000000000 ) ) 
 REPRESENTATION_ITEM ( '' )  );
#2624 = CIRCLE ( 'NONE', #18996, 3.749999999999975575 ) ;
#2625 = CARTESIAN_POINT ( 'NONE',  ( 1.040834085586084257E-14, -6.912230148066169200, -5.000000000000000000 ) ) ;
#2626 = EDGE_CURVE ( 'NONE', #41151, #33474, #47825, .T. ) ;
#2627 = DIRECTION ( 'NONE',  ( 0.000000000000000000, 0.000000000000000000, -1.000000000000000000 ) ) ;
#2628 = ADVANCED_FACE ( 'NONE', ( #7973 ), #4854, .T. ) ;
#2629 = VERTEX_POINT ( 'NONE', #3853 ) ;
#2630 = AXIS2_PLACEMENT_3D ( 'NONE', #12172, #28324, #12413 ) ;
#2631 = EDGE_CURVE ( 'NONE', #31059, #39414, #19493, .T. ) ;
#2632 = EDGE_CURVE ( 'NONE', #14525, #387, #13267, .T. ) ;
#2633 = VECTOR ( 'NONE', #24633, 1000.000000000000000 ) ;
#2634 = CARTESIAN_POINT ( 'NONE',  ( -177.4999999999999716, -112.5000000000000000, -9.999999999999973355 ) ) ;
#2635 = ORIENTED_EDGE ( 'NONE', *, *, #20465, .F. ) ;
#2636 = CARTESIAN_POINT ( 'NONE',  ( -164.9999999999984936, 17.00000000000000000, 35.00000000000000000 ) ) ;
#2637 = CARTESIAN_POINT ( 'NONE',  ( 350.0000000000001137, 181.0000000000000284, 359.9999999999997726 ) ) ;
#2638 = EDGE_CURVE ( 'NONE', #11949, #7818, #19759, .T. ) ;
#2639 = DIRECTION ( 'NONE',  ( 1.000000000000000000, 0.000000000000000000, 0.000000000000000000 ) ) ;
#2640 = EDGE_CURVE ( 'NONE', #12164, #16324, #41029, .T. ) ;
#2641 =( BOUNDED_CURVE ( )  B_SPLINE_CURVE ( 3, ( #33806, #3231, #33554, #22245 ),
 .UNSPECIFIED., .F., .F. ) 
 B_SPLINE_CURVE_WITH_KNOTS ( ( 4, 4 ),
 ( 3.141592653589793116, 4.712388980384689674 ),
 .UNSPECIFIED. ) 
 CURVE ( )  GEOMETRIC_REPRESENTATION_ITEM ( )  RATIONAL_B_SPLINE_CURVE ( ( 1.000000000000000000, 0.8047378541243649375, 0.8047378541243649375, 1.000000000000000000 ) ) 
 REPRESENTATION_ITEM ( '' )  );
#2642 = ORIENTED_EDGE ( 'NONE', *, *, #28141, .F. ) ;
#2643 = ORIENTED_EDGE ( 'NONE', *, *, #15632, .F. ) ;
#2644 = CARTESIAN_POINT ( 'NONE',  ( -3.087186397306470820, -2.514307945609864259, -2.642742795433417058E-16 ) ) ;
#2645 = LINE ( 'NONE', #45212, #940 ) ;
#2646 = EDGE_LOOP ( 'NONE', ( #14887, #27881, #28355, #15359 ) ) ;
#2647 = EDGE_LOOP ( 'NONE', ( #8365, #19298, #46418, #20713, #36956, #22631 ) ) ;
#2648 = CARTESIAN_POINT ( 'NONE',  ( 185.0000000000000000, -256.4999999999999432, -349.9999999999999432 ) ) ;
#2649 = DIRECTION ( 'NONE',  ( 0.000000000000000000, -0.000000000000000000, 1.000000000000000000 ) ) ;
#2650 = FACE_BOUND ( 'NONE', #33391, .T. ) ;
#2651 = ORIENTED_EDGE ( 'NONE', *, *, #19532, .T. ) ;
#2652 = FACE_OUTER_BOUND ( 'NONE', #21506, .T. ) ;
#2653 = EDGE_LOOP ( 'NONE', ( #13262, #17292, #31530 ) ) ;
#2654 = VECTOR ( 'NONE', #49924, 1000.000000000000000 ) ;
#2655 = EDGE_CURVE ( 'NONE', #15017, #11842, #1531, .T. ) ;
#2656 = CARTESIAN_POINT ( 'NONE',  ( -166.6959734468149463, 1.750000000000010658, -79.18171244307201562 ) ) ;
#2657 = CYLINDRICAL_SURFACE ( 'NONE', #42104, 1.750000000000010214 ) ;
#2658 = EDGE_CURVE ( 'NONE', #50662, #36948, #19601, .T. ) ;
#2659 = EDGE_CURVE ( 'NONE', #9213, #50130, #13564, .T. ) ;
#2660 = ORIENTED_EDGE ( 'NONE', *, *, #18732, .T. ) ;
#2661 = VECTOR ( 'NONE', #35085, 1000.000000000000000 ) ;
#2662 = ORIENTED_EDGE ( 'NONE', *, *, #17111, .T. ) ;
#2663 = FACE_OUTER_BOUND ( 'NONE', #13509, .T. ) ;
#2664 = VECTOR ( 'NONE', #47949, 1000.000000000000000 ) ;
#2665 = CARTESIAN_POINT ( 'NONE',  ( -46.69597344681494633, -1.750000000000010214, 40.81828755692798438 ) ) ;
#2666 = EDGE_LOOP ( 'NONE', ( #26311, #43649, #8617, #21048 ) ) ;
#2667 = DIRECTION ( 'NONE',  ( 0.000000000000000000, 0.000000000000000000, -1.000000000000000000 ) ) ;
#2668 = ORIENTED_EDGE ( 'NONE', *, *, #23201, .T. ) ;
#2669 = VECTOR ( 'NONE', #32314, 1000.000000000000000 ) ;
#2670 = EDGE_CURVE ( 'NONE', #17128, #13622, #41268, .T. ) ;
#2671 = DIRECTION ( 'NONE',  ( -0.000000000000000000, -0.000000000000000000, -1.000000000000000000 ) ) ;
#2672 = CARTESIAN_POINT ( 'NONE',  ( -2.538055338523173443, -50.00000000000000000, -9.367992836599951190 ) ) ;
#2673 = ORIENTED_EDGE ( 'NONE', *, *, #6086, .T. ) ;
#2674 = DIRECTION ( 'NONE',  ( 1.000000000000000000, 0.000000000000000000, 1.612977847700450206E-50 ) ) ;
#2675 = LINE ( 'NONE', #33995, #41584 ) ;
#2676 = CARTESIAN_POINT ( 'NONE',  ( -168.4459734468149463, 0.000000000000000000, 165.0000000000000000 ) ) ;
#2677 = VECTOR ( 'NONE', #42373, 1000.000000000000000 ) ;
#2678 = CARTESIAN_POINT ( 'NONE',  ( -164.9459734468149463, -1.025126265847089657, 79.06828755692797017 ) ) ;
#2679 = ORIENTED_EDGE ( 'NONE', *, *, #28748, .T. ) ;
#2680 = DIRECTION ( 'NONE',  ( 0.000000000000000000, 1.000000000000000000, 6.123233995736766036E-17 ) ) ;
#2681 = CARTESIAN_POINT ( 'NONE',  ( 33.89193117067290473, 0.000000000000000000, 910.0000000000000000 ) ) ;
#2682 = B_SPLINE_SURFACE_WITH_KNOTS ( 'NONE', 3, 3, ( 
 ( #24200, #27786, #15726, #11369 ),
 ( #11888, #27546, #7794, #8294 ),
 ( #23933, #39862, #39597, #35768 ),
 ( #42660, #7534, #23169, #19320 ) ),
 .UNSPECIFIED., .F., .F., .F.,
 ( 4, 4 ),
 ( 4, 4 ),
 ( 0.000000000000000000, 1.000000000000000000 ),
 ( 0.000000000000000000, 1.000000000000000000 ),
 .UNSPECIFIED. ) ;
#2683 = DIRECTION ( 'NONE',  ( 1.000000000000000000, 0.000000000000000000, -4.758098676964956461E-16 ) ) ;
#2684 = CARTESIAN_POINT ( 'NONE',  ( -46.11867747200562917, 19.86470446310265103, -8.016098858316199838 ) ) ;
#2685 = ADVANCED_FACE ( 'NONE', ( #17173 ), #48921, .T. ) ;
#2686 = CYLINDRICAL_SURFACE ( 'NONE', #23111, 1.750000000000008438 ) ;
#2687 = CARTESIAN_POINT ( 'NONE',  ( 71.55402655318505367, 0.000000000000000000, 122.5682875569279844 ) ) ;
#2688 = ADVANCED_FACE ( 'NONE', ( #5872 ), #6127, .T. ) ;
#2689 = DIRECTION ( 'NONE',  ( 0.000000000000000000, -1.000000000000000000, 0.000000000000000000 ) ) ;
#2690 = CARTESIAN_POINT ( 'NONE',  ( 166.9999999999999716, -93.49999999999998579, -350.0000000000001705 ) ) ;
#2691 = ORIENTED_EDGE ( 'NONE', *, *, #7899, .F. ) ;
#2692 = ADVANCED_FACE ( 'NONE', ( #36959 ), #36444, .T. ) ;
#2693 = EDGE_CURVE ( 'NONE', #25153, #19185, #16663, .T. ) ;
#2694 = CARTESIAN_POINT ( 'NONE',  ( -45.64490844644706868, -21.32281559348764333, 8.807470649214879543 ) ) ;
#2695 = CARTESIAN_POINT ( 'NONE',  ( -14.48769039275601145, -30.44468701195584970, 8.807470649214879543 ) ) ;
#2696 = CARTESIAN_POINT ( 'NONE',  ( 341.9999999999999432, -169.0000000000001137, -344.0000000000002842 ) ) ;
#2697 = CARTESIAN_POINT ( 'NONE',  ( -9.999999999999994671, -46.01315789473684248, -5.916985404131814619 ) ) ;
#2698 = VECTOR ( 'NONE', #10503, 1000.000000000000000 ) ;
#2699 = ADVANCED_FACE ( 'NONE', ( #44347 ), #2028, .T. ) ;
#2700 = EDGE_LOOP ( 'NONE', ( #11883, #13664, #45812 ) ) ;
#2701 = VERTEX_POINT ( 'NONE', #21776 ) ;
#2702 = CARTESIAN_POINT ( 'NONE',  ( -0.6595498452743703277, 16.59563386392009576, 3.266473740018926541 ) ) ;
#2703 = AXIS2_PLACEMENT_3D ( 'NONE', #27519, #26312, #46017 ) ;
#2704 = EDGE_CURVE ( 'NONE', #4734, #34716, #37453, .T. ) ;
#2705 = CARTESIAN_POINT ( 'NONE',  ( 181.0000000000000000, -164.9999999999999432, 355.9999999999998863 ) ) ;
#2706 = ADVANCED_FACE ( 'NONE', ( #28726 ), #44099, .F. ) ;
#2707 = EDGE_LOOP ( 'NONE', ( #7508, #36482, #24854, #40175 ) ) ;
#2708 = AXIS2_PLACEMENT_3D ( 'NONE', #11786, #7946, #23582 ) ;
#2709 = CARTESIAN_POINT ( 'NONE',  ( 8.277096487746778308, -50.00000000000000711, 7.455576670931136185 ) ) ;
#2710 = DIRECTION ( 'NONE',  ( -0.000000000000000000, 0.000000000000000000, -1.000000000000000000 ) ) ;
#2711 = EDGE_LOOP ( 'NONE', ( #23565, #14957, #15394, #19348 ) ) ;
#2712 = ORIENTED_EDGE ( 'NONE', *, *, #6473, .F. ) ;
#2713 = VERTEX_POINT ( 'NONE', #32588 ) ;
#2714 = DIRECTION ( 'NONE',  ( 0.000000000000000000, 0.000000000000000000, 1.000000000000000000 ) ) ;
#2715 = CARTESIAN_POINT ( 'NONE',  ( -125.6708471809678542, -1.749999999999996669, -160.2068387089191219 ) ) ;
#2716 = CARTESIAN_POINT ( 'NONE',  ( 210.0000000000000568, 0.000000000000000000, -159.1817124430720298 ) ) ;
#2717 = ORIENTED_EDGE ( 'NONE', *, *, #18899, .T. ) ;
#2718 = CARTESIAN_POINT ( 'NONE',  ( -42.78107912161479476, 16.56908454419426135, -9.367992836599951190 ) ) ;
#2719 = EDGE_CURVE ( 'NONE', #22911, #25388, #32841, .T. ) ;
#2720 = LINE ( 'NONE', #33034, #22236 ) ;
#2721 = CARTESIAN_POINT ( 'NONE',  ( 0.000000000000000000, -164.9999999999999432, -356.0000000000002274 ) ) ;
#2722 = ORIENTED_EDGE ( 'NONE', *, *, #2924, .T. ) ;
#2723 =( BOUNDED_CURVE ( )  B_SPLINE_CURVE ( 3, ( #20348, #32663, #48259, #24213 ),
 .UNSPECIFIED., .F., .F. ) 
 B_SPLINE_CURVE_WITH_KNOTS ( ( 4, 4 ),
 ( 4.712388980384682569, 6.283185307179586232 ),
 .UNSPECIFIED. ) 
 CURVE ( )  GEOMETRIC_REPRESENTATION_ITEM ( )  RATIONAL_B_SPLINE_CURVE ( ( 1.000000000000000000, 0.8047378541243632721, 0.8047378541243632721, 1.000000000000000000 ) ) 
 REPRESENTATION_ITEM ( '' )  );
#2724 = ORIENTED_EDGE ( 'NONE', *, *, #34275, .F. ) ;
#2725 = CARTESIAN_POINT ( 'NONE',  ( 210.0000000000000568, 0.000000000000000000, 122.5682875569279844 ) ) ;
#2726 = DIRECTION ( 'NONE',  ( -1.000000000000000000, 0.000000000000000000, 0.000000000000000000 ) ) ;
#2727 = LINE ( 'NONE', #2974, #10291 ) ;
#2728 = ORIENTED_EDGE ( 'NONE', *, *, #167, .F. ) ;
#2729 = CARTESIAN_POINT ( 'NONE',  ( -208.4459734468149463, 0.000000000000000000, -0.9317124430720247208 ) ) ;
#2730 = CYLINDRICAL_SURFACE ( 'NONE', #5117, 50.00000000000000000 ) ;
#2731 = DIRECTION ( 'NONE',  ( -1.000000000000000000, -0.000000000000000000, -0.000000000000000000 ) ) ;
#2732 = CYLINDRICAL_SURFACE ( 'NONE', #43327, 1.750000000000001554 ) ;
#2733 = AXIS2_PLACEMENT_3D ( 'NONE', #43344, #47167, #770 ) ;
#2734 = CARTESIAN_POINT ( 'NONE',  ( -1.250000000000000222, 0.000000000000000000, -3.333333333333333481 ) ) ;
#2735 = EDGE_LOOP ( 'NONE', ( #31824, #12828, #119, #35228 ) ) ;
#2736 = PLANE ( 'NONE',  #28390 ) ;
#2737 = AXIS2_PLACEMENT_3D ( 'NONE', #21421, #29632, #11155 ) ;
#2738 = CARTESIAN_POINT ( 'NONE',  ( -210.0000000000000568, 0.000000000000000000, 80.81828755692798438 ) ) ;
#2739 = DIRECTION ( 'NONE',  ( -0.000000000000000000, 1.000000000000000000, -1.604368532695312981E-16 ) ) ;
#2740 = FACE_OUTER_BOUND ( 'NONE', #48298, .T. ) ;
#2741 = COLOUR_RGB ( '',0.7921568627450980005, 0.8196078431372548767, 0.9333333333333333481 ) ;
#2742 = DIRECTION ( 'NONE',  ( -0.9770330068457271366, 0.000000000000000000, -0.2130880182788259247 ) ) ;
#2743 = ORIENTED_EDGE ( 'NONE', *, *, #40149, .T. ) ;
#2744 = CARTESIAN_POINT ( 'NONE',  ( 151.5540265531850537, 0.000000000000000000, 165.0000000000000000 ) ) ;
#2745 = DIRECTION ( 'NONE',  ( 0.000000000000000000, 0.000000000000000000, 1.000000000000000000 ) ) ;
#2746 = DIRECTION ( 'NONE',  ( -1.586032892321652236E-16, -1.000000000000000000, -6.853681917100419162E-49 ) ) ;
#2747 = VERTEX_POINT ( 'NONE', #25379 ) ;
#2748 = ADVANCED_FACE ( 'NONE', ( #37209 ), #24628, .T. ) ;
#2749 = ADVANCED_FACE ( 'NONE', ( #33846 ), #42028, .T. ) ;
#2750 = CARTESIAN_POINT ( 'NONE',  ( 181.0000000000000000, -252.5000000000000000, -114.9999999999999716 ) ) ;
#2751 = ORIENTED_EDGE ( 'NONE', *, *, #10925, .T. ) ;
#2752 = DIRECTION ( 'NONE',  ( 0.000000000000000000, 0.000000000000000000, 1.000000000000000000 ) ) ;
#2753 = CARTESIAN_POINT ( 'NONE',  ( -14.99999999999782041, 17.00000000000000000, 95.00000000000000000 ) ) ;
#2754 = CARTESIAN_POINT ( 'NONE',  ( 32.27890028733795447, 1.750000000000009548, -38.15658617722494483 ) ) ;
#2755 = CARTESIAN_POINT ( 'NONE',  ( 0.000000000000000000, -165.1999999999999602, -359.8000000000002387 ) ) ;
#2756 = ADVANCED_FACE ( 'NONE', ( #39154 ), #45603, .F. ) ;
#2757 = ORIENTED_EDGE ( 'NONE', *, *, #36900, .F. ) ;
#2758 = CARTESIAN_POINT ( 'NONE',  ( -24.39427009666018265, -44.07992421011638129, 8.807470649214879543 ) ) ;
#2759 = ORIENTED_EDGE ( 'NONE', *, *, #28887, .F. ) ;
#2760 = ORIENTED_EDGE ( 'NONE', *, *, #21930, .F. ) ;
#2761 = EDGE_CURVE ( 'NONE', #42454, #20304, #29988, .T. ) ;
#2762 = CARTESIAN_POINT ( 'NONE',  ( -19.99999999999846523, 17.00000000000000000, 60.00000000000000000 ) ) ;
#2763 = ADVANCED_FACE ( 'NONE', ( #14066 ), #30231, .T. ) ;
#2764 = ORIENTED_EDGE ( 'NONE', *, *, #43668, .T. ) ;
#2766 = VECTOR ( 'NONE', #1025, 1000.000000000000000 ) ;
#2765 = FACE_OUTER_BOUND ( 'NONE', #28, .T. ) ;
#2767 = CARTESIAN_POINT ( 'NONE',  ( -46.76852358249002606, 17.86468378716741512, -9.367992836599954742 ) ) ;
#2768 = VECTOR ( 'NONE', #30748, 1000.000000000000000 ) ;
#2769 = DIRECTION ( 'NONE',  ( 0.4436251537532894806, 0.000000000000000000, -0.8962124318248270161 ) ) ;
#2770 = AXIS2_PLACEMENT_3D ( 'NONE', #14804, #37669, #2742 ) ;
#2771 = EDGE_CURVE ( 'NONE', #35393, #42459, #37875, .T. ) ;
#2772 = DIRECTION ( 'NONE',  ( 0.000000000000000000, -2.969158215481698263E-48, 1.000000000000000000 ) ) ;
#2773 = ORIENTED_EDGE ( 'NONE', *, *, #2346, .F. ) ;
#2774 = CARTESIAN_POINT ( 'NONE',  ( 181.0000000000000000, -164.9999999999999432, -356.0000000000001705 ) ) ;
#2775 = LINE ( 'NONE', #31012, #29883 ) ;
#2776 = AXIS2_PLACEMENT_3D ( 'NONE', #47639, #12527, #28690 ) ;
#2777 = DIRECTION ( 'NONE',  ( -1.000000000000000000, -0.000000000000000000, -0.000000000000000000 ) ) ;
#2778 =( BOUNDED_CURVE ( )  B_SPLINE_CURVE ( 3, ( #2525, #18166, #49434, #14321 ),
 .UNSPECIFIED., .F., .F. ) 
 B_SPLINE_CURVE_WITH_KNOTS ( ( 4, 4 ),
 ( 4.712388980384689674, 6.283185307179586232 ),
 .UNSPECIFIED. ) 
 CURVE ( )  GEOMETRIC_REPRESENTATION_ITEM ( )  RATIONAL_B_SPLINE_CURVE ( ( 1.000000000000000000, 0.8047378541243649375, 0.8047378541243649375, 1.000000000000000000 ) ) 
 REPRESENTATION_ITEM ( '' )  );
#2779 = ORIENTED_EDGE ( 'NONE', *, *, #37076, .T. ) ;
#2780 = CARTESIAN_POINT ( 'NONE',  ( 340.0000000000000568, 169.0000000000000000, 357.9999999999997726 ) ) ;
#2781 = VERTEX_POINT ( 'NONE', #10722 ) ;
#2782 = ORIENTED_EDGE ( 'NONE', *, *, #37767, .T. ) ;
#2783 = ORIENTED_EDGE ( 'NONE', *, *, #20337, .F. ) ;
#2784 = DIRECTION ( 'NONE',  ( -1.000000000000000000, 0.000000000000000000, 0.000000000000000000 ) ) ;
#2785 = B_SPLINE_CURVE_WITH_KNOTS ( 'NONE', 3,
 ( #3000, #15827, #4285, #31492 ),
 .UNSPECIFIED., .F., .F.,
 ( 4, 4 ),
 ( 1.592264493058081649E-17, 0.009404495247862340590 ),
 .UNSPECIFIED. ) ;
#2786 =( BOUNDED_CURVE ( )  B_SPLINE_CURVE ( 3, ( #26945, #47166, #35176, #15144 ),
 .UNSPECIFIED., .F., .F. ) 
 B_SPLINE_CURVE_WITH_KNOTS ( ( 4, 4 ),
 ( 3.141592653589793116, 4.712388980384689674 ),
 .UNSPECIFIED. ) 
 CURVE ( )  GEOMETRIC_REPRESENTATION_ITEM ( )  RATIONAL_B_SPLINE_CURVE ( ( 1.000000000000000000, 0.8047378541243649375, 0.8047378541243649375, 1.000000000000000000 ) ) 
 REPRESENTATION_ITEM ( '' )  );
#2787 = DIRECTION ( 'NONE',  ( -1.000000000000000000, 0.000000000000000000, 1.586032892321651989E-16 ) ) ;
#2788 = B_SPLINE_SURFACE_WITH_KNOTS ( 'NONE', 3, 3, ( 
 ( #31024, #483, #31787, #47372 ),
 ( #3811, #19715, #35394, #31535 ),
 ( #9426, #35893, #33043, #32548 ),
 ( #12773, #16886, #17130, #48631 ) ),
 .UNSPECIFIED., .F., .F., .F.,
 ( 4, 4 ),
 ( 4, 4 ),
 ( 0.000000000000000000, 1.000000000000000000 ),
 ( 0.000000000000000000, 1.000000000000000000 ),
 .UNSPECIFIED. ) ;
#2789 = ORIENTED_EDGE ( 'NONE', *, *, #5538, .F. ) ;
#2790 = CARTESIAN_POINT ( 'NONE',  ( -206.6959734468149463, 1.750000000000009992, 0.8182875569279768335 ) ) ;
#2791 = CARTESIAN_POINT ( 'NONE',  ( -164.9999999999984936, 16.00000000000000000, 35.00000000000000000 ) ) ;
#2792 = VECTOR ( 'NONE', #31544, 1000.000000000000000 ) ;
#2793 = LINE ( 'NONE', #15874, #12076 ) ;
#2794 = CARTESIAN_POINT ( 'NONE',  ( 151.5540265531850537, -1.025126265847089879, -77.43171244307200141 ) ) ;
#2795 = ORIENTED_EDGE ( 'NONE', *, *, #50287, .F. ) ;
#2796 = CARTESIAN_POINT ( 'NONE',  ( -0.6369768774138663270, 1.285364331396255944, 9.950105812514292936 ) ) ;
#2797 = ADVANCED_FACE ( 'NONE', ( #42970 ), #38212, .F. ) ;
#2798 = EDGE_LOOP ( 'NONE', ( #14811, #28770, #6712, #21908, #31731, #40300, #17842, #23739, #30597, #13220, #37844, #41783 ) ) ;
#2799 = DIRECTION ( 'NONE',  ( -1.000000000000000000, 5.326388832052271710E-25, -1.587271980518778491E-16 ) ) ;
#2800 = DIRECTION ( 'NONE',  ( 1.000000000000000000, 0.000000000000000000, 0.000000000000000000 ) ) ;
#2801 = AXIS2_PLACEMENT_3D ( 'NONE', #27850, #12435, #39410 ) ;
#2802 = CARTESIAN_POINT ( 'NONE',  ( 8.001683061421385190, 5.997755262142701937, 9.282506307616484875 ) ) ;
#2803 = CARTESIAN_POINT ( 'NONE',  ( -44.94597344681493922, 2.143131898507880377E-16, 39.06828755692798438 ) ) ;
#2804 = ORIENTED_EDGE ( 'NONE', *, *, #38669, .F. ) ;
#2805 = CARTESIAN_POINT ( 'NONE',  ( 210.0000000000000568, 2.143131898507881856E-16, -120.9317124430720582 ) ) ;
#2806 = CARTESIAN_POINT ( 'NONE',  ( 23.26005729352310425, 44.90397804740356236, 7.906207997025717304 ) ) ;
#2807 = DIRECTION ( 'NONE',  ( 0.000000000000000000, -0.000000000000000000, -1.000000000000000000 ) ) ;
#2808 = CARTESIAN_POINT ( 'NONE',  ( 71.55402655318506788, 0.000000000000000000, 162.5682875569279702 ) ) ;
#2809 = AXIS2_PLACEMENT_3D ( 'NONE', #38403, #11199, #46799 ) ;
#2810 = PLANE ( 'NONE',  #22180 ) ;
#2811 = VERTEX_POINT ( 'NONE', #41527 ) ;
#2812 = VERTEX_POINT ( 'NONE', #23497 ) ;
#2813 = DIRECTION ( 'NONE',  ( -1.000000000000000000, -0.000000000000000000, -0.000000000000000000 ) ) ;
#2814 = ORIENTED_EDGE ( 'NONE', *, *, #43072, .F. ) ;
#2815 = CARTESIAN_POINT ( 'NONE',  ( -6.695973446814940111, -1.750000000000023759, 40.81828755692798438 ) ) ;
#2816 = DIRECTION ( 'NONE',  ( -1.000000000000000000, 0.000000000000000000, 0.000000000000000000 ) ) ;
#2817 = EDGE_LOOP ( 'NONE', ( #412, #31040, #39958, #40471 ) ) ;
#2818 = DIRECTION ( 'NONE',  ( -0.000000000000000000, -0.000000000000000000, 1.000000000000000000 ) ) ;
#2819 = ORIENTED_EDGE ( 'NONE', *, *, #38022, .T. ) ;
#2820 = VECTOR ( 'NONE', #30331, 1000.000000000000000 ) ;
#2821 = CARTESIAN_POINT ( 'NONE',  ( -85.67084718096784002, -1.750000000000009548, -0.2068387089191121020 ) ) ;
#2822 = ORIENTED_EDGE ( 'NONE', *, *, #6477, .T. ) ;
#2823 = DIRECTION ( 'NONE',  ( -0.000000000000000000, -1.000000000000000000, -0.000000000000000000 ) ) ;
#2824 = CARTESIAN_POINT ( 'NONE',  ( 40.00000000000000000, 4.898587196589413026E-15, 900.0000000000000000 ) ) ;
#2825 = DIRECTION ( 'NONE',  ( 0.000000000000000000, -0.4436251537532894806, -0.8962124318248270161 ) ) ;
#2826 = CARTESIAN_POINT ( 'NONE',  ( -88.44597344681497475, 0.000000000000000000, -117.4317124430720156 ) ) ;
#2827 = EDGE_CURVE ( 'NONE', #34035, #9083, #18668, .T. ) ;
#2828 = CARTESIAN_POINT ( 'NONE',  ( 177.5000000000000284, -112.5000000000000000, 0.000000000000000000 ) ) ;
#2829 = ORIENTED_EDGE ( 'NONE', *, *, #26161, .F. ) ;
#2830 = ORIENTED_EDGE ( 'NONE', *, *, #4563, .T. ) ;
#2831 = CARTESIAN_POINT ( 'NONE',  ( 210.0000000000000568, 0.000000000000000000, -79.18171244307201562 ) ) ;
#2832 = ORIENTED_EDGE ( 'NONE', *, *, #9784, .F. ) ;
#2833 = LINE ( 'NONE', #11570, #18533 ) ;
#2834 = CIRCLE ( 'NONE', #13502, 4.000000000000003553 ) ;
#2835 = CARTESIAN_POINT ( 'NONE',  ( 240.0000000000000000, -164.9999999999999716, 32.29650858650035161 ) ) ;
#2836 = EDGE_LOOP ( 'NONE', ( #15416, #20351, #9369, #19438 ) ) ;
#2837 = CARTESIAN_POINT ( 'NONE',  ( -44.94597344681493922, -1.025126265847088991, -157.4317124430720582 ) ) ;
#2838 = CARTESIAN_POINT ( 'NONE',  ( 155.0540265531850537, 2.143131898507880377E-16, -80.93171244307201562 ) ) ;
#2839 = VERTEX_POINT ( 'NONE', #10230 ) ;
#2840 = FACE_BOUND ( 'NONE', #31497, .T. ) ;
#2841 = CARTESIAN_POINT ( 'NONE',  ( 12.35406723005396046, -11.51001571518080624, 9.178419661560148768 ) ) ;
#2842 = CARTESIAN_POINT ( 'NONE',  ( -15.00000000000000000, 12.98684210526315930, -20.00000000000000000 ) ) ;
#2843 = LINE ( 'NONE', #46433, #10000 ) ;
#2844 = ORIENTED_EDGE ( 'NONE', *, *, #35570, .T. ) ;
#2845 = VERTEX_POINT ( 'NONE', #29728 ) ;
#2846 = CARTESIAN_POINT ( 'NONE',  ( 115.0540265531850395, 1.025126265847081664, 2.568287556927973281 ) ) ;
#2847 = LINE ( 'NONE', #46690, #18224 ) ;
#2848 = EDGE_LOOP ( 'NONE', ( #12548, #50011, #24278, #41729 ) ) ;
#2849 = EDGE_CURVE ( 'NONE', #36058, #16866, #34344, .T. ) ;
#2850 = ORIENTED_EDGE ( 'NONE', *, *, #28204, .F. ) ;
#2851 = DIRECTION ( 'NONE',  ( -0.2144099651976388021, 1.438973879383406636E-14, 0.9767437569925631058 ) ) ;
#2852 = CARTESIAN_POINT ( 'NONE',  ( -114.9999999999994031, 17.00000000000000000, -54.99999999999999289 ) ) ;
#2853 = DIRECTION ( 'NONE',  ( -1.000000000000000000, -0.000000000000000000, -0.000000000000000000 ) ) ;
#2854 = CARTESIAN_POINT ( 'NONE',  ( 114.3291528190321173, 1.749999999999996891, 79.79316129108087807 ) ) ;
#2855 = VECTOR ( 'NONE', #2017, 1000.000000000000000 ) ;
#2856 = SURFACE_STYLE_USAGE ( .BOTH. , #35210 ) ;
#2857 = LINE ( 'NONE', #42115, #24978 ) ;
#2858 = CARTESIAN_POINT ( 'NONE',  ( 210.0000000000000568, 0.000000000000000000, -37.43171244307202272 ) ) ;
#2859 = ORIENTED_EDGE ( 'NONE', *, *, #15510, .T. ) ;
#2860 = CARTESIAN_POINT ( 'NONE',  ( -1.724908962443186367, 9.880865948510580310, 9.516222621873128062 ) ) ;
#2861 = CARTESIAN_POINT ( 'NONE',  ( -4.207128120815918256E-14, 3.058192377181588826E-14, 10.00000000000000000 ) ) ;
#2862 = DIRECTION ( 'NONE',  ( 0.000000000000000000, 0.9152942571496521795, -0.4027858274925601445 ) ) ;
#2863 = VECTOR ( 'NONE', #30453, 1000.000000000000000 ) ;
#2864 = VERTEX_POINT ( 'NONE', #22021 ) ;
#2865 = VECTOR ( 'NONE', #35878, 1000.000000000000000 ) ;
#2866 = AXIS2_PLACEMENT_3D ( 'NONE', #16122, #31532, #31277 ) ;
#2867 = CARTESIAN_POINT ( 'NONE',  ( 115.0540265531850395, 1.025126265847082108, 82.56828755692798438 ) ) ;
#2868 = ORIENTED_EDGE ( 'NONE', *, *, #35603, .F. ) ;
#2869 = CARTESIAN_POINT ( 'NONE',  ( -166.6959734468149463, 0.000000000000000000, 165.0000000000000000 ) ) ;
#2870 = CARTESIAN_POINT ( 'NONE',  ( 1.365263087672787590, -0.5437404457008400138, 9.958264684458717042 ) ) ;
#2871 = CARTESIAN_POINT ( 'NONE',  ( 16.94310420131209227, -28.83076186680421671, -8.917361510505369182 ) ) ;
#2872 = VECTOR ( 'NONE', #1252, 1000.000000000000000 ) ;
#2873 = ORIENTED_EDGE ( 'NONE', *, *, #943, .F. ) ;
#2874 = ORIENTED_EDGE ( 'NONE', *, *, #44978, .T. ) ;
#2875 = CARTESIAN_POINT ( 'NONE',  ( 46.10908423965007330, 19.89422939639137766, 1.847720168420772691 ) ) ;
#2876 = CARTESIAN_POINT ( 'NONE',  ( 344.0000000000000000, 165.0000000000000000, -106.0000000000001990 ) ) ;
#2877 = LINE ( 'NONE', #14450, #7010 ) ;
#2878 = EDGE_CURVE ( 'NONE', #5639, #25771, #10477, .T. ) ;
#2879 = ORIENTED_EDGE ( 'NONE', *, *, #12373, .T. ) ;
#2880 = VERTEX_POINT ( 'NONE', #11947 ) ;
#2881 = LINE ( 'NONE', #50053, #43153 ) ;
#2882 = DIRECTION ( 'NONE',  ( 0.000000000000000000, 0.000000000000000000, -1.000000000000000000 ) ) ;
#2883 = ORIENTED_EDGE ( 'NONE', *, *, #47411, .F. ) ;
#2884 = ORIENTED_EDGE ( 'NONE', *, *, #5325, .T. ) ;
#2885 = CARTESIAN_POINT ( 'NONE',  ( -204.9459734468149463, 2.143131898507880377E-16, 79.06828755692797017 ) ) ;
#2886 = CARTESIAN_POINT ( 'NONE',  ( -64.99999999999877787, 17.00000000000000000, 30.00000000000000000 ) ) ;
#2887 = DIRECTION ( 'NONE',  ( 1.000000000000000000, 0.000000000000000000, 0.000000000000000000 ) ) ;
#2888 = VECTOR ( 'NONE', #14296, 1000.000000000000000 ) ;
#2889 = EDGE_LOOP ( 'NONE', ( #8359, #12907, #27713, #1484 ) ) ;
#2890 = CARTESIAN_POINT ( 'NONE',  ( -1.337801958641930300, -1.088266084286974689, 9.928159647716134018 ) ) ;
#2891 = ORIENTED_EDGE ( 'NONE', *, *, #43824, .T. ) ;
#2892 = ADVANCED_FACE ( 'NONE', ( #33590 ), #6373, .T. ) ;
#2893 = AXIS2_PLACEMENT_3D ( 'NONE', #43630, #40305, #24161 ) ;
#2894 = EDGE_CURVE ( 'NONE', #47489, #48612, #14926, .T. ) ;
#2895 = CARTESIAN_POINT ( 'NONE',  ( 350.0000000000000000, 167.0000000000000000, -356.0000000000002274 ) ) ;
#2896 = EDGE_CURVE ( 'NONE', #936, #48865, #18420, .T. ) ;
#2898 = VECTOR ( 'NONE', #22285, 1000.000000000000000 ) ;
#2897 = DIRECTION ( 'NONE',  ( -9.711650524620651178E-33, 1.223873602809432483E-48, -1.000000000000000000 ) ) ;
#2899 = EDGE_LOOP ( 'NONE', ( #926, #6392, #23218, #19533, #19849, #34241 ) ) ;
#2900 = VERTEX_POINT ( 'NONE', #45837 ) ;
#2901 = VECTOR ( 'NONE', #12023, 1000.000000000000000 ) ;
#2902 = ORIENTED_EDGE ( 'NONE', *, *, #25498, .T. ) ;
#2903 = CARTESIAN_POINT ( 'NONE',  ( 344.0000000000000000, -167.0000000000001137, 342.0000000000000000 ) ) ;
#2904 = CARTESIAN_POINT ( 'NONE',  ( -210.0000000000000568, 2.143131898507876926E-16, -80.93171244307202983 ) ) ;
#2905 = EDGE_LOOP ( 'NONE', ( #43290, #29468, #50497, #15454, #205 ) ) ;
#2906 = CARTESIAN_POINT ( 'NONE',  ( -0.9923808968704912470, 0.8303844723052444809, 9.947020512645417867 ) ) ;
#2907 = EDGE_CURVE ( 'NONE', #36589, #33796, #2778, .T. ) ;
#2908 = EDGE_CURVE ( 'NONE', #22082, #37470, #14575, .T. ) ;
#2909 = ORIENTED_EDGE ( 'NONE', *, *, #9784, .T. ) ;
#2910 = VECTOR ( 'NONE', #15592, 1000.000000000000000 ) ;
#2911 = DIRECTION ( 'NONE',  ( -1.000000000000000000, 0.000000000000000000, 0.000000000000000000 ) ) ;
#2912 = FILL_AREA_STYLE ('',( #41427 ) ) ;
#2913 = ORIENTED_EDGE ( 'NONE', *, *, #26154, .T. ) ;
#2914 = FACE_OUTER_BOUND ( 'NONE', #47406, .T. ) ;
#2915 =( BOUNDED_CURVE ( )  B_SPLINE_CURVE ( 3, ( #10716, #2520, #18415, #29980 ),
 .UNSPECIFIED., .F., .F. ) 
 B_SPLINE_CURVE_WITH_KNOTS ( ( 4, 4 ),
 ( 4.712388980384689674, 6.283185307179586232 ),
 .UNSPECIFIED. ) 
 CURVE ( )  GEOMETRIC_REPRESENTATION_ITEM ( )  RATIONAL_B_SPLINE_CURVE ( ( 1.000000000000000000, 0.8047378541243649375, 0.8047378541243649375, 1.000000000000000000 ) ) 
 REPRESENTATION_ITEM ( '' )  );
#2916 = EDGE_CURVE ( 'NONE', #31511, #25305, #21824, .T. ) ;
#2917 = CARTESIAN_POINT ( 'NONE',  ( 115.0540265531850395, 2.143131898507847836E-16, -37.43171244307205825 ) ) ;
#2918 = CARTESIAN_POINT ( 'NONE',  ( 75.05402655318509630, -1.025126265847089435, -117.4317124430720156 ) ) ;
#2919 = CARTESIAN_POINT ( 'NONE',  ( -14.99999999999845812, 17.00000000000000000, 35.00000000000000000 ) ) ;
#2920 = EDGE_CURVE ( 'NONE', #44875, #17662, #36277, .T. ) ;
#2921 = CARTESIAN_POINT ( 'NONE',  ( -166.6959734468149463, -1.750000000000010658, -119.1817124430720440 ) ) ;
#2922 = ORIENTED_EDGE ( 'NONE', *, *, #5675, .F. ) ;
#2923 =( BOUNDED_CURVE ( )  B_SPLINE_CURVE ( 3, ( #6080, #21726, #2235, #42481 ),
 .UNSPECIFIED., .F., .F. ) 
 B_SPLINE_CURVE_WITH_KNOTS ( ( 4, 4 ),
 ( 1.570796326794896558, 3.141592653589793116 ),
 .UNSPECIFIED. ) 
 CURVE ( )  GEOMETRIC_REPRESENTATION_ITEM ( )  RATIONAL_B_SPLINE_CURVE ( ( 1.000000000000000000, 0.8047378541243649375, 0.8047378541243649375, 1.000000000000000000 ) ) 
 REPRESENTATION_ITEM ( '' )  );
#2924 = EDGE_CURVE ( 'NONE', #42077, #42464, #39827, .T. ) ;
#2925 = LINE ( 'NONE', #2681, #43678 ) ;
#2926 = DIRECTION ( 'NONE',  ( -1.000000000000000000, 0.000000000000000000, 0.000000000000000000 ) ) ;
#2927 = CARTESIAN_POINT ( 'NONE',  ( 72.27890028733797578, 1.750000000000009548, -38.15658617722494483 ) ) ;
#2928 = CIRCLE ( 'NONE', #2149, 4.000000000000003553 ) ;
#2929 = CARTESIAN_POINT ( 'NONE',  ( 0.3862712429686810944, 1.188820645368943607, 10.00000000000000000 ) ) ;
#2930 = AXIS2_PLACEMENT_3D ( 'NONE', #5505, #48309, #9612 ) ;
#2931 = CARTESIAN_POINT ( 'NONE',  ( -225.0000000000000568, 164.9999999999999716, 372.0000000000000000 ) ) ;
#2932 = FACE_OUTER_BOUND ( 'NONE', #31942, .T. ) ;
#2933 =( BOUNDED_CURVE ( )  B_SPLINE_CURVE ( 3, ( #26666, #25209, #13891, #30775 ),
 .UNSPECIFIED., .F., .F. ) 
 B_SPLINE_CURVE_WITH_KNOTS ( ( 4, 4 ),
 ( 1.570796326794886788, 1.795031077903984418 ),
 .UNSPECIFIED. ) 
 CURVE ( )  GEOMETRIC_REPRESENTATION_ITEM ( )  RATIONAL_B_SPLINE_CURVE ( ( 1.000000000000000000, 0.9958142854328206894, 0.9958142854328206894, 1.000000000000000000 ) ) 
 REPRESENTATION_ITEM ( '' )  );
#2934 = ADVANCED_FACE ( 'NONE', ( #44477 ), #8850, .F. ) ;
#2935 = CARTESIAN_POINT ( 'NONE',  ( 45.64490844644691236, 21.32281559348795952, 8.807470649214879543 ) ) ;
#2936 = ORIENTED_EDGE ( 'NONE', *, *, #20797, .T. ) ;
#2937 = SURFACE_SIDE_STYLE ('',( #15705 ) ) ;
#2938 = VECTOR ( 'NONE', #50385, 1000.000000000000000 ) ;
#2939 = ADVANCED_FACE ( 'NONE', ( #36322 ), #4745, .T. ) ;
#2940 = ADVANCED_FACE ( 'NONE', ( #24505 ), #43982, .T. ) ;
#2941 = DIRECTION ( 'NONE',  ( -1.000000000000000000, -0.000000000000000000, -0.000000000000000000 ) ) ;
#2942=STYLED_ITEM('',(#50747),#21395);
#2943 = CARTESIAN_POINT ( 'NONE',  ( -23.82716369509181575, -44.49195112875988656, 8.356839323120299312 ) ) ;
#2944 = CARTESIAN_POINT ( 'NONE',  ( 9.260964247899973856, -13.84230907185609460, -9.683996418299976483 ) ) ;
#2945 = CARTESIAN_POINT ( 'NONE',  ( 0.000000000000000000, -184.7999999999999545, 359.7999999999997840 ) ) ;
#2946 = EDGE_CURVE ( 'NONE', #891, #3572, #16803, .T. ) ;
#2947 = ORIENTED_EDGE ( 'NONE', *, *, #9831, .T. ) ;
#2948 = VERTEX_POINT ( 'NONE', #28353 ) ;
#2949 = SPHERICAL_SURFACE ( 'NONE', #43069, 0.5000000000000000000 ) ;
#2950 = EDGE_CURVE ( 'NONE', #40469, #36951, #13197, .T. ) ;
#2951 = AXIS2_PLACEMENT_3D ( 'NONE', #20075, #19309, #11624 ) ;
#2952 = CARTESIAN_POINT ( 'NONE',  ( -4.672045878990125800, 50.00000000000000711, 1.847720168420772691 ) ) ;
#2953 = VERTEX_POINT ( 'NONE', #912 ) ;
#2954 = CARTESIAN_POINT ( 'NONE',  ( -36.08557433729205144, 35.58569447144795816, 7.455576670931136185 ) ) ;
#2955 = CARTESIAN_POINT ( 'NONE',  ( 193.3040265531851105, 1.750000000000010214, -39.18171244307202983 ) ) ;
#2956 = CARTESIAN_POINT ( 'NONE',  ( 85.00000000000090949, 17.00000000000000000, -24.99999999999999289 ) ) ;
#2957 = EDGE_LOOP ( 'NONE', ( #35682, #1523, #14776, #47922, #39971, #20751 ) ) ;
#2958 = ORIENTED_EDGE ( 'NONE', *, *, #2310, .T. ) ;
#2959 = ORIENTED_EDGE ( 'NONE', *, *, #42129, .T. ) ;
#2960 = CARTESIAN_POINT ( 'NONE',  ( 344.0000000000000000, -167.0000000000001137, -349.9999999999998863 ) ) ;
#2961 = DIRECTION ( 'NONE',  ( -0.000000000000000000, -1.000000000000000000, -0.000000000000000000 ) ) ;
#2962 = CARTESIAN_POINT ( 'NONE',  ( -1.011271242968693862, 0.7347315653655780432, -3.333333333333333481 ) ) ;
#2963 = ORIENTED_EDGE ( 'NONE', *, *, #24972, .T. ) ;
#2964 = CARTESIAN_POINT ( 'NONE',  ( -38.83486119589580454, 15.16159403945161621, -9.387872844313825738 ) ) ;
#2965 = VECTOR ( 'NONE', #33104, 1000.000000000000000 ) ;
#2966 = CARTESIAN_POINT ( 'NONE',  ( -7.241383964640739634, -3.035766082959412415E-15, -5.000000000000000000 ) ) ;
#2967 = DIRECTION ( 'NONE',  ( -6.938893903907222461E-16, -0.000000000000000000, -1.000000000000000000 ) ) ;
#2968 = EDGE_LOOP ( 'NONE', ( #14933, #7197, #19117, #5943 ) ) ;
#2969 = EDGE_CURVE ( 'NONE', #10537, #47246, #45013, .T. ) ;
#2970 = AXIS2_PLACEMENT_3D ( 'NONE', #7481, #38785, #33917 ) ;
#2971 = ORIENTED_EDGE ( 'NONE', *, *, #30880, .T. ) ;
#2972 = CARTESIAN_POINT ( 'NONE',  ( 111.5540265531850537, -1.025126265847081442, 159.0682875569279418 ) ) ;
#2973 = CARTESIAN_POINT ( 'NONE',  ( 1.841313484560079816, 1.034875822465065820, 9.884520277910693764 ) ) ;
#2974 = CARTESIAN_POINT ( 'NONE',  ( 210.0000000000000568, 2.143131898507881116E-16, 39.06828755692797728 ) ) ;
#2975 = ORIENTED_EDGE ( 'NONE', *, *, #2473, .F. ) ;
#2976 = ORIENTED_EDGE ( 'NONE', *, *, #28015, .T. ) ;
#2977 = CARTESIAN_POINT ( 'NONE',  ( 0.000000000000000000, 17.00000000000000000, 0.000000000000000000 ) ) ;
#2978 = CARTESIAN_POINT ( 'NONE',  ( -19.99999999999815969, 16.00000000000000000, 90.00000000000000000 ) ) ;
#2979 = VECTOR ( 'NONE', #15930, 1000.000000000000000 ) ;
#2980 = EDGE_CURVE ( 'NONE', #2364, #49857, #50235, .T. ) ;
#2981 = DIRECTION ( 'NONE',  ( 0.000000000000000000, 1.000000000000000000, 0.000000000000000000 ) ) ;
#2982 = CARTESIAN_POINT ( 'NONE',  ( -86.69597344681494633, 1.750000000000009992, -159.1817124430720298 ) ) ;
#2983 = ADVANCED_FACE ( 'NONE', ( #27852 ), #43485, .T. ) ;
#2984 = MECHANICAL_DESIGN_GEOMETRIC_PRESENTATION_REPRESENTATION (  '', ( #20173 ), #3804 ) ;
#2985 = CARTESIAN_POINT ( 'NONE',  ( 210.0000000000000568, 2.143131898507881856E-16, 119.0682875569279560 ) ) ;
#2986 = EDGE_LOOP ( 'NONE', ( #17759, #28658, #20389, #1956 ) ) ;
#2987 = CARTESIAN_POINT ( 'NONE',  ( 339.9999999999999432, 181.0000000000000284, -344.0000000000001705 ) ) ;
#2988 = EDGE_CURVE ( 'NONE', #8719, #14950, #29690, .T. ) ;
#2989 = CARTESIAN_POINT ( 'NONE',  ( 9.221081804193270059, 13.81382350053991104, 3.266473740018926541 ) ) ;
#2990 = ADVANCED_FACE ( 'NONE', ( #8356 ), #5248, .F. ) ;
#2991 = LINE ( 'NONE', #31482, #32243 ) ;
#2992 = DIRECTION ( 'NONE',  ( 0.000000000000000000, -0.000000000000000000, 1.000000000000000000 ) ) ;
#2993 = AXIS2_PLACEMENT_3D ( 'NONE', #43795, #24563, #24067 ) ;
#2994 = ADVANCED_FACE ( 'NONE', ( #16299 ), #31960, .T. ) ;
#2995 = FACE_OUTER_BOUND ( 'NONE', #40559, .T. ) ;
#2996 = DIRECTION ( 'NONE',  ( -1.000000000000000000, -0.000000000000000000, -0.000000000000000000 ) ) ;
#2997 = VERTEX_POINT ( 'NONE', #10368 ) ;
#2998 = CARTESIAN_POINT ( 'NONE',  ( 3.996390545799824334, -16.57371371864897469, 8.953103998512858652 ) ) ;
#2999 = DIRECTION ( 'NONE',  ( 0.000000000000000000, 0.000000000000000000, 1.000000000000000000 ) ) ;
#3000 = CARTESIAN_POINT ( 'NONE',  ( 8.001683061421385190, 5.997755262142701937, 9.282506307616484875 ) ) ;
#3001 = ORIENTED_EDGE ( 'NONE', *, *, #9563, .F. ) ;
#3002 = CARTESIAN_POINT ( 'NONE',  ( 224.9999999999999716, -175.0000000000000000, 62.29650858650038003 ) ) ;
#3003 = AXIS2_PLACEMENT_3D ( 'NONE', #28425, #36657, #24825 ) ;
#3004 = EDGE_CURVE ( 'NONE', #20642, #23633, #49307, .T. ) ;
#3005 = CARTESIAN_POINT ( 'NONE',  ( 154.1026953830863420, -98.56198943095992604, -17.65743994998277699 ) ) ;
#3006 = ORIENTED_EDGE ( 'NONE', *, *, #34345, .F. ) ;
#3007 = LINE ( 'NONE', #14304, #29645 ) ;
#3008 = DIRECTION ( 'NONE',  ( 1.000000000000000000, 0.000000000000000000, -9.251858538543084240E-16 ) ) ;
#3009 = LINE ( 'NONE', #18655, #2073 ) ;
#3010 = ORIENTED_EDGE ( 'NONE', *, *, #11718, .T. ) ;
#3011 = CARTESIAN_POINT ( 'NONE',  ( -9.221081804193374865, -13.81382350053984176, 3.266473740018926541 ) ) ;
#3012 = VERTEX_POINT ( 'NONE', #13698 ) ;
#3013 = ORIENTED_EDGE ( 'NONE', *, *, #1265, .T. ) ;
#3014 = LINE ( 'NONE', #2762, #17264 ) ;
#3015 = ORIENTED_EDGE ( 'NONE', *, *, #25363, .T. ) ;
#3016 = CARTESIAN_POINT ( 'NONE',  ( 111.5540265531850679, 0.000000000000000000, -40.93171244307202983 ) ) ;
#3017 = DIRECTION ( 'NONE',  ( -0.000000000000000000, -1.000000000000000000, -0.000000000000000000 ) ) ;
#3018 =( BOUNDED_CURVE ( )  B_SPLINE_CURVE ( 3, ( #36533, #47755, #4204, #4708 ),
 .UNSPECIFIED., .F., .F. ) 
 B_SPLINE_CURVE_WITH_KNOTS ( ( 4, 4 ),
 ( 4.712388980384689674, 6.283185307179586232 ),
 .UNSPECIFIED. ) 
 CURVE ( )  GEOMETRIC_REPRESENTATION_ITEM ( )  RATIONAL_B_SPLINE_CURVE ( ( 1.000000000000000000, 0.8047378541243649375, 0.8047378541243649375, 1.000000000000000000 ) ) 
 REPRESENTATION_ITEM ( '' )  );
#3019 = CARTESIAN_POINT ( 'NONE',  ( 339.9999999999998863, -168.9999999999999432, 359.9999999999998295 ) ) ;
#3020 = EDGE_CURVE ( 'NONE', #4421, #16851, #21653, .T. ) ;
#3021 = CARTESIAN_POINT ( 'NONE',  ( 135.0000000000003411, 17.00000000000000000, -84.99999999999998579 ) ) ;
#3022 = CARTESIAN_POINT ( 'NONE',  ( 195.0540265531851105, 2.143131898507880377E-16, 165.0000000000000000 ) ) ;
#3023 = EDGE_LOOP ( 'NONE', ( #44750, #47253, #35868, #13821, #14713 ) ) ;
#3024 = VECTOR ( 'NONE', #43424, 1000.000000000000000 ) ;
#3025 = DIRECTION ( 'NONE',  ( 0.000000000000000000, 0.000000000000000000, 1.000000000000000000 ) ) ;
#3026 = LINE ( 'NONE', #46094, #25786 ) ;
#3027 = PLANE ( 'NONE',  #15241 ) ;
#3028 = CARTESIAN_POINT ( 'NONE',  ( -22.82242230425432439, -2.816136035261162185, 226.0000000000000000 ) ) ;
#3029 = ORIENTED_EDGE ( 'NONE', *, *, #18887, .F. ) ;
#3030 = CARTESIAN_POINT ( 'NONE',  ( 356.0000000000000000, -167.0000000000001137, -342.0000000000003411 ) ) ;
#3031 = CARTESIAN_POINT ( 'NONE',  ( 350.0000000000000000, -184.9999999999999716, -360.0000000000002274 ) ) ;
#3032 = ORIENTED_EDGE ( 'NONE', *, *, #46572, .T. ) ;
#3033 =( REPRESENTATION_RELATIONSHIP ('NONE','NONE', #45699, #13952 ) REPRESENTATION_RELATIONSHIP_WITH_TRANSFORMATION ( #20544 )SHAPE_REPRESENTATION_RELATIONSHIP( ) );
#3034 = EDGE_LOOP ( 'NONE', ( #18109, #6648, #12703, #38229 ) ) ;
#3035 = ORIENTED_EDGE ( 'NONE', *, *, #8382, .F. ) ;
#3036 = DIRECTION ( 'NONE',  ( -0.000000000000000000, -0.000000000000000000, -1.000000000000000000 ) ) ;
#3037 = FACE_OUTER_BOUND ( 'NONE', #21079, .T. ) ;
#3038 = VERTEX_POINT ( 'NONE', #6505 ) ;
#3039 = LINE ( 'NONE', #17694, #20841 ) ;
#3040 = CARTESIAN_POINT ( 'NONE',  ( -14.99999999999812594, 17.00000000000000000, 90.00000000000000000 ) ) ;
#3041 = DIRECTION ( 'NONE',  ( 0.000000000000000000, -0.000000000000000000, -1.000000000000000000 ) ) ;
#3042 = ADVANCED_FACE ( 'NONE', ( #2650, #14191 ), #29862, .T. ) ;
#3043 = CARTESIAN_POINT ( 'NONE',  ( 35.00000000000122213, 17.00000000000000000, 30.00000000000000000 ) ) ;
#3044 = CARTESIAN_POINT ( 'NONE',  ( -14.99999999999937472, 17.00000000000000000, -30.00000000000000000 ) ) ;
#3045 = EDGE_CURVE ( 'NONE', #23318, #42480, #30981, .T. ) ;
#3046 = AXIS2_PLACEMENT_3D ( 'NONE', #25399, #10254, #18187 ) ;
#3047 = DIRECTION ( 'NONE',  ( 0.000000000000000000, -1.000000000000000000, 0.000000000000000000 ) ) ;
#3048 = CARTESIAN_POINT ( 'NONE',  ( 73.30402655318508209, 0.000000000000000000, 165.0000000000000000 ) ) ;
#3049 = EDGE_CURVE ( 'NONE', #32394, #22969, #49558, .T. ) ;
#3050 = CARTESIAN_POINT ( 'NONE',  ( -0.5133303889063141057, 1.273801409042568888, 9.946805383069623474 ) ) ;
#3051 = VERTEX_POINT ( 'NONE', #2167 ) ;
#3052 = EDGE_CURVE ( 'NONE', #43342, #34175, #49058, .T. ) ;
#3053 = EDGE_CURVE ( 'NONE', #40413, #29620, #38717, .T. ) ;
#3054 = DIRECTION ( 'NONE',  ( -1.000000000000000000, -0.000000000000000000, -0.000000000000000000 ) ) ;
#3055 = CARTESIAN_POINT ( 'NONE',  ( 25.63461350838963426, -43.17876197216376966, -8.016098858316199838 ) ) ;
#3056 = LINE ( 'NONE', #18700, #32288 ) ;
#3057 = DIRECTION ( 'NONE',  ( 0.000000000000000000, 0.000000000000000000, 1.000000000000000000 ) ) ;
#3058 = ORIENTED_EDGE ( 'NONE', *, *, #5388, .F. ) ;
#3059 = CARTESIAN_POINT ( 'NONE',  ( -165.6708471809677974, 1.750000000000010214, 119.7931612910808781 ) ) ;
#3060 = CARTESIAN_POINT ( 'NONE',  ( -24.87968592351613495, -28.06706927586046518, -8.600750091277037157 ) ) ;
#3061 = EDGE_CURVE ( 'NONE', #9299, #5041, #18513, .T. ) ;
#3062 = CARTESIAN_POINT ( 'NONE',  ( 34.08355720199905647, -2.371364769369109116, 7.455576670931136185 ) ) ;
#3063 = PLANE ( 'NONE',  #26611 ) ;
#3064 = EDGE_LOOP ( 'NONE', ( #38905, #19899, #45220, #15309 ) ) ;
#3065 = LINE ( 'NONE', #37994, #26446 ) ;
#3066 = VERTEX_POINT ( 'NONE', #25504 ) ;
#3067 = CARTESIAN_POINT ( 'NONE',  ( 169.0000000000000000, -184.9999999999999716, -115.0000000000001137 ) ) ;
#3068 = ORIENTED_EDGE ( 'NONE', *, *, #48539, .F. ) ;
#3069 = CARTESIAN_POINT ( 'NONE',  ( 1.267276237729528354, -0.08162529406826456169, 9.975314328424614629 ) ) ;
#3070 = DIRECTION ( 'NONE',  ( -0.000000000000000000, -0.000000000000000000, -1.000000000000000000 ) ) ;
#3071 = ORIENTED_EDGE ( 'NONE', *, *, #26122, .T. ) ;
#3072 = DIRECTION ( 'NONE',  ( -1.000000000000000000, -0.000000000000000000, -0.000000000000000000 ) ) ;
#3073 = ORIENTED_EDGE ( 'NONE', *, *, #30278, .T. ) ;
#3074 =( BOUNDED_CURVE ( )  B_SPLINE_CURVE ( 3, ( #13599, #45631, #9744, #34135 ),
 .UNSPECIFIED., .F., .F. ) 
 B_SPLINE_CURVE_WITH_KNOTS ( ( 4, 4 ),
 ( 4.712388980384689674, 6.283185307179586232 ),
 .UNSPECIFIED. ) 
 CURVE ( )  GEOMETRIC_REPRESENTATION_ITEM ( )  RATIONAL_B_SPLINE_CURVE ( ( 1.000000000000000000, 0.8047378541243649375, 0.8047378541243649375, 1.000000000000000000 ) ) 
 REPRESENTATION_ITEM ( '' )  );
#3075 = CARTESIAN_POINT ( 'NONE',  ( 0.3862712429686978033, -1.188820645368937834, 10.00000000000000000 ) ) ;
#3076 = AXIS2_PLACEMENT_3D ( 'NONE', #25784, #41431, #22936 ) ;
#3077 = ORIENTED_EDGE ( 'NONE', *, *, #19358, .F. ) ;
#3078 = LINE ( 'NONE', #33899, #2422 ) ;
#3079 = CARTESIAN_POINT ( 'NONE',  ( 80.00000000000028422, 17.00000000000000000, -60.00000000000000000 ) ) ;
#3080 = ORIENTED_EDGE ( 'NONE', *, *, #47279, .F. ) ;
#3081 = DIRECTION ( 'NONE',  ( 0.000000000000000000, 0.000000000000000000, -1.000000000000000000 ) ) ;
#3082 = FACE_OUTER_BOUND ( 'NONE', #32907, .T. ) ;
#3083 = LINE ( 'NONE', #23094, #39682 ) ;
#3084 =( BOUNDED_CURVE ( )  B_SPLINE_CURVE ( 3, ( #19137, #27112, #19659, #11455 ),
 .UNSPECIFIED., .F., .F. ) 
 B_SPLINE_CURVE_WITH_KNOTS ( ( 4, 4 ),
 ( 1.570796326794896558, 3.141592653589793116 ),
 .UNSPECIFIED. ) 
 CURVE ( )  GEOMETRIC_REPRESENTATION_ITEM ( )  RATIONAL_B_SPLINE_CURVE ( ( 1.000000000000000000, 0.8047378541243649375, 0.8047378541243649375, 1.000000000000000000 ) ) 
 REPRESENTATION_ITEM ( '' )  );
#3085 = EDGE_LOOP ( 'NONE', ( #2922, #23541, #10418, #18159, #25180, #45487 ) ) ;
#3086 = VERTEX_POINT ( 'NONE', #29606 ) ;
#3087 = LINE ( 'NONE', #10042, #48814 ) ;
#3088 = EDGE_CURVE ( 'NONE', #26328, #3380, #34892, .T. ) ;
#3089 = CARTESIAN_POINT ( 'NONE',  ( -0.7601424845489993531, 1.297311920617006065, 9.927319414211224213 ) ) ;
#3090 = ORIENTED_EDGE ( 'NONE', *, *, #5480, .T. ) ;
#3091 = FACE_OUTER_BOUND ( 'NONE', #10508, .T. ) ;
#3092 = PLANE ( 'NONE',  #35201 ) ;
#3093 = EDGE_LOOP ( 'NONE', ( #8101, #18855, #13246, #36911 ) ) ;
#3094 = CARTESIAN_POINT ( 'NONE',  ( -168.4459734468149463, 0.000000000000000000, 82.56828755692798438 ) ) ;
#3095 = TOROIDAL_SURFACE ( 'NONE', #31808, 27.58190990837850265, 8.000000000000000000 ) ;
#3096 = DIRECTION ( 'NONE',  ( -1.000000000000000000, -0.000000000000000000, 4.625929269271635797E-16 ) ) ;
#3097 = B_SPLINE_SURFACE_WITH_KNOTS ( 'NONE', 3, 3, ( 
 ( #32175, #8823, #8072, #39378 ),
 ( #23961, #47013, #24476, #4214 ),
 ( #35528, #40125, #16018, #4956 ),
 ( #20613, #36292, #16768, #10337 ) ),
 .UNSPECIFIED., .F., .F., .F.,
 ( 4, 4 ),
 ( 4, 4 ),
 ( 0.000000000000000000, 1.000000000000000000 ),
 ( 0.000000000000000000, 1.000000000000000000 ),
 .UNSPECIFIED. ) ;
#3098 = ORIENTED_EDGE ( 'NONE', *, *, #1117, .T. ) ;
#3099 = FACE_OUTER_BOUND ( 'NONE', #17848, .T. ) ;
#3100 = CARTESIAN_POINT ( 'NONE',  ( 13.59579750444771307, -10.60877755095900632, 8.727788335465566760 ) ) ;
#3101 = DIRECTION ( 'NONE',  ( 0.000000000000000000, 0.000000000000000000, 1.000000000000000000 ) ) ;
#3102 = CARTESIAN_POINT ( 'NONE',  ( -114.9999999999991047, 17.00000000000000000, -24.99999999999999289 ) ) ;
#3103 = ADVANCED_FACE ( 'NONE', ( #10104 ), #40907, .F. ) ;
#3104 = ORIENTED_EDGE ( 'NONE', *, *, #47830, .T. ) ;
#3105 = CARTESIAN_POINT ( 'NONE',  ( 1.011271242968688311, -0.7347315653655855927, 10.00000000000000000 ) ) ;
#3106 = CARTESIAN_POINT ( 'NONE',  ( 30.00000000000187228, 17.00000000000000000, 65.00000000000000000 ) ) ;
#3107 = CARTESIAN_POINT ( 'NONE',  ( 33.16902712922644270, -37.70469005304286725, 1.847720168420772691 ) ) ;
#3108 = ORIENTED_EDGE ( 'NONE', *, *, #35912, .F. ) ;
#3109 = EDGE_LOOP ( 'NONE', ( #26223, #41186, #50645, #15630 ) ) ;
#3110 = EDGE_CURVE ( 'NONE', #15554, #9081, #37082, .T. ) ;
#3111 = EDGE_CURVE ( 'NONE', #20412, #42459, #33229, .T. ) ;
#3112 = DIRECTION ( 'NONE',  ( -1.000000000000000000, 0.000000000000000000, 0.000000000000000000 ) ) ;
#3113 = CARTESIAN_POINT ( 'NONE',  ( -2.595273106918313033, -2.906811120256372671, 9.741991644047246268 ) ) ;
#3114 = CARTESIAN_POINT ( 'NONE',  ( 115.0540265531850395, 2.143131898507847836E-16, 79.06828755692798438 ) ) ;
#3115 = AXIS2_PLACEMENT_3D ( 'NONE', #37666, #37173, #45809 ) ;
#3116 = CARTESIAN_POINT ( 'NONE',  ( 35.00000000000028422, 17.00000000000000000, -84.99999999999998579 ) ) ;
#3117 = CARTESIAN_POINT ( 'NONE',  ( 339.9999999999999432, 181.0000000000000284, -356.0000000000002274 ) ) ;
#3118 = CARTESIAN_POINT ( 'NONE',  ( -19.99999999999878142, 17.00000000000000000, 5.000000000000004441 ) ) ;
#3119 = ORIENTED_EDGE ( 'NONE', *, *, #9665, .F. ) ;
#3120 = EDGE_CURVE ( 'NONE', #18505, #50033, #41449, .T. ) ;
#3121 = DIRECTION ( 'NONE',  ( 0.000000000000000000, -2.265761274745217480E-16, 1.000000000000000000 ) ) ;
#3122 = CARTESIAN_POINT ( 'NONE',  ( 0.000000000000000000, 181.0000000000000284, -358.0000000000002274 ) ) ;
#3123 = DIRECTION ( 'NONE',  ( 0.5038710255240859137, 0.000000000000000000, -0.8637789008984335659 ) ) ;
#3124 = FILL_AREA_STYLE ('',( #34977 ) ) ;
#3125 = ORIENTED_EDGE ( 'NONE', *, *, #489, .F. ) ;
#3126 = DIRECTION ( 'NONE',  ( -1.000000000000000000, -0.000000000000000000, -0.000000000000000000 ) ) ;
#3127 = EDGE_LOOP ( 'NONE', ( #32010, #30119, #20434, #19432, #32405, #5133, #24170, #17306 ) ) ;
#3128 = DIRECTION ( 'NONE',  ( 0.000000000000000000, 0.000000000000000000, -1.000000000000000000 ) ) ;
#3129 = LINE ( 'NONE', #31107, #42142 ) ;
#3130 = LINE ( 'NONE', #43162, #23045 ) ;
#3131 = ORIENTED_EDGE ( 'NONE', *, *, #37323, .T. ) ;
#3132 = CARTESIAN_POINT ( 'NONE',  ( -210.0000000000000568, 0.000000000000000000, -39.18171244307202983 ) ) ;
#3133 = ORIENTED_EDGE ( 'NONE', *, *, #29928, .F. ) ;
#3134 = CARTESIAN_POINT ( 'NONE',  ( 32.43949840348898306, 7.871562655726499713, -9.367992836599954742 ) ) ;
#3135 = DIRECTION ( 'NONE',  ( 0.000000000000000000, 0.000000000000000000, 1.000000000000000000 ) ) ;
#3136 = CARTESIAN_POINT ( 'NONE',  ( 210.0000000000000568, 0.000000000000000000, 160.8182875569279702 ) ) ;
#3137 = VERTEX_POINT ( 'NONE', #17806 ) ;
#3138 = ORIENTED_EDGE ( 'NONE', *, *, #22162, .F. ) ;
#3139 = CARTESIAN_POINT ( 'NONE',  ( -208.4459734468148611, -1.025126265847089435, 162.5682875569279133 ) ) ;
#3140 = CARTESIAN_POINT ( 'NONE',  ( 16.07893968642772364, 33.88550589494195009, 8.100132398494510610 ) ) ;
#3141 = ADVANCED_FACE ( 'NONE', ( #21916 ), #37583, .F. ) ;
#3142 = VECTOR ( 'NONE', #25991, 1000.000000000000000 ) ;
#3143 = EDGE_LOOP ( 'NONE', ( #11241, #17569, #15727, #15784, #45336, #25581 ) ) ;
#3144 = B_SPLINE_CURVE_WITH_KNOTS ( 'NONE', 3,
 ( #41947, #21682, #49592, #49093 ),
 .UNSPECIFIED., .F., .F.,
 ( 4, 4 ),
 ( 0.000000000000000000, 0.001246897409371962393 ),
 .UNSPECIFIED. ) ;
#3145 = ORIENTED_EDGE ( 'NONE', *, *, #1325, .F. ) ;
#3146 = DIRECTION ( 'NONE',  ( -1.000000000000000000, 0.000000000000000000, -1.612977847700450206E-50 ) ) ;
#3147 = LINE ( 'NONE', #46728, #12000 ) ;
#3148 = DIRECTION ( 'NONE',  ( 0.000000000000000000, 1.000000000000000000, 3.186989995019654210E-49 ) ) ;
#3149 = ORIENTED_EDGE ( 'NONE', *, *, #42550, .T. ) ;
#3150 = PLANE ( 'NONE',  #12025 ) ;
#3151 = ORIENTED_EDGE ( 'NONE', *, *, #8795, .F. ) ;
#3152 = CARTESIAN_POINT ( 'NONE',  ( 0.3862712429686894766, -1.188820645368940276, 3.333333333333333481 ) ) ;
#3153 = CLOSED_SHELL ( 'NONE', ( #5898, #9220, #18286, #37671, #20586, #18104, #14876, #883, #26048, #41307 ) ) ;
#3154 = LINE ( 'NONE', #18300, #28798 ) ;
#3155 = ORIENTED_EDGE ( 'NONE', *, *, #27453, .F. ) ;
#3156 = VERTEX_POINT ( 'NONE', #34744 ) ;
#3157 = SHAPE_REPRESENTATION ( 'tire assembly', ( #30773, #21744, #15200 ), #25855 ) ;
#3158 = ORIENTED_EDGE ( 'NONE', *, *, #41068, .F. ) ;
#3159 = CARTESIAN_POINT ( 'NONE',  ( 85.00000000000123634, 17.00000000000000000, 5.000000000000004441 ) ) ;
#3160 = CARTESIAN_POINT ( 'NONE',  ( -167.7210997126620384, 1.750000000000010436, -120.2068387089191219 ) ) ;
#3161 = EDGE_LOOP ( 'NONE', ( #20847, #24621, #34113, #33708 ) ) ;
#3162 = PLANE ( 'NONE',  #17396 ) ;
#3163 = ORIENTED_EDGE ( 'NONE', *, *, #23730, .F. ) ;
#3164 = DIRECTION ( 'NONE',  ( 0.000000000000000000, 1.000000000000000000, 0.000000000000000000 ) ) ;
#3165 = CARTESIAN_POINT ( 'NONE',  ( 356.0000000000000000, -165.0000000000001137, 339.9999999999999432 ) ) ;
#3166 = ORIENTED_EDGE ( 'NONE', *, *, #19090, .F. ) ;
#3167 = CARTESIAN_POINT ( 'NONE',  ( -208.4459734468149463, 0.000000000000000000, 2.568287556927978166 ) ) ;
#3168 = DIRECTION ( 'NONE',  ( -1.612977847700450206E-50, 0.000000000000000000, -1.000000000000000000 ) ) ;
#3169 = CARTESIAN_POINT ( 'NONE',  ( -88.44597344681494633, 1.025126265847089213, -37.43171244307202272 ) ) ;
#3170 = CARTESIAN_POINT ( 'NONE',  ( 71.55402655318505367, 0.000000000000000000, -0.9317124430720524764 ) ) ;
#3171 = ORIENTED_EDGE ( 'NONE', *, *, #26645, .F. ) ;
#3172 = EDGE_CURVE ( 'NONE', #43697, #47413, #15239, .T. ) ;
#3173 = CYLINDRICAL_SURFACE ( 'NONE', #24749, 0.5000000000000007772 ) ;
#3174 = LINE ( 'NONE', #49089, #37999 ) ;
#3175 = DIRECTION ( 'NONE',  ( 1.000000000000000000, 0.000000000000000000, 0.000000000000000000 ) ) ;
#3176 = CARTESIAN_POINT ( 'NONE',  ( -20.00000000000003197, 16.00000000000000000, -114.9999999999999858 ) ) ;
#3177 = B_SPLINE_CURVE_WITH_KNOTS ( 'NONE', 3,
 ( #11859, #19027, #3644, #20057 ),
 .UNSPECIFIED., .F., .F.,
 ( 4, 4 ),
 ( 0.000000000000000000, 0.0009539133080771172290 ),
 .UNSPECIFIED. ) ;
#3178 = CIRCLE ( 'NONE', #31046, 1.750000000000001554 ) ;
#3179 = VECTOR ( 'NONE', #31098, 1000.000000000000000 ) ;
#3180 = CARTESIAN_POINT ( 'NONE',  ( -14.49999999999999822, 12.98684210526315930, -19.37312575500900280 ) ) ;
#3181 = CARTESIAN_POINT ( 'NONE',  ( 135.0000000000006253, 16.00000000000000000, -54.99999999999999289 ) ) ;
#3182 = VECTOR ( 'NONE', #6227, 1000.000000000000000 ) ;
#3183 = PLANE ( 'NONE',  #12279 ) ;
#3184 = AXIS2_PLACEMENT_3D ( 'NONE', #45627, #5893, #29753 ) ;
#3185 = LINE ( 'NONE', #27833, #40241 ) ;
#3186 = EDGE_CURVE ( 'NONE', #10986, #4748, #46729, .T. ) ;
#3187 = EDGE_LOOP ( 'NONE', ( #16068, #45085, #15128, #42404 ) ) ;
#3188 = AXIS2_PLACEMENT_3D ( 'NONE', #32896, #16223, #832 ) ;
#3189 = CARTESIAN_POINT ( 'NONE',  ( 9.260964247899973856, -13.84230907185609460, -9.683996418299976483 ) ) ;
#3190 = CARTESIAN_POINT ( 'NONE',  ( -7.749480817862350435, -14.85497772329513211, 9.403735324607438884 ) ) ;
#3191 = LINE ( 'NONE', #10905, #28331 ) ;
#3192 = ORIENTED_EDGE ( 'NONE', *, *, #28018, .F. ) ;
#3193 = B_SPLINE_SURFACE_WITH_KNOTS ( 'NONE', 3, 3, ( 
 ( #23239, #15316, #10939, #19654 ),
 ( #15046, #18874, #11210, #50653 ),
 ( #46049, #38414, #11967, #170 ),
 ( #50403, #31219, #39430, #26599 ) ),
 .UNSPECIFIED., .F., .F., .F.,
 ( 4, 4 ),
 ( 4, 4 ),
 ( 0.000000000000000000, 1.000000000000000000 ),
 ( 0.000000000000000000, 1.000000000000000000 ),
 .UNSPECIFIED. ) ;
#3194 = EDGE_CURVE ( 'NONE', #17776, #34175, #42153, .T. ) ;
#3195 = ORIENTED_EDGE ( 'NONE', *, *, #14454, .F. ) ;
#3196 = LINE ( 'NONE', #22215, #30009 ) ;
#3197 = CARTESIAN_POINT ( 'NONE',  ( -1.249999999999999778, 0.000000000000000000, -3.333333333333333481 ) ) ;
#3198 = ORIENTED_EDGE ( 'NONE', *, *, #37933, .T. ) ;
#3199 = ORIENTED_EDGE ( 'NONE', *, *, #8595, .F. ) ;
#3200 = CARTESIAN_POINT ( 'NONE',  ( -10.01251772323708700, 8.486842105263161073, 18.46084505325461578 ) ) ;
#3201 = CARTESIAN_POINT ( 'NONE',  ( 50.00000000000000000, -50.00000000000000000, 800.0000000000000000 ) ) ;
#3202 = CARTESIAN_POINT ( 'NONE',  ( -69.99999999999816680, 17.00000000000000000, 65.00000000000000000 ) ) ;
#3203 = ORIENTED_EDGE ( 'NONE', *, *, #39529, .T. ) ;
#3204 = ORIENTED_EDGE ( 'NONE', *, *, #45592, .F. ) ;
#3205 = ORIENTED_EDGE ( 'NONE', *, *, #50496, .T. ) ;
#3206 = CYLINDRICAL_SURFACE ( 'NONE', #16813, 3.749999999999975575 ) ;
#3207 = CARTESIAN_POINT ( 'NONE',  ( 0.3862712429686810944, 1.188820645368943607, 10.00000000000000000 ) ) ;
#3208 = VECTOR ( 'NONE', #19916, 1000.000000000000000 ) ;
#3209 = DIRECTION ( 'NONE',  ( 0.000000000000000000, 0.000000000000000000, -1.000000000000000000 ) ) ;
#3210 =( BOUNDED_CURVE ( )  B_SPLINE_CURVE ( 3, ( #8952, #28706, #47906, #40510 ),
 .UNSPECIFIED., .F., .F. ) 
 B_SPLINE_CURVE_WITH_KNOTS ( ( 4, 4 ),
 ( 4.712388980384689674, 6.283185307179586232 ),
 .UNSPECIFIED. ) 
 CURVE ( )  GEOMETRIC_REPRESENTATION_ITEM ( )  RATIONAL_B_SPLINE_CURVE ( ( 1.000000000000000000, 0.8047378541243649375, 0.8047378541243649375, 1.000000000000000000 ) ) 
 REPRESENTATION_ITEM ( '' )  );
#3211 = VERTEX_POINT ( 'NONE', #39099 ) ;
#3212 = CIRCLE ( 'NONE', #2433, 1.750000000000001554 ) ;
#3213 = DIRECTION ( 'NONE',  ( -0.000000000000000000, -0.000000000000000000, -1.000000000000000000 ) ) ;
#3214 = CARTESIAN_POINT ( 'NONE',  ( 75.05402655318509630, 2.143131898507880377E-16, -40.93171244307205825 ) ) ;
#3215 = VERTEX_POINT ( 'NONE', #15470 ) ;
#3216 = VERTEX_POINT ( 'NONE', #38337 ) ;
#3217 = DIRECTION ( 'NONE',  ( 0.000000000000000000, 0.000000000000000000, -1.000000000000000000 ) ) ;
#3218 = CIRCLE ( 'NONE', #48246, 50.00000000000000000 ) ;
#3219 = VECTOR ( 'NONE', #30789, 1000.000000000000000 ) ;
#3221 = CARTESIAN_POINT ( 'NONE',  ( 35.00000000000061107, 16.00000000000000000, -30.00000000000000000 ) ) ;
#3220 =( BOUNDED_CURVE ( )  B_SPLINE_CURVE ( 3, ( #11599, #27249, #42874, #7238 ),
 .UNSPECIFIED., .F., .F. ) 
 B_SPLINE_CURVE_WITH_KNOTS ( ( 4, 4 ),
 ( 4.712388980384689674, 6.283185307179586232 ),
 .UNSPECIFIED. ) 
 CURVE ( )  GEOMETRIC_REPRESENTATION_ITEM ( )  RATIONAL_B_SPLINE_CURVE ( ( 1.000000000000000000, 0.8047378541243649375, 0.8047378541243649375, 1.000000000000000000 ) ) 
 REPRESENTATION_ITEM ( '' )  );
#3222 = CARTESIAN_POINT ( 'NONE',  ( 115.0540265531850395, 1.025126265847082108, -37.43171244307203693 ) ) ;
#3223 = ORIENTED_EDGE ( 'NONE', *, *, #41886, .F. ) ;
#3224 = ORIENTED_EDGE ( 'NONE', *, *, #3704, .F. ) ;
#3225 = CARTESIAN_POINT ( 'NONE',  ( 191.5540265531850537, 1.025126265847089657, 119.0682875569279560 ) ) ;
#3226 = FACE_OUTER_BOUND ( 'NONE', #27179, .T. ) ;
#3227 = AXIS2_PLACEMENT_3D ( 'NONE', #2876, #41648, #21639 ) ;
#3228 = CYLINDRICAL_SURFACE ( 'NONE', #4739, 1.750000000000015543 ) ;
#3229 = CARTESIAN_POINT ( 'NONE',  ( -14.99999999999812594, 17.00000000000000000, 90.00000000000000000 ) ) ;
#3230 = ADVANCED_FACE ( 'NONE', ( #19562, #27282 ), #42658, .F. ) ;
#3231 = CARTESIAN_POINT ( 'NONE',  ( -44.94597344681493922, -1.025126265847088991, 159.0682875569279418 ) ) ;
#3232 = ORIENTED_EDGE ( 'NONE', *, *, #33834, .F. ) ;
#3233 = DIRECTION ( 'NONE',  ( 0.000000000000000000, -0.000000000000000000, -1.000000000000000000 ) ) ;
#3234 = ADVANCED_FACE ( 'NONE', ( #15229 ), #22406, .F. ) ;
#3235 = CARTESIAN_POINT ( 'NONE',  ( 181.0000000000000000, -270.5000000000000000, -114.9999999999999147 ) ) ;
#3236 = CARTESIAN_POINT ( 'NONE',  ( -64.99999999999971578, 16.00000000000000000, -60.00000000000000000 ) ) ;
#3237 =( BOUNDED_CURVE ( )  B_SPLINE_CURVE ( 3, ( #23946, #43940, #39608, #32410 ),
 .UNSPECIFIED., .F., .F. ) 
 B_SPLINE_CURVE_WITH_KNOTS ( ( 4, 4 ),
 ( 3.141592653589793116, 4.712388980384689674 ),
 .UNSPECIFIED. ) 
 CURVE ( )  GEOMETRIC_REPRESENTATION_ITEM ( )  RATIONAL_B_SPLINE_CURVE ( ( 1.000000000000000000, 0.8047378541243649375, 0.8047378541243649375, 1.000000000000000000 ) ) 
 REPRESENTATION_ITEM ( '' )  );
#3238 = CARTESIAN_POINT ( 'NONE',  ( -3.245326723439060146, -7.282604692634697230, 0.000000000000000000 ) ) ;
#3239 = EDGE_CURVE ( 'NONE', #16830, #586, #41153, .T. ) ;
#3240 = CARTESIAN_POINT ( 'NONE',  ( 46.76852358249013975, -17.86468378716709537, -9.367992836599954742 ) ) ;
#3241 = EDGE_CURVE ( 'NONE', #43437, #39173, #48510, .T. ) ;
#3242 = FACE_OUTER_BOUND ( 'NONE', #8976, .T. ) ;
#3243 = ORIENTED_EDGE ( 'NONE', *, *, #1225, .F. ) ;
#3244 = CARTESIAN_POINT ( 'NONE',  ( 36.08557433729230723, -35.58569447144768105, 7.455576670931136185 ) ) ;
#3245 = DIRECTION ( 'NONE',  ( -1.000000000000000000, 0.000000000000000000, 0.000000000000000000 ) ) ;
#3246 = VECTOR ( 'NONE', #45655, 1000.000000000000000 ) ;
#3247 = CARTESIAN_POINT ( 'NONE',  ( -84.94597344681494633, 2.143131898507880377E-16, -157.4317124430720582 ) ) ;
#3248 = VERTEX_POINT ( 'NONE', #35005 ) ;
#3249 = CARTESIAN_POINT ( 'NONE',  ( -206.6959734468149463, 0.000000000000000000, 165.0000000000000000 ) ) ;
#3250 = VECTOR ( 'NONE', #31432, 1000.000000000000000 ) ;
#3251 = CYLINDRICAL_SURFACE ( 'NONE', #40962, 2.000000000000001776 ) ;
#3252 = ORIENTED_EDGE ( 'NONE', *, *, #4842, .T. ) ;
#3253 = DIRECTION ( 'NONE',  ( -1.000000000000000000, 0.000000000000000000, -0.000000000000000000 ) ) ;
#3254 = CARTESIAN_POINT ( 'NONE',  ( 3.940019464150765760, 33.28272320232423453, -8.466730184410787174 ) ) ;
#3255 = LINE ( 'NONE', #34087, #25681 ) ;
#3256 = VECTOR ( 'NONE', #17185, 1000.000000000000000 ) ;
#3257 = LINE ( 'NONE', #46079, #10237 ) ;
#3258 = VERTEX_POINT ( 'NONE', #26772 ) ;
#3259 = CARTESIAN_POINT ( 'NONE',  ( -12.16428377685542017, -11.73151505502925929, -9.008049429158100807 ) ) ;
#3260 = ADVANCED_FACE ( 'NONE', ( #18549 ), #7267, .T. ) ;
#3262 = EDGE_LOOP ( 'NONE', ( #6568, #13904, #48658, #8787, #15034, #39005, #20964, #2515 ) ) ;
#3261 = EDGE_CURVE ( 'NONE', #43354, #4645, #14712, .T. ) ;
#3263 = ORIENTED_EDGE ( 'NONE', *, *, #9906, .T. ) ;
#3264 = DIRECTION ( 'NONE',  ( -0.000000000000000000, -0.000000000000000000, -1.000000000000000000 ) ) ;
#3265 = AXIS2_PLACEMENT_3D ( 'NONE', #29791, #37017, #18483 ) ;
#3266 = EDGE_CURVE ( 'NONE', #14624, #46895, #27063, .T. ) ;
#3267 = EDGE_CURVE ( 'NONE', #12079, #14709, #30671, .T. ) ;
#3268 = ORIENTED_EDGE ( 'NONE', *, *, #20803, .F. ) ;
#3269 = CARTESIAN_POINT ( 'NONE',  ( 0.000000000000000000, -168.9999999999999432, -360.0000000000002274 ) ) ;
#3270 = CARTESIAN_POINT ( 'NONE',  ( 194.9999999999999432, -173.0000000000000000, 112.0000000000000284 ) ) ;
#3271 = CARTESIAN_POINT ( 'NONE',  ( 0.1469336902871260508, 1.496274467947966258, 9.953784399990622589 ) ) ;
#3272 = EDGE_CURVE ( 'NONE', #23694, #14722, #50314, .T. ) ;
#3273 = ADVANCED_FACE ( 'NONE', ( #27019 ), #3666, .T. ) ;
#3274 = CARTESIAN_POINT ( 'NONE',  ( 73.30402655318508209, -1.750000000000010658, 80.81828755692798438 ) ) ;
#3275 = ORIENTED_EDGE ( 'NONE', *, *, #12788, .F. ) ;
#3276 = CARTESIAN_POINT ( 'NONE',  ( 74.32915281903215998, 1.750000000000009548, 159.7931612910809065 ) ) ;
#3277 = FACE_OUTER_BOUND ( 'NONE', #48315, .T. ) ;
#3278 = CARTESIAN_POINT ( 'NONE',  ( -8.445973446814964092, 1.025126265847097429, 119.0682875569279133 ) ) ;
#3279 = EDGE_LOOP ( 'NONE', ( #36139, #43467, #26596, #6835 ) ) ;
#3280 = CARTESIAN_POINT ( 'NONE',  ( 0.000000000000000000, 6.912230148066162094, 5.000000000000000000 ) ) ;
#3281 = DIRECTION ( 'NONE',  ( -0.000000000000000000, 0.000000000000000000, 1.000000000000000000 ) ) ;
#3282 = ORIENTED_EDGE ( 'NONE', *, *, #15272, .F. ) ;
#3283 = VERTEX_POINT ( 'NONE', #19316 ) ;
#3284 = VERTEX_POINT ( 'NONE', #26515 ) ;
#3285 = CARTESIAN_POINT ( 'NONE',  ( 27.31081730472575941, 41.96092862852144378, 3.199614146704519602 ) ) ;
#3286 = CARTESIAN_POINT ( 'NONE',  ( 7.359817328027030925, 15.16751262232805431, 2.590526750877053086 ) ) ;
#3287 = ORIENTED_EDGE ( 'NONE', *, *, #49621, .T. ) ;
#3288 = AXIS2_PLACEMENT_3D ( 'NONE', #19939, #8158, #39211 ) ;
#3289 = ADVANCED_FACE ( 'NONE', ( #50573 ), #16493, .T. ) ;
#3290 = AXIS2_PLACEMENT_3D ( 'NONE', #42388, #7253, #38578 ) ;
#3291 = CARTESIAN_POINT ( 'NONE',  ( 0.6440276692615888310, 16.64212148744554298, -9.683996418299976483 ) ) ;
#3292 = CARTESIAN_POINT ( 'NONE',  ( 168.9999999999999716, 165.0000000000000000, -356.0000000000001705 ) ) ;
#3293 = VECTOR ( 'NONE', #13618, 1000.000000000000000 ) ;
#3294 = ADVANCED_FACE ( 'NONE', ( #4692 ), #32393, .T. ) ;
#3295 = CARTESIAN_POINT ( 'NONE',  ( 32.27890028733795447, -1.750000000000010214, -80.20683870891910772 ) ) ;
#3296 = CARTESIAN_POINT ( 'NONE',  ( -86.69597344681494633, -1.750000000000010658, 80.81828755692798438 ) ) ;
#3297 = EDGE_CURVE ( 'NONE', #20901, #15399, #36008, .T. ) ;
#3298 = CARTESIAN_POINT ( 'NONE',  ( 181.0000000000000000, -174.9999999999999716, -344.0000000000001137 ) ) ;
#3299 = CYLINDRICAL_SURFACE ( 'NONE', #39700, 1.750000000000001554 ) ;
#3300 = CARTESIAN_POINT ( 'NONE',  ( -124.9459734468149463, 2.143131898507847836E-16, 79.06828755692798438 ) ) ;
#3301 = CIRCLE ( 'NONE', #17237, 5.000000000000000000 ) ;
#3302 = AXIS2_PLACEMENT_3D ( 'NONE', #7934, #8178, #8688 ) ;
#3303 = CARTESIAN_POINT ( 'NONE',  ( -126.6959734468149321, 0.000000000000000000, 165.0000000000000000 ) ) ;
#3304 = VECTOR ( 'NONE', #28764, 1000.000000000000000 ) ;
#3305 = ORIENTED_EDGE ( 'NONE', *, *, #13985, .T. ) ;
#3306 = DIRECTION ( 'NONE',  ( -0.000000000000000000, -1.000000000000000000, -0.000000000000000000 ) ) ;
#3307 = CARTESIAN_POINT ( 'NONE',  ( -0.7964335060761117413, -1.145363263855212477, 9.955131761384825140 ) ) ;
#3308 = DIRECTION ( 'NONE',  ( -2.958228394578793832E-31, 0.000000000000000000, -1.000000000000000000 ) ) ;
#3309 = CARTESIAN_POINT ( 'NONE',  ( -1.962558162477761714, 3.366505435501197407, 9.741991644046970933 ) ) ;
#3310 = ORIENTED_EDGE ( 'NONE', *, *, #28398, .T. ) ;
#3311 = CARTESIAN_POINT ( 'NONE',  ( -7.721099712662037540, 1.750000000000023315, 121.8434138227750623 ) ) ;
#3312 = EDGE_CURVE ( 'NONE', #2953, #46163, #28291, .T. ) ;
#3313 = DIRECTION ( 'NONE',  ( 1.000000000000000000, 0.000000000000000000, 0.000000000000000000 ) ) ;
#3314 = CARTESIAN_POINT ( 'NONE',  ( -14.76429217231967428, -8.192625680377590314, 9.178419661560148768 ) ) ;
#3315 = FILL_AREA_STYLE_COLOUR ( '', #10702 ) ;
#3316 = ORIENTED_EDGE ( 'NONE', *, *, #27779, .T. ) ;
#3317 = LINE ( 'NONE', #31048, #25609 ) ;
#3318 = VERTEX_POINT ( 'NONE', #16239 ) ;
#3319 = DIRECTION ( 'NONE',  ( 0.000000000000000000, -1.000000000000000000, 0.000000000000000000 ) ) ;
#3320 = EDGE_CURVE ( 'NONE', #16572, #26176, #25634, .T. ) ;
#3321 = ORIENTED_EDGE ( 'NONE', *, *, #10741, .F. ) ;
#3322 = CARTESIAN_POINT ( 'NONE',  ( 343.9999999999999432, -185.0000000000001421, -360.0000000000003411 ) ) ;
#3323 = LINE ( 'NONE', #30801, #43763 ) ;
#3324 = ORIENTED_EDGE ( 'NONE', *, *, #40374, .F. ) ;
#3325 = VERTEX_POINT ( 'NONE', #28541 ) ;
#3326 = EDGE_CURVE ( 'NONE', #4061, #30057, #32145, .T. ) ;
#3327 = VECTOR ( 'NONE', #48289, 1000.000000000000000 ) ;
#3328 = ADVANCED_FACE ( 'NONE', ( #600 ), #8042, .F. ) ;
#3329 = VERTEX_POINT ( 'NONE', #4930 ) ;
#3330 = CARTESIAN_POINT ( 'NONE',  ( 356.0000000000001137, 185.0000000000000284, 349.9999999999998295 ) ) ;
#3331 = CARTESIAN_POINT ( 'NONE',  ( 30.00000000000092726, 17.00000000000000000, -24.99999999999999289 ) ) ;
#3332 = ORIENTED_EDGE ( 'NONE', *, *, #37837, .T. ) ;
#3333 = CARTESIAN_POINT ( 'NONE',  ( -33.16902712922616558, 37.70469005304312304, 1.847720168420772691 ) ) ;
#3334 = CARTESIAN_POINT ( 'NONE',  ( 356.0000000000000000, -174.9999999999999432, 339.9999999999998295 ) ) ;
#3335 = CARTESIAN_POINT ( 'NONE',  ( -45.67084718096785423, 1.750000000000009548, 1.843413822775065825 ) ) ;
#3336 = ORIENTED_EDGE ( 'NONE', *, *, #17142, .F. ) ;
#3337 = EDGE_CURVE ( 'NONE', #31887, #46968, #35500, .T. ) ;
#3338 = B_SPLINE_CURVE_WITH_KNOTS ( 'NONE', 3,
 ( #32918, #38538, #25970, #38291 ),
 .UNSPECIFIED., .F., .F.,
 ( 4, 4 ),
 ( 0.9890644561682322422, 1.000000000000000000 ),
 .UNSPECIFIED. ) ;
#3339 = AXIS2_PLACEMENT_3D ( 'NONE', #47286, #19860, #30933 ) ;
#3340 = ORIENTED_EDGE ( 'NONE', *, *, #13714, .F. ) ;
#3341 = CARTESIAN_POINT ( 'NONE',  ( -87.72109971266203843, -1.750000000000009548, 161.8434138227750907 ) ) ;
#3342 = ADVANCED_FACE ( 'NONE', ( #8800 ), #24451, .T. ) ;
#3343 = LINE ( 'NONE', #25251, #28878 ) ;
#3344 = EDGE_CURVE ( 'NONE', #34855, #45594, #22413, .T. ) ;
#3345 = ORIENTED_EDGE ( 'NONE', *, *, #30501, .F. ) ;
#3346 = CARTESIAN_POINT ( 'NONE',  ( -0.9870575514055066613, -1.980598328282574316, 9.881002359080278907 ) ) ;
#3347 = CARTESIAN_POINT ( 'NONE',  ( 73.30402655318508209, 0.000000000000000000, 165.0000000000000000 ) ) ;
#3348 = ORIENTED_EDGE ( 'NONE', *, *, #27379, .T. ) ;
#3349 = DIRECTION ( 'NONE',  ( 0.000000000000000000, 0.000000000000000000, -1.000000000000000000 ) ) ;
#3350 = ADVANCED_FACE ( 'NONE', ( #36259 ), #8291, .F. ) ;
#3351 = DIRECTION ( 'NONE',  ( 0.000000000000000000, 0.000000000000000000, 1.000000000000000000 ) ) ;
#3352 = EDGE_LOOP ( 'NONE', ( #11966, #12871, #41989, #33452, #15521, #7643 ) ) ;
#3353 = CARTESIAN_POINT ( 'NONE',  ( -2.188678504086925880, 0.3267089737526900350, 9.881002359080270026 ) ) ;
#3354 = CARTESIAN_POINT ( 'NONE',  ( 153.3040265531850537, 0.000000000000000000, 165.0000000000000000 ) ) ;
#3355 = LINE ( 'NONE', #41858, #30385 ) ;
#3356 = CARTESIAN_POINT ( 'NONE',  ( 0.7964335060745958428, 1.145363263855377456, 9.955131761384901523 ) ) ;
#3357 = ORIENTED_EDGE ( 'NONE', *, *, #36236, .F. ) ;
#3358 = CARTESIAN_POINT ( 'NONE',  ( 344.0000000000000568, 165.0000000000000000, 339.9999999999998295 ) ) ;
#3359 = CARTESIAN_POINT ( 'NONE',  ( 0.1469336902871260508, 1.496274467947966258, 9.953784399990622589 ) ) ;
#3360 = FACE_OUTER_BOUND ( 'NONE', #30031, .T. ) ;
#3361 = ORIENTED_EDGE ( 'NONE', *, *, #20811, .T. ) ;
#3363 = ORIENTED_EDGE ( 'NONE', *, *, #4350, .T. ) ;
#3362 = AXIS2_PLACEMENT_3D ( 'NONE', #10601, #19310, #2882 ) ;
#3364 = CARTESIAN_POINT ( 'NONE',  ( 874.9995338190065013, 1090.488709487382948, 2085.870881657164773 ) ) ;
#3365 = CARTESIAN_POINT ( 'NONE',  ( 115.0540265531850395, 2.143131898507847836E-16, 122.5682875569279560 ) ) ;
#3366 = CARTESIAN_POINT ( 'NONE',  ( 168.9999999999999716, -174.9999999999999716, -340.0000000000001137 ) ) ;
#3367 = LINE ( 'NONE', #34699, #44682 ) ;
#3368 = DIRECTION ( 'NONE',  ( 0.000000000000000000, 0.000000000000000000, -1.000000000000000000 ) ) ;
#3369 = CARTESIAN_POINT ( 'NONE',  ( -1.011271242968693862, 0.7347315653655780432, 10.00000000000000000 ) ) ;
#3370 = ORIENTED_EDGE ( 'NONE', *, *, #26185, .F. ) ;
#3371 = CARTESIAN_POINT ( 'NONE',  ( -46.69597344681494633, 1.750000000000010658, -79.18171244307201562 ) ) ;
#3372 = AXIS2_PLACEMENT_3D ( 'NONE', #30630, #11891, #353 ) ;
#3374 = VECTOR ( 'NONE', #29459, 1000.000000000000000 ) ;
#3373 = CARTESIAN_POINT ( 'NONE',  ( -15.62858259096117841, 5.755205073598721910, -9.683996418299976483 ) ) ;
#3375 = CARTESIAN_POINT ( 'NONE',  ( 0.8965959638259385356, 1.582931917743541028, 9.903764339332076005 ) ) ;
#3376 = PLANE ( 'NONE',  #1006 ) ;
#3377 = EDGE_LOOP ( 'NONE', ( #17966, #12196, #20456 ) ) ;
#3378 = CARTESIAN_POINT ( 'NONE',  ( 194.9999999999999432, -172.9999999999999716, 232.0000000000000284 ) ) ;
#3379 = CARTESIAN_POINT ( 'NONE',  ( -0.4611230188129920582, 1.144552435864505835, 9.969907203203804968 ) ) ;
#3380 = VERTEX_POINT ( 'NONE', #31900 ) ;
#3381 = DIRECTION ( 'NONE',  ( -0.000000000000000000, -0.000000000000000000, -1.000000000000000000 ) ) ;
#3382 = LINE ( 'NONE', #11348, #13475 ) ;
#3383 =( BOUNDED_CURVE ( )  B_SPLINE_CURVE ( 3, ( #12038, #22625, #6717, #49769 ),
 .UNSPECIFIED., .F., .F. ) 
 B_SPLINE_CURVE_WITH_KNOTS ( ( 4, 4 ),
 ( 1.570796326794896558, 3.141592653589793116 ),
 .UNSPECIFIED. ) 
 CURVE ( )  GEOMETRIC_REPRESENTATION_ITEM ( )  RATIONAL_B_SPLINE_CURVE ( ( 1.000000000000000000, 0.8047378541243649375, 0.8047378541243649375, 1.000000000000000000 ) ) 
 REPRESENTATION_ITEM ( '' )  );
#3384 = CARTESIAN_POINT ( 'NONE',  ( -46.69597344681494633, 1.750000000000009992, 160.8182875569279702 ) ) ;
#3385 = ORIENTED_EDGE ( 'NONE', *, *, #3061, .T. ) ;
#3386 = EDGE_CURVE ( 'NONE', #37650, #42224, #20834, .T. ) ;
#3387 = FACE_OUTER_BOUND ( 'NONE', #9694, .T. ) ;
#3388 = EDGE_CURVE ( 'NONE', #36127, #23493, #27543, .T. ) ;
#3389 = DIRECTION ( 'NONE',  ( -1.000000000000000000, -0.000000000000000000, -0.000000000000000000 ) ) ;
#3390 = ORIENTED_EDGE ( 'NONE', *, *, #43963, .F. ) ;
#3391 = CARTESIAN_POINT ( 'NONE',  ( 194.3291528190321742, -1.750000000000009326, 159.7931612910809065 ) ) ;
#3392 = LINE ( 'NONE', #30879, #29506 ) ;
#3393 = FACE_OUTER_BOUND ( 'NONE', #43556, .T. ) ;
#3394 = VECTOR ( 'NONE', #6579, 1000.000000000000000 ) ;
#3395 = VERTEX_POINT ( 'NONE', #23681 ) ;
#3396 = EDGE_CURVE ( 'NONE', #19221, #42182, #41183, .T. ) ;
#3397 = ORIENTED_EDGE ( 'NONE', *, *, #26556, .F. ) ;
#3398 = CARTESIAN_POINT ( 'NONE',  ( 194.9999999999999432, -172.9999999999999716, 232.0000000000000284 ) ) ;
#3399 = DIRECTION ( 'NONE',  ( 0.000000000000000000, 0.000000000000000000, -1.000000000000000000 ) ) ;
#3400 = EDGE_CURVE ( 'NONE', #12850, #18090, #27783, .T. ) ;
#3401 = ADVANCED_FACE ( 'NONE', ( #31656 ), #47243, .T. ) ;
#3402 = VERTEX_POINT ( 'NONE', #37281 ) ;
#3403 = ORIENTED_EDGE ( 'NONE', *, *, #36200, .T. ) ;
#3404 = VECTOR ( 'NONE', #1319, 1000.000000000000000 ) ;
#3405 = CARTESIAN_POINT ( 'NONE',  ( 194.3291528190321742, 1.750000000000010214, -120.2068387089191219 ) ) ;
#3406 = CARTESIAN_POINT ( 'NONE',  ( -84.94597344681493212, 1.025126265847089657, -120.9317124430720440 ) ) ;
#3407 = CARTESIAN_POINT ( 'NONE',  ( 35.05402655318504657, 1.025126265847089435, 39.06828755692797728 ) ) ;
#3408 = ORIENTED_EDGE ( 'NONE', *, *, #14245, .F. ) ;
#3409 = DIRECTION ( 'NONE',  ( 0.000000000000000000, 0.000000000000000000, 1.000000000000000000 ) ) ;
#3410 = EDGE_CURVE ( 'NONE', #47482, #16170, #16889, .T. ) ;
#3411 = ORIENTED_EDGE ( 'NONE', *, *, #1446, .F. ) ;
#3412 = DIRECTION ( 'NONE',  ( -0.000000000000000000, -0.000000000000000000, -1.000000000000000000 ) ) ;
#3413 = AXIS2_PLACEMENT_3D ( 'NONE', #19158, #15338, #35105 ) ;
#3414 = CARTESIAN_POINT ( 'NONE',  ( 193.3040265531851105, -1.750000000000010658, 80.81828755692798438 ) ) ;
#3415 = CARTESIAN_POINT ( 'NONE',  ( -22.82242230425432439, -2.816136035261162185, 229.0000000000000000 ) ) ;
#3416 = ORIENTED_EDGE ( 'NONE', *, *, #42506, .T. ) ;
#3417 = ORIENTED_EDGE ( 'NONE', *, *, #44305, .F. ) ;
#3418 = ORIENTED_EDGE ( 'NONE', *, *, #45707, .T. ) ;
#3419 = CARTESIAN_POINT ( 'NONE',  ( -225.0000000000000568, -165.6999999999999602, 250.3600000000000136 ) ) ;
#3420 = DIRECTION ( 'NONE',  ( -1.000000000000000000, 0.000000000000000000, -4.758098658057970186E-16 ) ) ;
#3421 = CARTESIAN_POINT ( 'NONE',  ( 0.3862712429686894766, -1.188820645368940276, 10.00000000000000000 ) ) ;
#3422 = ORIENTED_EDGE ( 'NONE', *, *, #38744, .F. ) ;
#3423 = CARTESIAN_POINT ( 'NONE',  ( 195.0540265531851105, 1.025126265847089435, 39.06828755692797728 ) ) ;
#3424 = ORIENTED_EDGE ( 'NONE', *, *, #3949, .T. ) ;
#3425 = CARTESIAN_POINT ( 'NONE',  ( -6.695973446814940111, 1.750000000000023315, -159.1817124430720298 ) ) ;
#3426 = ORIENTED_EDGE ( 'NONE', *, *, #40442, .T. ) ;
#3427 =( NAMED_UNIT ( * ) PLANE_ANGLE_UNIT ( ) SI_UNIT ( $, .RADIAN. ) );
#3428 = CARTESIAN_POINT ( 'NONE',  ( 181.0000000000003411, 165.0000000000000000, 341.9999999999998863 ) ) ;
#3429 = DIRECTION ( 'NONE',  ( -0.6904757466825005574, 0.7233555441435721711, 0.000000000000000000 ) ) ;
#3430 = FACE_OUTER_BOUND ( 'NONE', #20895, .T. ) ;
#3431 = CARTESIAN_POINT ( 'NONE',  ( 350.0000000000001137, 185.0000000000000284, 343.9999999999997726 ) ) ;
#3432 = ORIENTED_EDGE ( 'NONE', *, *, #40983, .T. ) ;
#3433 = FACE_OUTER_BOUND ( 'NONE', #13573, .T. ) ;
#3434 = EDGE_CURVE ( 'NONE', #27788, #18915, #36228, .T. ) ;
#3435 = CIRCLE ( 'NONE', #32132, 2.000000000000001776 ) ;
#3436 = CARTESIAN_POINT ( 'NONE',  ( 72.27890028733797578, -1.750000000000010214, -118.1565861772249519 ) ) ;
#3437 = FACE_OUTER_BOUND ( 'NONE', #5296, .T. ) ;
#3439 = EDGE_CURVE ( 'NONE', #34800, #16909, #48597, .T. ) ;
#3438 = VECTOR ( 'NONE', #42191, 1000.000000000000000 ) ;
#3440 = LINE ( 'NONE', #23202, #28871 ) ;
#3441 = VECTOR ( 'NONE', #27335, 1000.000000000000000 ) ;
#3442 = LINE ( 'NONE', #3181, #34377 ) ;
#3443 = ORIENTED_EDGE ( 'NONE', *, *, #1572, .T. ) ;
#3444 = CARTESIAN_POINT ( 'NONE',  ( 236.0000000000000000, -169.9999999999999716, 32.29650858650035161 ) ) ;
#3445 = CARTESIAN_POINT ( 'NONE',  ( 356.0000000000000000, 175.0000000000000284, -110.0000000000002132 ) ) ;
#3446 = VERTEX_POINT ( 'NONE', #28795 ) ;
#3447 = DIRECTION ( 'NONE',  ( -0.000000000000000000, -0.000000000000000000, -1.000000000000000000 ) ) ;
#3448 = FACE_OUTER_BOUND ( 'NONE', #48944, .T. ) ;
#3449 = CARTESIAN_POINT ( 'NONE',  ( 359.9999999999999432, -165.0000000000001137, -106.0000000000001990 ) ) ;
#3450 = AXIS2_PLACEMENT_3D ( 'NONE', #20387, #43735, #48303 ) ;
#3451 = EDGE_LOOP ( 'NONE', ( #36840, #5856, #20569, #18117, #14582, #42576, #19182, #46370 ) ) ;
#3452 = VERTEX_POINT ( 'NONE', #25702 ) ;
#3453 = CARTESIAN_POINT ( 'NONE',  ( -175.0000000000000000, 15.00000000000000000, 122.5000000000000142 ) ) ;
#3454 = DIRECTION ( 'NONE',  ( 1.000000000000000000, 0.000000000000000000, 1.612977847700450206E-50 ) ) ;
#3455 = ORIENTED_EDGE ( 'NONE', *, *, #583, .F. ) ;
#3456 = EDGE_LOOP ( 'NONE', ( #18971, #34663, #41921, #30952, #6831 ) ) ;
#3457 = CARTESIAN_POINT ( 'NONE',  ( 45.42829307628542779, 21.98948915213303579, 8.356839323120299312 ) ) ;
#3458 = CARTESIAN_POINT ( 'NONE',  ( -125.6708471809678542, -1.749999999999996225, -158.1565861772249377 ) ) ;
#3459 = LINE ( 'NONE', #30426, #41439 ) ;
#3460 = AXIS2_PLACEMENT_3D ( 'NONE', #21411, #21668, #25271 ) ;
#3461 = ORIENTED_EDGE ( 'NONE', *, *, #26682, .F. ) ;
#3462 = ORIENTED_EDGE ( 'NONE', *, *, #24269, .F. ) ;
#3463 = EDGE_CURVE ( 'NONE', #11684, #2139, #29297, .T. ) ;
#3464 = CIRCLE ( 'NONE', #8400, 0.4999999999999995559 ) ;
#3465 = ORIENTED_EDGE ( 'NONE', *, *, #7771, .T. ) ;
#3466 = AXIS2_PLACEMENT_3D ( 'NONE', #31875, #4666, #47967 ) ;
#3467 = DIRECTION ( 'NONE',  ( 0.000000000000000000, 0.000000000000000000, -1.000000000000000000 ) ) ;
#3468 = CARTESIAN_POINT ( 'NONE',  ( 85.00000000000152056, 17.00000000000000000, 35.00000000000000000 ) ) ;
#3469 = ORIENTED_EDGE ( 'NONE', *, *, #35637, .F. ) ;
#3470 = CARTESIAN_POINT ( 'NONE',  ( 5.542614707656925432, 8.340505786370636443, 6.429802539306464837 ) ) ;
#3471 = VECTOR ( 'NONE', #22284, 1000.000000000000000 ) ;
#3472 = CARTESIAN_POINT ( 'NONE',  ( 155.0540265531850537, 2.143131898507880377E-16, 42.56828755692798438 ) ) ;
#3473 = ORIENTED_EDGE ( 'NONE', *, *, #15794, .T. ) ;
#3474 = ORIENTED_EDGE ( 'NONE', *, *, #22858, .F. ) ;
#3475 = DIRECTION ( 'NONE',  ( 0.000000000000000000, 1.000000000000000000, -1.604368532695312981E-16 ) ) ;
#3476 = ORIENTED_EDGE ( 'NONE', *, *, #18614, .T. ) ;
#3477 = ORIENTED_EDGE ( 'NONE', *, *, #34297, .F. ) ;
#3478 = PLANE ( 'NONE',  #25794 ) ;
#3479 = CARTESIAN_POINT ( 'NONE',  ( 168.9999999999999716, -184.9999999999999716, -342.0000000000001137 ) ) ;
#3480 = CARTESIAN_POINT ( 'NONE',  ( -50.64730461691362962, -42.31198943095992604, 742.8425600500171413 ) ) ;
#3481 = CARTESIAN_POINT ( 'NONE',  ( 129.9999999999999432, 16.00000000000000000, -90.00000000000000000 ) ) ;
#3482 = CARTESIAN_POINT ( 'NONE',  ( 356.0000000000001137, 185.0000000000000284, 359.9999999999998295 ) ) ;
#3483 = CYLINDRICAL_SURFACE ( 'NONE', #20815, 1.750000000000015543 ) ;
#3484 = EDGE_LOOP ( 'NONE', ( #30437, #29593, #4566 ) ) ;
#3485 = DIRECTION ( 'NONE',  ( -1.000000000000000000, -0.000000000000000000, -0.000000000000000000 ) ) ;
#3486 = CARTESIAN_POINT ( 'NONE',  ( 191.5540265531850537, -1.025126265847089213, -160.9317124430720014 ) ) ;
#3487 = VECTOR ( 'NONE', #47496, 1000.000000000000000 ) ;
#3488 = CYLINDRICAL_SURFACE ( 'NONE', #46067, 1.750000000000010214 ) ;
#3489 = CARTESIAN_POINT ( 'NONE',  ( 151.5540265531850537, -1.025126265847089657, -37.43171244307202272 ) ) ;
#3490 = EDGE_CURVE ( 'NONE', #11094, #28407, #10304, .T. ) ;
#3491 = CARTESIAN_POINT ( 'NONE',  ( 47.88254548617766204, -14.43607691413525984, -3.760136334089591248 ) ) ;
#3492 = CARTESIAN_POINT ( 'NONE',  ( -124.9459734468149321, 1.025126265847081886, -120.9317124430720440 ) ) ;
#3493 = ORIENTED_EDGE ( 'NONE', *, *, #41058, .F. ) ;
#3494 = CARTESIAN_POINT ( 'NONE',  ( 1.011271242968677653, 0.7347315653656002477, -10.00000000000000000 ) ) ;
#3495 = VECTOR ( 'NONE', #2298, 1000.000000000000000 ) ;
#3496 = CARTESIAN_POINT ( 'NONE',  ( 0.000000000000000000, 169.0000000000000000, 343.9999999999997726 ) ) ;
#3497 = CARTESIAN_POINT ( 'NONE',  ( 1.655785408456140084, 0.7536129375913136474, 9.903764339332061795 ) ) ;
#3498 = COLOUR_RGB ( '',0.7921568627450980005, 0.8196078431372548767, 0.9333333333333333481 ) ;
#3499 = ORIENTED_EDGE ( 'NONE', *, *, #25092, .F. ) ;
#3500 = DIRECTION ( 'NONE',  ( 0.000000000000000000, -1.000000000000000000, 0.000000000000000000 ) ) ;
#3501 = VECTOR ( 'NONE', #35907, 1000.000000000000000 ) ;
#3502 = DIRECTION ( 'NONE',  ( 0.000000000000000000, 0.000000000000000000, 1.000000000000000000 ) ) ;
#3503 = ORIENTED_EDGE ( 'NONE', *, *, #39131, .T. ) ;
#3504 = CARTESIAN_POINT ( 'NONE',  ( 2.500000000000000444, 224.9999999999999716, -240.0000000000000000 ) ) ;
#3505 = DIRECTION ( 'NONE',  ( -1.000000000000000000, 0.000000000000000000, -0.000000000000000000 ) ) ;
#3506 = DIRECTION ( 'NONE',  ( -0.000000000000000000, -1.000000000000000000, -0.000000000000000000 ) ) ;
#3507 = LINE ( 'NONE', #30472, #28266 ) ;
#3508 = ORIENTED_EDGE ( 'NONE', *, *, #43790, .F. ) ;
#3509 = DIRECTION ( 'NONE',  ( -1.156482317317870492E-16, 1.000000000000000000, 0.000000000000000000 ) ) ;
#3510 = B_SPLINE_SURFACE_WITH_KNOTS ( 'NONE', 3, 3, ( 
 ( #20658, #24276, #36335, #35840 ),
 ( #8616, #28605, #20398, #44244 ),
 ( #9363, #25267, #9117, #5762 ),
 ( #40918, #24776, #12453, #28114 ) ),
 .UNSPECIFIED., .F., .F., .F.,
 ( 4, 4 ),
 ( 4, 4 ),
 ( 0.000000000000000000, 1.000000000000000000 ),
 ( 0.000000000000000000, 1.000000000000000000 ),
 .UNSPECIFIED. ) ;
#3511 = ORIENTED_EDGE ( 'NONE', *, *, #33199, .T. ) ;
#3513 = ORIENTED_EDGE ( 'NONE', *, *, #2083, .F. ) ;
#3512 = B_SPLINE_CURVE_WITH_KNOTS ( 'NONE', 3,
 ( #7569, #47780, #43465, #4726 ),
 .UNSPECIFIED., .F., .F.,
 ( 4, 4 ),
 ( 0.000000000000000000, 0.2637263876330691592 ),
 .UNSPECIFIED. ) ;
#3514 = CARTESIAN_POINT ( 'NONE',  ( 210.0000000000000568, 0.000000000000000000, -117.4317124430720298 ) ) ;
#3515 =( BOUNDED_CURVE ( )  B_SPLINE_CURVE ( 3, ( #39533, #4371, #3341, #35694 ),
 .UNSPECIFIED., .F., .F. ) 
 B_SPLINE_CURVE_WITH_KNOTS ( ( 4, 4 ),
 ( 0.000000000000000000, 1.570796326794896558 ),
 .UNSPECIFIED. ) 
 CURVE ( )  GEOMETRIC_REPRESENTATION_ITEM ( )  RATIONAL_B_SPLINE_CURVE ( ( 1.000000000000000000, 0.8047378541243649375, 0.8047378541243649375, 1.000000000000000000 ) ) 
 REPRESENTATION_ITEM ( '' )  );
#3516 = ORIENTED_EDGE ( 'NONE', *, *, #41546, .T. ) ;
#3517 = CARTESIAN_POINT ( 'NONE',  ( -65.00000000000002842, 17.00000000000000000, -114.9999999999999858 ) ) ;
#3518 = FACE_OUTER_BOUND ( 'NONE', #45969, .T. ) ;
#3519 = DIRECTION ( 'NONE',  ( -1.586032892321652236E-16, -1.000000000000000000, -6.853681917100419162E-49 ) ) ;
#3520 = EDGE_CURVE ( 'NONE', #19871, #11669, #41598, .T. ) ;
#3521 =( BOUNDED_CURVE ( )  B_SPLINE_CURVE ( 3, ( #42759, #49673, #26109, #26627 ),
 .UNSPECIFIED., .F., .F. ) 
 B_SPLINE_CURVE_WITH_KNOTS ( ( 4, 4 ),
 ( 3.141592653589793116, 4.712388980384689674 ),
 .UNSPECIFIED. ) 
 CURVE ( )  GEOMETRIC_REPRESENTATION_ITEM ( )  RATIONAL_B_SPLINE_CURVE ( ( 1.000000000000000000, 0.8047378541243649375, 0.8047378541243649375, 1.000000000000000000 ) ) 
 REPRESENTATION_ITEM ( '' )  );
#3522 = ORIENTED_EDGE ( 'NONE', *, *, #40149, .F. ) ;
#3523 = EDGE_CURVE ( 'NONE', #18198, #23745, #13414, .T. ) ;
#3524 = CARTESIAN_POINT ( 'NONE',  ( 193.3040265531851105, -1.750000000000010658, -79.18171244307201562 ) ) ;
#3525 = DIRECTION ( 'NONE',  ( -1.000000000000000000, 0.000000000000000000, -2.958228394578794270E-31 ) ) ;
#3526 = EDGE_CURVE ( 'NONE', #33292, #50656, #50146, .T. ) ;
#3527 = DIRECTION ( 'NONE',  ( 0.000000000000000000, 0.000000000000000000, 1.000000000000000000 ) ) ;
#3528 = ORIENTED_EDGE ( 'NONE', *, *, #11798, .T. ) ;
#3529 = CARTESIAN_POINT ( 'NONE',  ( 0.000000000000000000, 17.00000000000000000, 0.000000000000000000 ) ) ;
#3530 = DIRECTION ( 'NONE',  ( -1.000000000000000000, -0.000000000000000000, -0.000000000000000000 ) ) ;
#3531 = ORIENTED_EDGE ( 'NONE', *, *, #18390, .T. ) ;
#3532 = EDGE_LOOP ( 'NONE', ( #13431, #22172, #30047, #39452 ) ) ;
#3533 = ORIENTED_EDGE ( 'NONE', *, *, #48129, .F. ) ;
#3534 = CARTESIAN_POINT ( 'NONE',  ( 85.00000000000213163, 17.00000000000000000, 115.0000000000000142 ) ) ;
#3535 = VECTOR ( 'NONE', #183, 1000.000000000000000 ) ;
#3536 = EDGE_CURVE ( 'NONE', #24944, #35881, #21519, .T. ) ;
#3537 = EDGE_CURVE ( 'NONE', #25776, #3827, #22096, .T. ) ;
#3538 =( BOUNDED_CURVE ( )  B_SPLINE_CURVE ( 3, ( #19582, #31148, #31407, #7805 ),
 .UNSPECIFIED., .F., .F. ) 
 B_SPLINE_CURVE_WITH_KNOTS ( ( 4, 4 ),
 ( 0.000000000000000000, 1.570796326794896558 ),
 .UNSPECIFIED. ) 
 CURVE ( )  GEOMETRIC_REPRESENTATION_ITEM ( )  RATIONAL_B_SPLINE_CURVE ( ( 1.000000000000000000, 0.8047378541243649375, 0.8047378541243649375, 1.000000000000000000 ) ) 
 REPRESENTATION_ITEM ( '' )  );
#3539 = CARTESIAN_POINT ( 'NONE',  ( 155.0540265531850537, 2.143131898507880377E-16, 2.568287556927978166 ) ) ;
#3540 = ORIENTED_EDGE ( 'NONE', *, *, #31994, .T. ) ;
#3541 = LINE ( 'NONE', #46871, #45418 ) ;
#3542 =( LENGTH_UNIT ( ) NAMED_UNIT ( * ) SI_UNIT ( .MILLI., .METRE. ) );
#3543 = EDGE_CURVE ( 'NONE', #45635, #31056, #2421, .T. ) ;
#3544 = LINE ( 'NONE', #34121, #37892 ) ;
#3545 = CARTESIAN_POINT ( 'NONE',  ( 0.2401930789657907572, 1.414287202658143894, 9.950105812514292936 ) ) ;
#3546 = CARTESIAN_POINT ( 'NONE',  ( -48.44597344681495343, 0.000000000000000000, 42.56828755692798438 ) ) ;
#3547 = CIRCLE ( 'NONE', #37977, 4.000000000000003553 ) ;
#3548 = CARTESIAN_POINT ( 'NONE',  ( 115.0540265531850395, 2.143131898507847836E-16, 165.0000000000000000 ) ) ;
#3549 = CARTESIAN_POINT ( 'NONE',  ( -6.695973446814940111, 0.000000000000000000, 165.0000000000000000 ) ) ;
#3550 = CARTESIAN_POINT ( 'NONE',  ( -15.00000000000001421, 17.00000000000000000, -114.9999999999999858 ) ) ;
#3551 = CARTESIAN_POINT ( 'NONE',  ( 0.000000000000000000, 184.8000000000000114, 359.7999999999997840 ) ) ;
#3552 = LINE ( 'NONE', #2549, #4333 ) ;
#3553 = EDGE_CURVE ( 'NONE', #20088, #22621, #48242, .T. ) ;
#3554 = EDGE_CURVE ( 'NONE', #48314, #3283, #8429, .T. ) ;
#3555 = ORIENTED_EDGE ( 'NONE', *, *, #23846, .F. ) ;
#3556 = CARTESIAN_POINT ( 'NONE',  ( 194.9999999999999432, 164.9999999999999716, 231.9999999999999716 ) ) ;
#3557 = CARTESIAN_POINT ( 'NONE',  ( -124.9459734468149321, 1.025126265847082108, 42.56828755692797017 ) ) ;
#3558 = EDGE_CURVE ( 'NONE', #9513, #48877, #13873, .T. ) ;
#3559 = ADVANCED_FACE ( 'NONE', ( #40598 ), #5433, .T. ) ;
#3560 = AXIS2_PLACEMENT_3D ( 'NONE', #19131, #50398, #50133 ) ;
#3561 = CARTESIAN_POINT ( 'NONE',  ( -3.886636751349460628, 37.33392444503267171, 6.057468652304066836 ) ) ;
#3562 = DIRECTION ( 'NONE',  ( 0.000000000000000000, -0.000000000000000000, -1.000000000000000000 ) ) ;
#3563 = ORIENTED_EDGE ( 'NONE', *, *, #11111, .F. ) ;
#3564 = ADVANCED_FACE ( 'NONE', ( #32910 ), #1849, .T. ) ;
#3565 = DIRECTION ( 'NONE',  ( -0.000000000000000000, -0.000000000000000000, 1.000000000000000000 ) ) ;
#3566 = CARTESIAN_POINT ( 'NONE',  ( -6.695973446814940111, 0.000000000000000000, 165.0000000000000000 ) ) ;
#3567 = EDGE_CURVE ( 'NONE', #3732, #45897, #46674, .T. ) ;
#3568 = CARTESIAN_POINT ( 'NONE',  ( 168.9999999999999716, -166.9999999999999432, -350.0000000000001705 ) ) ;
#3569 = DIRECTION ( 'NONE',  ( -0.000000000000000000, -1.000000000000000000, -0.000000000000000000 ) ) ;
#3570 = CARTESIAN_POINT ( 'NONE',  ( 14.29087950072012170, 9.652079258044652832, 8.727788335465566760 ) ) ;
#3571 = ORIENTED_EDGE ( 'NONE', *, *, #46563, .T. ) ;
#3572 = VERTEX_POINT ( 'NONE', #34941 ) ;
#3573 = CARTESIAN_POINT ( 'NONE',  ( 49.67735855322978011, -8.912210285361751971, 8.356839323120299312 ) ) ;
#3574 = AXIS2_PLACEMENT_3D ( 'NONE', #44094, #9714, #41025 ) ;
#3575 = ORIENTED_EDGE ( 'NONE', *, *, #33987, .T. ) ;
#3576 = DIRECTION ( 'NONE',  ( 0.000000000000000000, 0.000000000000000000, 1.000000000000000000 ) ) ;
#3577 = AXIS2_PLACEMENT_3D ( 'NONE', #25346, #33059, #13534 ) ;
#3578 = FACE_OUTER_BOUND ( 'NONE', #13186, .T. ) ;
#3579 = VERTEX_POINT ( 'NONE', #19246 ) ;
#3580 = CARTESIAN_POINT ( 'NONE',  ( 195.0540265531851105, 2.143131898507880377E-16, 165.0000000000000000 ) ) ;
#3581 = EDGE_CURVE ( 'NONE', #12455, #37995, #22343, .T. ) ;
#3582 = ORIENTED_EDGE ( 'NONE', *, *, #24464, .F. ) ;
#3583 = VECTOR ( 'NONE', #39264, 1000.000000000000000 ) ;
#3584 = VECTOR ( 'NONE', #7170, 1000.000000000000000 ) ;
#3585 = EDGE_CURVE ( 'NONE', #47178, #12755, #26452, .T. ) ;
#3586 = EDGE_CURVE ( 'NONE', #26037, #16958, #48900, .T. ) ;
#3587 = VERTEX_POINT ( 'NONE', #6955 ) ;
#3588 = FACE_OUTER_BOUND ( 'NONE', #35618, .T. ) ;
#3589 = CYLINDRICAL_SURFACE ( 'NONE', #14230, 1.750000000000008438 ) ;
#3590 = ORIENTED_EDGE ( 'NONE', *, *, #24246, .T. ) ;
#3591 = CARTESIAN_POINT ( 'NONE',  ( 0.8285222815141930486, 1.889008401827334094, 9.886433018048068178 ) ) ;
#3592 = CARTESIAN_POINT ( 'NONE',  ( 194.9999999999999432, -173.0000000000000000, 352.0000000000000568 ) ) ;
#3593 = ADVANCED_FACE ( 'NONE', ( #38284 ), #14649, .T. ) ;
#3594 = CARTESIAN_POINT ( 'NONE',  ( 210.0000000000000568, 0.000000000000000000, -119.1817124430720440 ) ) ;
#3595 = ORIENTED_EDGE ( 'NONE', *, *, #9327, .F. ) ;
#3596 = ORIENTED_EDGE ( 'NONE', *, *, #40000, .F. ) ;
#3597 = CARTESIAN_POINT ( 'NONE',  ( -32.92553608936650988, -17.96298651181783868, 8.100132398494512387 ) ) ;
#3598 = EDGE_CURVE ( 'NONE', #8209, #33697, #26206, .T. ) ;
#3599 = CARTESIAN_POINT ( 'NONE',  ( 30.00000000000092726, 17.00000000000000000, 0.000000000000000000 ) ) ;
#3600 = AXIS2_PLACEMENT_3D ( 'NONE', #9631, #36347, #24788 ) ;
#3601 = ORIENTED_EDGE ( 'NONE', *, *, #19583, .F. ) ;
#3602 = CARTESIAN_POINT ( 'NONE',  ( -165.6708471809677974, 1.750000000000009548, -38.15658617722494483 ) ) ;
#3603 = CARTESIAN_POINT ( 'NONE',  ( 181.0000000000000000, 175.0000000000000284, -344.0000000000001137 ) ) ;
#3604 = ORIENTED_EDGE ( 'NONE', *, *, #46511, .T. ) ;
#3605 = CARTESIAN_POINT ( 'NONE',  ( 1.424123654779712922, 0.3625862473308184009, 9.958264684458541183 ) ) ;
#3606 = CARTESIAN_POINT ( 'NONE',  ( 85.00000000000090949, 17.00000000000000000, -24.99999999999999289 ) ) ;
#3607 = EDGE_LOOP ( 'NONE', ( #34537, #18552, #35865, #36207 ) ) ;
#3608 = EDGE_CURVE ( 'NONE', #50186, #2282, #22597, .T. ) ;
#3609 = CARTESIAN_POINT ( 'NONE',  ( 339.9999999999999432, 169.0000000000000000, -342.0000000000001705 ) ) ;
#3610 = CARTESIAN_POINT ( 'NONE',  ( 0.000000000000000000, 17.00000000000000000, 0.000000000000000000 ) ) ;
#3611 = DIRECTION ( 'NONE',  ( 0.000000000000000000, 0.000000000000000000, 1.000000000000000000 ) ) ;
#3612 = CARTESIAN_POINT ( 'NONE',  ( 0.000000000000000000, -175.0000000000000284, -350.0000000000002274 ) ) ;
#3613 = VECTOR ( 'NONE', #42083, 1000.000000000000000 ) ;
#3614 = ORIENTED_EDGE ( 'NONE', *, *, #6119, .F. ) ;
#3615 = VECTOR ( 'NONE', #15292, 1000.000000000000000 ) ;
#3616 = EDGE_CURVE ( 'NONE', #39284, #48491, #15415, .T. ) ;
#3617 = CARTESIAN_POINT ( 'NONE',  ( -1.642172164747307761, 0.000000000000000000, 27.58190990837850265 ) ) ;
#3618 = CARTESIAN_POINT ( 'NONE',  ( 113.3040265531850537, -1.749999999999996891, 0.8182875569279768335 ) ) ;
#3619 = VECTOR ( 'NONE', #26495, 1000.000000000000000 ) ;
#3620 = CARTESIAN_POINT ( 'NONE',  ( 29.39982726364966581, 16.78152490921169360, 8.356839323120299312 ) ) ;
#3621 = EDGE_LOOP ( 'NONE', ( #43249, #780, #29487, #20056 ) ) ;
#3622 = AXIS2_PLACEMENT_3D ( 'NONE', #24895, #36459, #1300 ) ;
#3623 = VERTEX_POINT ( 'NONE', #2835 ) ;
#3624 = CARTESIAN_POINT ( 'NONE',  ( 867.4995338190028633, 1578.153237050701591, 1561.986414963432253 ) ) ;
#3625 = CARTESIAN_POINT ( 'NONE',  ( 33.30402655318503946, -1.750000000000010214, 40.81828755692798438 ) ) ;
#3626 = CARTESIAN_POINT ( 'NONE',  ( 5.551115123125782702E-14, -168.9999999999999432, 339.9999999999997726 ) ) ;
#3627 = ADVANCED_FACE ( 'NONE', ( #34421 ), #3092, .F. ) ;
#3628 = EDGE_CURVE ( 'NONE', #35494, #45431, #34342, .T. ) ;
#3629 = SURFACE_SIDE_STYLE ('',( #42370 ) ) ;
#3630 = DIRECTION ( 'NONE',  ( -0.000000000000000000, -1.000000000000000000, -0.000000000000000000 ) ) ;
#3631 = CARTESIAN_POINT ( 'NONE',  ( 33.30402655318503946, 1.750000000000010214, -39.18171244307202983 ) ) ;
#3632 = ORIENTED_EDGE ( 'NONE', *, *, #6372, .T. ) ;
#3633 = EDGE_CURVE ( 'NONE', #31313, #449, #4866, .T. ) ;
#3634 = DIRECTION ( 'NONE',  ( 0.000000000000000000, 0.000000000000000000, 1.000000000000000000 ) ) ;
#3635 = EDGE_CURVE ( 'NONE', #21418, #28177, #4441, .T. ) ;
#3636 = PRODUCT_DEFINITION_SHAPE ( 'NONE', 'NONE',  #50726 ) ;
#3637 = DIRECTION ( 'NONE',  ( -0.000000000000000000, -0.000000000000000000, -1.000000000000000000 ) ) ;
#3638 = DIRECTION ( 'NONE',  ( -0.000000000000000000, -0.000000000000000000, -1.000000000000000000 ) ) ;
#3639 = CARTESIAN_POINT ( 'NONE',  ( 42.51732812238058301, -47.49695244670218131, -5.000000000000000000 ) ) ;
#3640 = ADVANCED_FACE ( 'NONE', ( #14399 ), #34678, .F. ) ;
#3641 = AXIS2_PLACEMENT_3D ( 'NONE', #40376, #16766, #8571 ) ;
#3642 = CARTESIAN_POINT ( 'NONE',  ( -4.999999999999997335, 204.9999999999999716, -234.7500000000000000 ) ) ;
#3643 = VERTEX_POINT ( 'NONE', #11055 ) ;
#3644 = CARTESIAN_POINT ( 'NONE',  ( -10.00000000000000533, -0.04986450829243618821, 8.654293224463934564 ) ) ;
#3645 = DIRECTION ( 'NONE',  ( 0.000000000000000000, 2.537652627714642000E-15, 1.000000000000000000 ) ) ;
#3646 = ORIENTED_EDGE ( 'NONE', *, *, #43668, .F. ) ;
#3647 = DIRECTION ( 'NONE',  ( -1.000000000000000000, 0.000000000000000000, 0.000000000000000000 ) ) ;
#3648 = DIRECTION ( 'NONE',  ( 1.860490536778032451E-50, 0.000000000000000000, -1.000000000000000000 ) ) ;
#3649 = CARTESIAN_POINT ( 'NONE',  ( 114.3291528190321173, 1.749999999999996669, -0.2068387089191042749 ) ) ;
#3650 = ORIENTED_EDGE ( 'NONE', *, *, #46157, .T. ) ;
#3651 = DIRECTION ( 'NONE',  ( -1.000000000000000000, -0.000000000000000000, -0.000000000000000000 ) ) ;
#3652 = ADVANCED_FACE ( 'NONE', ( #30064 ), #10795, .T. ) ;
#3653 = DIRECTION ( 'NONE',  ( -1.000000000000000000, 0.000000000000000000, 0.000000000000000000 ) ) ;
#3654 = ORIENTED_EDGE ( 'NONE', *, *, #8260, .T. ) ;
#3655 = CARTESIAN_POINT ( 'NONE',  ( 343.9999999999998863, -165.0000000000001137, -110.0000000000002132 ) ) ;
#3656 = VECTOR ( 'NONE', #11629, 1000.000000000000000 ) ;
#3657 = LINE ( 'NONE', #27273, #9833 ) ;
#3658 = VERTEX_POINT ( 'NONE', #49502 ) ;
#3659 = ORIENTED_EDGE ( 'NONE', *, *, #49978, .F. ) ;
#3660 = CARTESIAN_POINT ( 'NONE',  ( 5.551115123125782702E-14, -168.9999999999999432, 339.9999999999997726 ) ) ;
#3661 = VECTOR ( 'NONE', #29191, 1000.000000000000000 ) ;
#3662 = FACE_OUTER_BOUND ( 'NONE', #50102, .T. ) ;
#3663 = ORIENTED_EDGE ( 'NONE', *, *, #7740, .F. ) ;
#3664 = ORIENTED_EDGE ( 'NONE', *, *, #13355, .T. ) ;
#3665 = CARTESIAN_POINT ( 'NONE',  ( -85.67084718096784002, 1.750000000000010214, -120.2068387089191219 ) ) ;
#3666 = CYLINDRICAL_SURFACE ( 'NONE', #23948, 1.750000000000010214 ) ;
#3667 = ORIENTED_EDGE ( 'NONE', *, *, #20668, .T. ) ;
#3668 = LINE ( 'NONE', #31659, #25168 ) ;
#3669 = ORIENTED_EDGE ( 'NONE', *, *, #30323, .F. ) ;
#3670 = EDGE_CURVE ( 'NONE', #47848, #29172, #854, .T. ) ;
#3671 = DIRECTION ( 'NONE',  ( 0.000000000000000000, 0.000000000000000000, 1.000000000000000000 ) ) ;
#3672 = CARTESIAN_POINT ( 'NONE',  ( -84.94597344681494633, 2.143131898507880377E-16, 79.06828755692797017 ) ) ;
#3673 = CARTESIAN_POINT ( 'NONE',  ( 130.0000000000021032, 16.00000000000000000, 95.00000000000000000 ) ) ;
#3674 = ORIENTED_EDGE ( 'NONE', *, *, #36613, .T. ) ;
#3675 = ORIENTED_EDGE ( 'NONE', *, *, #19025, .F. ) ;
#3676 = ORIENTED_EDGE ( 'NONE', *, *, #44948, .F. ) ;
#3677 = AXIS2_PLACEMENT_3D ( 'NONE', #31623, #43385, #23902 ) ;
#3678 = FACE_OUTER_BOUND ( 'NONE', #38951, .T. ) ;
#3679 = B_SPLINE_CURVE_WITH_KNOTS ( 'NONE', 3,
 ( #22815, #30271, #6654, #2802 ),
 .UNSPECIFIED., .F., .F.,
 ( 4, 4 ),
 ( 0.000000000000000000, 0.002368422649471299893 ),
 .UNSPECIFIED. ) ;
#3680 = CARTESIAN_POINT ( 'NONE',  ( -65.00000000000002842, 16.00000000000000000, -90.00000000000000000 ) ) ;
#3681 = LINE ( 'NONE', #23699, #15884 ) ;
#3682 = ORIENTED_EDGE ( 'NONE', *, *, #40758, .T. ) ;
#3683 = CARTESIAN_POINT ( 'NONE',  ( -65.00000000000002842, 16.00000000000000000, -90.00000000000000000 ) ) ;
#3684 = ORIENTED_EDGE ( 'NONE', *, *, #43166, .T. ) ;
#3685 = CARTESIAN_POINT ( 'NONE',  ( -164.9459734468149463, 2.143131898507880377E-16, 42.56828755692798438 ) ) ;
#3686 = EDGE_LOOP ( 'NONE', ( #31338, #48065, #22159, #18658, #11705, #26828 ) ) ;
#3687 = CARTESIAN_POINT ( 'NONE',  ( 350.0000000000000000, 181.0000000000000284, -342.0000000000001705 ) ) ;
#3688 = DIRECTION ( 'NONE',  ( -1.000000000000000000, 0.000000000000000000, 1.586032892321651989E-16 ) ) ;
#3689 = CARTESIAN_POINT ( 'NONE',  ( -84.94597344681493212, -1.025126265847089657, 119.0682875569279560 ) ) ;
#3690 = CARTESIAN_POINT ( 'NONE',  ( 2.500000000000001776, 214.9999999999999716, -234.7500000000000000 ) ) ;
#3691 = EDGE_CURVE ( 'NONE', #24521, #30113, #20524, .T. ) ;
#3692 = EDGE_CURVE ( 'NONE', #22226, #28031, #43117, .T. ) ;
#3693 = VECTOR ( 'NONE', #4074, 1000.000000000000000 ) ;
#3694 = CARTESIAN_POINT ( 'NONE',  ( 4.999999999999999112, -175.0000000000000284, 346.2500000000002274 ) ) ;
#3695 = ORIENTED_EDGE ( 'NONE', *, *, #39267, .F. ) ;
#3696 = ORIENTED_EDGE ( 'NONE', *, *, #21537, .F. ) ;
#3697 = CARTESIAN_POINT ( 'NONE',  ( 153.3040265531850537, 1.750000000000009992, -159.1817124430720298 ) ) ;
#3698 = CARTESIAN_POINT ( 'NONE',  ( -86.69597344681494633, -1.750000000000010658, -79.18171244307201562 ) ) ;
#3699 =( BOUNDED_CURVE ( )  B_SPLINE_CURVE ( 3, ( #37582, #49057, #40664, #36831 ),
 .UNSPECIFIED., .F., .F. ) 
 B_SPLINE_CURVE_WITH_KNOTS ( ( 4, 4 ),
 ( 4.712388980384689674, 6.283185307179586232 ),
 .UNSPECIFIED. ) 
 CURVE ( )  GEOMETRIC_REPRESENTATION_ITEM ( )  RATIONAL_B_SPLINE_CURVE ( ( 1.000000000000000000, 0.8047378541243649375, 0.8047378541243649375, 1.000000000000000000 ) ) 
 REPRESENTATION_ITEM ( '' )  );
#3700 = EDGE_CURVE ( 'NONE', #40759, #18948, #23685, .T. ) ;
#3701 = DIRECTION ( 'NONE',  ( 1.000000000000000000, 0.000000000000000000, -0.000000000000000000 ) ) ;
#3702 = CARTESIAN_POINT ( 'NONE',  ( 183.0000000000000000, -272.4999999999999432, -356.0000000000001705 ) ) ;
#3703 = AXIS2_PLACEMENT_3D ( 'NONE', #32046, #36923, #37171 ) ;
#3704 = EDGE_CURVE ( 'NONE', #40138, #34589, #22121, .T. ) ;
#3705 = ADVANCED_FACE ( 'NONE', ( #44107 ), #35442, .F. ) ;
#3706 = PLANE ( 'NONE',  #4301 ) ;
#3707 = CARTESIAN_POINT ( 'NONE',  ( 350.0000000000001137, 169.0000000000000000, 355.9999999999997726 ) ) ;
#3708 = ORIENTED_EDGE ( 'NONE', *, *, #5550, .T. ) ;
#3709 = LINE ( 'NONE', #27584, #4912 ) ;
#3710 = ADVANCED_FACE ( 'NONE', ( #31593 ), #47674, .T. ) ;
#3711 = CARTESIAN_POINT ( 'NONE',  ( 164.9999999999999716, 16.00000000000000000, 65.00000000000000000 ) ) ;
#3712 = ORIENTED_EDGE ( 'NONE', *, *, #33824, .F. ) ;
#3713 = VECTOR ( 'NONE', #5926, 1000.000000000000000 ) ;
#3714 = B_SPLINE_CURVE_WITH_KNOTS ( 'NONE', 3,
 ( #5288, #43778, #8651, #24307, #952, #16591 ),
 .UNSPECIFIED., .F., .F.,
 ( 4, 2, 4 ),
 ( 8.673617379884035472E-19, 0.009882509389272365469, 0.01976501877854472747 ),
 .UNSPECIFIED. ) ;
#3715 = CARTESIAN_POINT ( 'NONE',  ( 36.08557433729230723, -35.58569447144768105, 7.455576670931136185 ) ) ;
#3716 = LINE ( 'NONE', #43470, #31128 ) ;
#3717 = DIRECTION ( 'NONE',  ( 0.000000000000000000, 2.537652627714642000E-15, 1.000000000000000000 ) ) ;
#3718 = VECTOR ( 'NONE', #10070, 1000.000000000000000 ) ;
#3719 = VERTEX_POINT ( 'NONE', #16670 ) ;
#3720 = ORIENTED_EDGE ( 'NONE', *, *, #43078, .T. ) ;
#3721 = CARTESIAN_POINT ( 'NONE',  ( 181.0000000000000000, 8.000000000000062172, -340.0000000000001137 ) ) ;
#3722 = CARTESIAN_POINT ( 'NONE',  ( 8.277096487746778308, -50.00000000000000711, 7.455576670931136185 ) ) ;
#3723 = AXIS2_PLACEMENT_3D ( 'NONE', #10567, #45186, #2371 ) ;
#3724 = ORIENTED_EDGE ( 'NONE', *, *, #40212, .F. ) ;
#3725 = VERTEX_POINT ( 'NONE', #8741 ) ;
#3726 = DIRECTION ( 'NONE',  ( -1.000000000000000000, -0.000000000000000000, -0.000000000000000000 ) ) ;
#3727 = DIRECTION ( 'NONE',  ( -0.000000000000000000, -0.000000000000000000, -1.000000000000000000 ) ) ;
#3728 = DIRECTION ( 'NONE',  ( 0.000000000000000000, 0.000000000000000000, 1.000000000000000000 ) ) ;
#3729 = VECTOR ( 'NONE', #42933, 1000.000000000000000 ) ;
#3730 = AXIS2_PLACEMENT_3D ( 'NONE', #26082, #13766, #6585 ) ;
#3731 = EDGE_LOOP ( 'NONE', ( #32546, #41000, #20246, #21661 ) ) ;
#3732 = VERTEX_POINT ( 'NONE', #47181 ) ;
#3733 = VERTEX_POINT ( 'NONE', #285 ) ;
#3734 = CIRCLE ( 'NONE', #38991, 3.749999999999975575 ) ;
#3735 = EDGE_CURVE ( 'NONE', #42730, #27480, #4375, .T. ) ;
#3736 = LINE ( 'NONE', #46036, #47958 ) ;
#3737 = CARTESIAN_POINT ( 'NONE',  ( -40.00000000000000000, 0.000000000000000000, 897.6604670114603550 ) ) ;
#3738 = ORIENTED_EDGE ( 'NONE', *, *, #16114, .T. ) ;
#3739 = LINE ( 'NONE', #38651, #3861 ) ;
#3740 = CARTESIAN_POINT ( 'NONE',  ( 40.00000000000000000, 4.898587196589413026E-15, 897.6604670114603550 ) ) ;
#3741 = DIRECTION ( 'NONE',  ( 7.793956916774525800E-48, 0.000000000000000000, 1.000000000000000000 ) ) ;
#3742 = ORIENTED_EDGE ( 'NONE', *, *, #12633, .T. ) ;
#3743 = ORIENTED_EDGE ( 'NONE', *, *, #48497, .F. ) ;
#3744 = FACE_OUTER_BOUND ( 'NONE', #19132, .T. ) ;
#3745 = FILL_AREA_STYLE ('',( #7868 ) ) ;
#3746 = CARTESIAN_POINT ( 'NONE',  ( -69.99999999999940314, 17.00000000000000000, -54.99999999999999289 ) ) ;
#3747 = ORIENTED_EDGE ( 'NONE', *, *, #48586, .F. ) ;
#3748 = ORIENTED_EDGE ( 'NONE', *, *, #9507, .F. ) ;
#3749 = CARTESIAN_POINT ( 'NONE',  ( -7.884183412771418986, 42.26678417219199702, 893.0811050474360400 ) ) ;
#3750 = LINE ( 'NONE', #31734, #13278 ) ;
#3751 = ORIENTED_EDGE ( 'NONE', *, *, #9821, .F. ) ;
#3752 = AXIS2_PLACEMENT_3D ( 'NONE', #18603, #34279, #3981 ) ;
#3753 = CARTESIAN_POINT ( 'NONE',  ( -194.9999999999999432, -173.0000000000000000, 112.0000000000000284 ) ) ;
#3754 = CARTESIAN_POINT ( 'NONE',  ( -0.2834763335384945515, 1.876787935831946141, 9.900811091504550632 ) ) ;
#3755 = CARTESIAN_POINT ( 'NONE',  ( -210.0000000000000568, 0.000000000000000000, -159.1817124430720298 ) ) ;
#3756 = CARTESIAN_POINT ( 'NONE',  ( -167.7210997126620384, -1.750000000000010214, 81.84341382277507648 ) ) ;
#3757 = AXIS2_PLACEMENT_3D ( 'NONE', #37588, #17056, #33476 ) ;
#3758 = ORIENTED_EDGE ( 'NONE', *, *, #8894, .F. ) ;
#3759 = LINE ( 'NONE', #47071, #12747 ) ;
#3761 = VECTOR ( 'NONE', #19467, 1000.000000000000000 ) ;
#3760 = CARTESIAN_POINT ( 'NONE',  ( -0.2773062244624664441, 1.251557370488897813, 9.948547179989621014 ) ) ;
#3762 = DIRECTION ( 'NONE',  ( -0.000000000000000000, 0.000000000000000000, 1.000000000000000000 ) ) ;
#3763 = EDGE_CURVE ( 'NONE', #17953, #42814, #31332, .T. ) ;
#3764 = DIRECTION ( 'NONE',  ( -1.000000000000000000, 0.000000000000000000, 0.000000000000000000 ) ) ;
#3765 = EDGE_CURVE ( 'NONE', #9029, #24426, #18751, .T. ) ;
#3766 = AXIS2_PLACEMENT_3D ( 'NONE', #45100, #37960, #14581 ) ;
#3767 = MECHANICAL_DESIGN_GEOMETRIC_PRESENTATION_REPRESENTATION (  '', ( #48780 ), #46328 ) ;
#3768 = ORIENTED_EDGE ( 'NONE', *, *, #34779, .T. ) ;
#3769 = EDGE_CURVE ( 'NONE', #34589, #47864, #20467, .T. ) ;
#3770 = CARTESIAN_POINT ( 'NONE',  ( -14.49999999999999822, 13.59802227364769323, -19.51251772323705325 ) ) ;
#3771 = CARTESIAN_POINT ( 'NONE',  ( -16.99749102614300966, 1.320765928724422222, 8.953103998512858652 ) ) ;
#3772 = DIRECTION ( 'NONE',  ( -0.000000000000000000, -1.000000000000000000, -0.000000000000000000 ) ) ;
#3773 = CIRCLE ( 'NONE', #43113, 4.000000000000003553 ) ;
#3774 = EDGE_LOOP ( 'NONE', ( #34613, #34237, #18842, #18030 ) ) ;
#3775 = CARTESIAN_POINT ( 'NONE',  ( -4.945973446814917018, -1.025126265847096763, 159.0682875569279418 ) ) ;
#3776 = DIRECTION ( 'NONE',  ( 0.000000000000000000, -0.000000000000000000, 1.000000000000000000 ) ) ;
#3777 =( BOUNDED_CURVE ( )  B_SPLINE_CURVE ( 3, ( #10523, #6424, #34159, #6670 ),
 .UNSPECIFIED., .F., .F. ) 
 B_SPLINE_CURVE_WITH_KNOTS ( ( 4, 4 ),
 ( 0.000000000000000000, 1.570796326794896558 ),
 .UNSPECIFIED. ) 
 CURVE ( )  GEOMETRIC_REPRESENTATION_ITEM ( )  RATIONAL_B_SPLINE_CURVE ( ( 1.000000000000000000, 0.8047378541243649375, 0.8047378541243649375, 1.000000000000000000 ) ) 
 REPRESENTATION_ITEM ( '' )  );
#3778 = EDGE_LOOP ( 'NONE', ( #35698, #6071, #6455, #44785 ) ) ;
#3779 = CARTESIAN_POINT ( 'NONE',  ( -44.94597344681493922, 2.143131898507880377E-16, 119.0682875569279702 ) ) ;
#3780 = CARTESIAN_POINT ( 'NONE',  ( 164.9999999999999716, 15.00000000000000000, 115.0000000000000142 ) ) ;
#3781 = FACE_OUTER_BOUND ( 'NONE', #6382, .T. ) ;
#3782 = LINE ( 'NONE', #15587, #43815 ) ;
#3783 = ORIENTED_EDGE ( 'NONE', *, *, #25279, .F. ) ;
#3784 = DIRECTION ( 'NONE',  ( -1.000000000000000000, 0.000000000000000000, 0.000000000000000000 ) ) ;
#3785 = ORIENTED_EDGE ( 'NONE', *, *, #26162, .T. ) ;
#3786 = EDGE_LOOP ( 'NONE', ( #5766, #9145, #25506, #27864 ) ) ;
#3787 = CARTESIAN_POINT ( 'NONE',  ( 195.0540265531851105, 2.143131898507880377E-16, 122.5682875569279702 ) ) ;
#3788 = VECTOR ( 'NONE', #45975, 1000.000000000000114 ) ;
#3789 = VERTEX_POINT ( 'NONE', #47934 ) ;
#3790 = PLANE ( 'NONE',  #24 ) ;
#3791 = LINE ( 'NONE', #4307, #46173 ) ;
#3792 = AXIS2_PLACEMENT_3D ( 'NONE', #8237, #35194, #35952 ) ;
#3793 = CARTESIAN_POINT ( 'NONE',  ( -8.445973446814914354, 2.143131898507880377E-16, -160.9317124430720298 ) ) ;
#3794 = VERTEX_POINT ( 'NONE', #47429 ) ;
#3795 = EDGE_CURVE ( 'NONE', #25569, #6330, #43356, .T. ) ;
#3796 = DIRECTION ( 'NONE',  ( 1.000000000000000000, 0.000000000000000000, 0.000000000000000000 ) ) ;
#3797 = CARTESIAN_POINT ( 'NONE',  ( -6.695973446814940111, 1.750000000000024203, 120.8182875569279702 ) ) ;
#3798 = CARTESIAN_POINT ( 'NONE',  ( -69.99999999999940314, 16.00000000000000000, -30.00000000000000000 ) ) ;
#3799 = AXIS2_PLACEMENT_3D ( 'NONE', #2716, #49862, #33290 ) ;
#3800 = ORIENTED_EDGE ( 'NONE', *, *, #22070, .T. ) ;
#3801 = CARTESIAN_POINT ( 'NONE',  ( -3.975459390375366997, -0.2195152216756601216, -2.642742795433417058E-16 ) ) ;
#3802 = LINE ( 'NONE', #8424, #49042 ) ;
#3803 = VERTEX_POINT ( 'NONE', #35187 ) ;
#3804 =( GEOMETRIC_REPRESENTATION_CONTEXT ( 3 ) GLOBAL_UNCERTAINTY_ASSIGNED_CONTEXT ( ( #44071 ) ) GLOBAL_UNIT_ASSIGNED_CONTEXT ( ( #19723, #46878, #43572 ) ) REPRESENTATION_CONTEXT ( 'NONE', 'WORKASPACE' ) );
#3805 = ORIENTED_EDGE ( 'NONE', *, *, #8270, .F. ) ;
#3806 = ORIENTED_EDGE ( 'NONE', *, *, #8825, .F. ) ;
#3807 = DIRECTION ( 'NONE',  ( -0.000000000000000000, -1.000000000000000000, -0.000000000000000000 ) ) ;
#3808 = DIRECTION ( 'NONE',  ( 1.000000000000000000, 0.000000000000000000, 2.958228394578794270E-31 ) ) ;
#3809 = VERTEX_POINT ( 'NONE', #4124 ) ;
#3810 = AXIS2_PLACEMENT_3D ( 'NONE', #5177, #32388, #4924 ) ;
#3811 = CARTESIAN_POINT ( 'NONE',  ( -33.16902712922616558, 37.70469005304312304, 1.847720168420772691 ) ) ;
#3812 = SURFACE_STYLE_FILL_AREA ( #38979 ) ;
#3813 = PLANE ( 'NONE',  #25568 ) ;
#3814 = CYLINDRICAL_SURFACE ( 'NONE', #23539, 1.749999999999973799 ) ;
#3815 = CARTESIAN_POINT ( 'NONE',  ( 151.5540265531850537, 0.000000000000000000, -77.43171244307204404 ) ) ;
#3816 = FACE_OUTER_BOUND ( 'NONE', #13441, .T. ) ;
#3817 = CARTESIAN_POINT ( 'NONE',  ( 39.35269538308637038, 47.68801056904006685, 742.8425600500171413 ) ) ;
#3818 = SURFACE_SIDE_STYLE ('',( #35658 ) ) ;
#3819 = DIRECTION ( 'NONE',  ( 0.000000000000000000, 0.000000000000000000, -1.000000000000000000 ) ) ;
#3820 = CARTESIAN_POINT ( 'NONE',  ( 35.00000000000216716, 17.00000000000000000, 115.0000000000000142 ) ) ;
#3821 = ORIENTED_EDGE ( 'NONE', *, *, #16569, .F. ) ;
#3822 = CARTESIAN_POINT ( 'NONE',  ( 210.0000000000000568, 2.143131898507881856E-16, 119.0682875569279560 ) ) ;
#3823 = LINE ( 'NONE', #38492, #3761 ) ;
#3824 = AXIS2_PLACEMENT_3D ( 'NONE', #35385, #15605, #19446 ) ;
#3825 = CARTESIAN_POINT ( 'NONE',  ( 113.3040265531850537, 1.749999999999996891, 0.8182875569279768335 ) ) ;
#3826 = CARTESIAN_POINT ( 'NONE',  ( -87.72109971266203843, -1.750000000000009548, -0.2068387089191121020 ) ) ;
#3827 = VERTEX_POINT ( 'NONE', #8230 ) ;
#3828 = EDGE_CURVE ( 'NONE', #36764, #21950, #24141, .T. ) ;
#3829 = CARTESIAN_POINT ( 'NONE',  ( 0.000000000000000000, -180.9999999999999716, -340.0000000000001705 ) ) ;
#3830 = CARTESIAN_POINT ( 'NONE',  ( 10.00000000000000355, -48.43825625180578953, 5.363892796379245986 ) ) ;
#3831 = CARTESIAN_POINT ( 'NONE',  ( -124.9459734468149605, 0.000000000000000000, 162.5682875569279702 ) ) ;
#3832 = B_SPLINE_CURVE_WITH_KNOTS ( 'NONE', 3,
 ( #24714, #5700, #48256, #28301 ),
 .UNSPECIFIED., .F., .F.,
 ( 4, 4 ),
 ( 0.000000000000000000, 0.001246897409371959574 ),
 .UNSPECIFIED. ) ;
#3833 =( BOUNDED_CURVE ( )  B_SPLINE_CURVE ( 3, ( #14959, #23667, #23425, #34732 ),
 .UNSPECIFIED., .F., .F. ) 
 B_SPLINE_CURVE_WITH_KNOTS ( ( 4, 4 ),
 ( 0.000000000000000000, 1.570796326794896780 ),
 .UNSPECIFIED. ) 
 CURVE ( )  GEOMETRIC_REPRESENTATION_ITEM ( )  RATIONAL_B_SPLINE_CURVE ( ( 1.000000000000000000, 0.8047378541243649375, 0.8047378541243649375, 1.000000000000000000 ) ) 
 REPRESENTATION_ITEM ( '' )  );
#3834 = ORIENTED_EDGE ( 'NONE', *, *, #4571, .F. ) ;
#3835 = CARTESIAN_POINT ( 'NONE',  ( 343.9999999999999432, -165.0000000000001137, -106.0000000000001990 ) ) ;
#3836 = ORIENTED_EDGE ( 'NONE', *, *, #42791, .F. ) ;
#3837 = DIRECTION ( 'NONE',  ( -4.758098676964956461E-16, 0.000000000000000000, -1.000000000000000000 ) ) ;
#3838 = VERTEX_POINT ( 'NONE', #20277 ) ;
#3839 = DIRECTION ( 'NONE',  ( -1.156482317317870492E-16, 1.000000000000000000, 0.000000000000000000 ) ) ;
#3841 = EDGE_CURVE ( 'NONE', #7468, #41411, #35946, .T. ) ;
#3840 = DIRECTION ( 'NONE',  ( -1.000000000000000000, -0.000000000000000000, -0.000000000000000000 ) ) ;
#3842 =( BOUNDED_CURVE ( )  B_SPLINE_CURVE ( 3, ( #18011, #29571, #2130, #29829 ),
 .UNSPECIFIED., .F., .F. ) 
 B_SPLINE_CURVE_WITH_KNOTS ( ( 4, 4 ),
 ( 0.000000000000000000, 1.570796326794896558 ),
 .UNSPECIFIED. ) 
 CURVE ( )  GEOMETRIC_REPRESENTATION_ITEM ( )  RATIONAL_B_SPLINE_CURVE ( ( 1.000000000000000000, 0.8047378541243649375, 0.8047378541243649375, 1.000000000000000000 ) ) 
 REPRESENTATION_ITEM ( '' )  );
#3843 = ORIENTED_EDGE ( 'NONE', *, *, #5961, .T. ) ;
#3844 = DIRECTION ( 'NONE',  ( -1.000000000000000000, 0.000000000000000000, 0.000000000000000000 ) ) ;
#3845 = ORIENTED_EDGE ( 'NONE', *, *, #39163, .T. ) ;
#3846 = EDGE_CURVE ( 'NONE', #9471, #7228, #32084, .T. ) ;
#3847 = AXIS2_PLACEMENT_3D ( 'NONE', #42030, #21520, #29478 ) ;
#3848 = ORIENTED_EDGE ( 'NONE', *, *, #25155, .F. ) ;
#3849 = FACE_OUTER_BOUND ( 'NONE', #16334, .T. ) ;
#3850 = VERTEX_POINT ( 'NONE', #32595 ) ;
#3851 = DIRECTION ( 'NONE',  ( -0.000000000000000000, -0.000000000000000000, -1.000000000000000000 ) ) ;
#3852 = DIRECTION ( 'NONE',  ( -0.000000000000000000, -1.000000000000000000, -0.000000000000000000 ) ) ;
#3853 = CARTESIAN_POINT ( 'NONE',  ( 356.0000000000006253, 167.0000000000000000, 341.9999999999998863 ) ) ;
#3854 = VERTEX_POINT ( 'NONE', #5373 ) ;
#3855 = EDGE_CURVE ( 'NONE', #35640, #27759, #5651, .T. ) ;
#3856 = CARTESIAN_POINT ( 'NONE',  ( 344.0000000000000568, 181.0000000000000284, 349.9999999999998295 ) ) ;
#3857 = EDGE_CURVE ( 'NONE', #21703, #29662, #29319, .T. ) ;
#3858 = DIRECTION ( 'NONE',  ( -0.000000000000000000, 1.000000000000000000, 0.000000000000000000 ) ) ;
#3859 = ADVANCED_FACE ( 'NONE', ( #36967 ), #37464, .F. ) ;
#3860 = ORIENTED_EDGE ( 'NONE', *, *, #31285, .F. ) ;
#3861 = VECTOR ( 'NONE', #34813, 1000.000000000000000 ) ;
#3862 = LINE ( 'NONE', #7980, #39047 ) ;
#3863 = CARTESIAN_POINT ( 'NONE',  ( -165.0000000000000284, 16.00000000000000000, -114.9999999999999858 ) ) ;
#3864 = ORIENTED_EDGE ( 'NONE', *, *, #28961, .F. ) ;
#3865 = FACE_OUTER_BOUND ( 'NONE', #49674, .T. ) ;
#3866 = CARTESIAN_POINT ( 'NONE',  ( 210.0000000000000568, 2.143131898507881856E-16, 79.06828755692797017 ) ) ;
#3867 = EDGE_LOOP ( 'NONE', ( #9418, #36728, #42468, #12485 ) ) ;
#3868 = DIRECTION ( 'NONE',  ( 0.000000000000000000, -0.000000000000000000, 1.000000000000000000 ) ) ;
#3869 = CARTESIAN_POINT ( 'NONE',  ( -16.50002041759928062, -3.070736177214532514, -9.233365092205394475 ) ) ;
#3870 = CYLINDRICAL_SURFACE ( 'NONE', #45910, 3.500000000000003109 ) ;
#3871 = PLANE ( 'NONE',  #11659 ) ;
#3872 = B_SPLINE_CURVE_WITH_KNOTS ( 'NONE', 3,
 ( #49698, #18433, #41785, #14336 ),
 .UNSPECIFIED., .F., .F.,
 ( 4, 4 ),
 ( 0.000000000000000000, 0.0002610106747150516752 ),
 .UNSPECIFIED. ) ;
#3873 = ORIENTED_EDGE ( 'NONE', *, *, #9412, .T. ) ;
#3874 = FACE_OUTER_BOUND ( 'NONE', #19231, .T. ) ;
#3875 = DIRECTION ( 'NONE',  ( 1.000000000000000000, 0.000000000000000000, -1.586032892321651989E-16 ) ) ;
#3876 = EDGE_LOOP ( 'NONE', ( #20562, #30762, #43189, #31382, #33457, #22011 ) ) ;
#3877 = EDGE_CURVE ( 'NONE', #8815, #47173, #13814, .T. ) ;
#3878 = VERTEX_POINT ( 'NONE', #37218 ) ;
#3879 = CARTESIAN_POINT ( 'NONE',  ( 874.9995338189906988, 1084.939886851464280, 2132.111070289912732 ) ) ;
#3880 = DIRECTION ( 'NONE',  ( -1.586032892321652236E-16, -1.000000000000000000, -2.288264760618012091E-48 ) ) ;
#3881 = PLANE ( 'NONE',  #7841 ) ;
#3882 = EDGE_CURVE ( 'NONE', #34400, #47251, #17126, .T. ) ;
#3883 = EDGE_CURVE ( 'NONE', #34447, #17617, #20770, .T. ) ;
#3884 = FACE_OUTER_BOUND ( 'NONE', #39698, .T. ) ;
#3885 = CARTESIAN_POINT ( 'NONE',  ( 155.0540265531850537, 2.143131898507880377E-16, -120.9317124430720156 ) ) ;
#3886 = VERTEX_POINT ( 'NONE', #48930 ) ;
#3887 = CARTESIAN_POINT ( 'NONE',  ( -166.6959734468149463, 1.750000000000009992, 0.8182875569279768335 ) ) ;
#3888 = EDGE_CURVE ( 'NONE', #34035, #31951, #9225, .T. ) ;
#3889 = CARTESIAN_POINT ( 'NONE',  ( -0.3862712429686809279, -1.188820645368943163, -10.00000000000000000 ) ) ;
#3890 = CARTESIAN_POINT ( 'NONE',  ( -164.9459734468149463, 1.025126265847089435, 159.0682875569279418 ) ) ;
#3891 = EDGE_CURVE ( 'NONE', #27411, #18811, #40534, .T. ) ;
#3892 = CARTESIAN_POINT ( 'NONE',  ( 344.0000000000000000, 174.9999999999996589, -344.0000000000002842 ) ) ;
#3893 = VERTEX_POINT ( 'NONE', #13575 ) ;
#3894 = DIRECTION ( 'NONE',  ( 3.172065745548403743E-16, 1.000000000000000000, 0.000000000000000000 ) ) ;
#3896 = ORIENTED_EDGE ( 'NONE', *, *, #28398, .F. ) ;
#3895 = AXIS2_PLACEMENT_3D ( 'NONE', #12157, #20101, #1378 ) ;
#3897 = CARTESIAN_POINT ( 'NONE',  ( 0.000000000000000000, 0.000000000000000000, -10.00000000000000000 ) ) ;
#3898 = PLANE ( 'NONE',  #36039 ) ;
#3899 = ORIENTED_EDGE ( 'NONE', *, *, #28728, .F. ) ;
#3900 = LINE ( 'NONE', #15702, #48312 ) ;
#3901 = CARTESIAN_POINT ( 'NONE',  ( 23.31729631074197329, 24.19776167542427814, -8.016098858316205167 ) ) ;
#3902 = CARTESIAN_POINT ( 'NONE',  ( 181.0000000000000000, -184.9999999999999716, -342.0000000000001137 ) ) ;
#3903 = ORIENTED_EDGE ( 'NONE', *, *, #13705, .F. ) ;
#3904 = CARTESIAN_POINT ( 'NONE',  ( 5.551115123125782702E-14, -168.9999999999999432, 359.9999999999997726 ) ) ;
#3905 = DIRECTION ( 'NONE',  ( 0.000000000000000000, 0.000000000000000000, -1.000000000000000000 ) ) ;
#3906 = ORIENTED_EDGE ( 'NONE', *, *, #35697, .F. ) ;
#3907 = PLANE ( 'NONE',  #42666 ) ;
#3908 = LINE ( 'NONE', #10652, #47749 ) ;
#3909 = DIRECTION ( 'NONE',  ( 0.000000000000000000, 0.000000000000000000, 1.000000000000000000 ) ) ;
#3910 = UNCERTAINTY_MEASURE_WITH_UNIT (LENGTH_MEASURE( 1.000000000000000082E-05 ), #38612, 'distance_accuracy_value', 'NONE');
#3911 = CARTESIAN_POINT ( 'NONE',  ( -164.4973046169135955, 53.53801056904001854, -93.79675437945476801 ) ) ;
#3912 = ORIENTED_EDGE ( 'NONE', *, *, #48957, .T. ) ;
#3914 = EDGE_LOOP ( 'NONE', ( #27318, #30038, #31505, #40737 ) ) ;
#3913 = ADVANCED_FACE ( 'NONE', ( #2281, #21788 ), #44851, .F. ) ;
#3915 = CARTESIAN_POINT ( 'NONE',  ( 210.0000000000000568, 0.000000000000000000, -79.18171244307201562 ) ) ;
#3916 = EDGE_CURVE ( 'NONE', #9256, #30177, #1539, .T. ) ;
#3917 = B_SPLINE_CURVE_WITH_KNOTS ( 'NONE', 3,
 ( #17755, #37528, #5691, #37032 ),
 .UNSPECIFIED., .F., .F.,
 ( 4, 4 ),
 ( 0.0002736185395732594399, 0.0005346342798032415345 ),
 .UNSPECIFIED. ) ;
#3918 = EDGE_CURVE ( 'NONE', #34995, #13154, #32326, .T. ) ;
#3919 = EDGE_CURVE ( 'NONE', #7547, #49568, #21277, .T. ) ;
#3920 = ORIENTED_EDGE ( 'NONE', *, *, #13177, .F. ) ;
#3921 = DIRECTION ( 'NONE',  ( 1.000000000000000000, 0.000000000000000000, 0.000000000000000000 ) ) ;
#3922 = CARTESIAN_POINT ( 'NONE',  ( 151.5540265531850537, 0.000000000000000000, 165.0000000000000000 ) ) ;
#3923 = CARTESIAN_POINT ( 'NONE',  ( 34.32915281903212446, 1.750000000000009548, 39.79316129108089228 ) ) ;
#3924 = ORIENTED_EDGE ( 'NONE', *, *, #37456, .T. ) ;
#3925 = DIRECTION ( 'NONE',  ( -0.000000000000000000, -0.000000000000000000, -1.000000000000000000 ) ) ;
#3926 = EDGE_CURVE ( 'NONE', #34772, #8207, #5879, .T. ) ;
#3927 = ORIENTED_EDGE ( 'NONE', *, *, #35284, .T. ) ;
#3928 = ADVANCED_FACE ( 'NONE', ( #17684 ), #5622, .T. ) ;
#3929 = CARTESIAN_POINT ( 'NONE',  ( -14.86945752723352498, -7.944783388878907004, 2.590526750877053086 ) ) ;
#3930 = CARTESIAN_POINT ( 'NONE',  ( -126.6959734468149321, 0.000000000000000000, 165.0000000000000000 ) ) ;
#3931 = CARTESIAN_POINT ( 'NONE',  ( 185.0000000000000284, -180.9999999999993747, -115.0000000000001279 ) ) ;
#3932 = ORIENTED_EDGE ( 'NONE', *, *, #33759, .F. ) ;
#3933 = AXIS2_PLACEMENT_3D ( 'NONE', #38935, #27118, #7620 ) ;
#3934 = ORIENTED_EDGE ( 'NONE', *, *, #21121, .F. ) ;
#3935 = ORIENTED_EDGE ( 'NONE', *, *, #16714, .T. ) ;
#3936 = CARTESIAN_POINT ( 'NONE',  ( -114.9999999999987779, 17.00000000000000000, 30.00000000000000000 ) ) ;
#3937 = CARTESIAN_POINT ( 'NONE',  ( -48.44597344681495343, 0.000000000000000000, 165.0000000000000000 ) ) ;
#3938 = ORIENTED_EDGE ( 'NONE', *, *, #33386, .F. ) ;
#3939 = CARTESIAN_POINT ( 'NONE',  ( 344.0000000000000000, 175.0000000000000284, -94.00000000000019895 ) ) ;
#3940 = ORIENTED_EDGE ( 'NONE', *, *, #44807, .T. ) ;
#3941 = EDGE_CURVE ( 'NONE', #40207, #1237, #47400, .T. ) ;
#3942 = DIRECTION ( 'NONE',  ( -1.368455531567204171E-48, 1.000000000000000000, 2.265761274745217480E-16 ) ) ;
#3943 = ORIENTED_EDGE ( 'NONE', *, *, #12300, .F. ) ;
#3944 =( NAMED_UNIT ( * ) PLANE_ANGLE_UNIT ( ) SI_UNIT ( $, .RADIAN. ) );
#3945 = CARTESIAN_POINT ( 'NONE',  ( 75.05402655318509630, 2.143131898507880377E-16, 165.0000000000000000 ) ) ;
#3946 = LINE ( 'NONE', #19079, #14545 ) ;
#3947 = LINE ( 'NONE', #32669, #24210 ) ;
#3948 = ADVANCED_FACE ( 'NONE', ( #28979 ), #44594, .T. ) ;
#3949 = EDGE_CURVE ( 'NONE', #7843, #1108, #14331, .T. ) ;
#3950 = CYLINDRICAL_SURFACE ( 'NONE', #50286, 1.750000000000008438 ) ;
#3951 = ORIENTED_EDGE ( 'NONE', *, *, #17445, .F. ) ;
#3952 = ORIENTED_EDGE ( 'NONE', *, *, #48838, .T. ) ;
#3953 = DIRECTION ( 'NONE',  ( 1.000000000000000000, 0.000000000000000000, 0.000000000000000000 ) ) ;
#3954 = B_SPLINE_SURFACE_WITH_KNOTS ( 'NONE', 3, 3, ( 
 ( #14795, #45804, #6591, #2490 ),
 ( #30714, #14536, #26853, #2734 ),
 ( #41493, #18381, #34061, #2238 ),
 ( #34302, #46317, #49645, #10689 ) ),
 .UNSPECIFIED., .F., .F., .F.,
 ( 4, 4 ),
 ( 4, 4 ),
 ( 0.000000000000000000, 1.000000000000000000 ),
 ( 0.000000000000000000, 1.000000000000000000 ),
 .UNSPECIFIED. ) ;
#3955 = FACE_OUTER_BOUND ( 'NONE', #41248, .T. ) ;
#3956 = DIRECTION ( 'NONE',  ( 0.000000000000000000, 0.000000000000000000, 1.000000000000000000 ) ) ;
#3957 = CARTESIAN_POINT ( 'NONE',  ( -214.9999999999999432, 173.0000000000000000, 352.0000000000000000 ) ) ;
#3958 = CARTESIAN_POINT ( 'NONE',  ( 34.30563531518984632, 15.23322832906888991, 6.057468652304070389 ) ) ;
#3959 = ORIENTED_EDGE ( 'NONE', *, *, #50304, .T. ) ;
#3960 = EDGE_CURVE ( 'NONE', #43789, #4257, #22791, .T. ) ;
#3961 = CARTESIAN_POINT ( 'NONE',  ( -0.4426377647354682865, -1.666766018367764834, 9.928159647716134018 ) ) ;
#3962 = DIRECTION ( 'NONE',  ( 0.000000000000000000, -2.265761274745217480E-16, 1.000000000000000000 ) ) ;
#3963 = ORIENTED_EDGE ( 'NONE', *, *, #13651, .T. ) ;
#3964 = AXIS2_PLACEMENT_3D ( 'NONE', #5219, #16771, #9076 ) ;
#3965 = LINE ( 'NONE', #30155, #23785 ) ;
#3966 = EDGE_CURVE ( 'NONE', #46337, #15022, #22288, .T. ) ;
#3967 = CARTESIAN_POINT ( 'NONE',  ( 183.0000000000000568, 175.0000000000000284, 355.9999999999998863 ) ) ;
#3968 = CARTESIAN_POINT ( 'NONE',  ( 194.9999999999999432, -173.0000000000000000, 352.0000000000000568 ) ) ;
#3969 = ORIENTED_EDGE ( 'NONE', *, *, #971, .F. ) ;
#3970 = CLOSED_SHELL ( 'NONE', ( #5604, #21662, #14912, #36988, #40306, #22135, #14564, #29609, #3913, #4055, #40441, #39067, #37568, #15185, #49985, #11877, #2685, #16782 ) ) ;
#3971 = VERTEX_POINT ( 'NONE', #34604 ) ;
#3972 = CARTESIAN_POINT ( 'NONE',  ( 1.114871695981101585, -0.4953159757246433093, 9.963925895596188909 ) ) ;
#3973 = CARTESIAN_POINT ( 'NONE',  ( 0.6440276692615888310, 16.64212148744554298, -9.683996418299976483 ) ) ;
#3974 =( BOUNDED_CURVE ( )  B_SPLINE_CURVE ( 3, ( #31860, #30848, #39059, #23638 ),
 .UNSPECIFIED., .F., .F. ) 
 B_SPLINE_CURVE_WITH_KNOTS ( ( 4, 4 ),
 ( 4.712388980384689674, 6.283185307179586232 ),
 .UNSPECIFIED. ) 
 CURVE ( )  GEOMETRIC_REPRESENTATION_ITEM ( )  RATIONAL_B_SPLINE_CURVE ( ( 1.000000000000000000, 0.8047378541243649375, 0.8047378541243649375, 1.000000000000000000 ) ) 
 REPRESENTATION_ITEM ( '' )  );
#3975 = EDGE_CURVE ( 'NONE', #29168, #1639, #10342, .T. ) ;
#3976 = EDGE_CURVE ( 'NONE', #32354, #9732, #9690, .T. ) ;
#3977 = ORIENTED_EDGE ( 'NONE', *, *, #44635, .T. ) ;
#3978 = ORIENTED_EDGE ( 'NONE', *, *, #29078, .F. ) ;
#3979 = FACE_OUTER_BOUND ( 'NONE', #5848, .T. ) ;
#3980 = CARTESIAN_POINT ( 'NONE',  ( -1.011271242968677875, -0.7347315653656004697, 10.00000000000000000 ) ) ;
#3981 = DIRECTION ( 'NONE',  ( -1.000000000000000000, 0.000000000000000000, 0.000000000000000000 ) ) ;
#3982 = CARTESIAN_POINT ( 'NONE',  ( 35.00000000000091660, 16.00000000000000000, -24.99999999999999289 ) ) ;
#3983 = ORIENTED_EDGE ( 'NONE', *, *, #21589, .F. ) ;
#3984 = ORIENTED_EDGE ( 'NONE', *, *, #46187, .T. ) ;
#3985 = VERTEX_POINT ( 'NONE', #30000 ) ;
#3986 = EDGE_CURVE ( 'NONE', #17007, #4976, #15098, .T. ) ;
#3987 = EDGE_CURVE ( 'NONE', #20660, #10986, #48211, .T. ) ;
#3988 = CARTESIAN_POINT ( 'NONE',  ( -69.99999999999972999, 17.00000000000000000, -60.00000000000000000 ) ) ;
#3989 = EDGE_CURVE ( 'NONE', #2713, #24145, #14585, .T. ) ;
#3990 = CARTESIAN_POINT ( 'NONE',  ( 15.00000000000000000, -46.01315789473684248, 0.000000000000000000 ) ) ;
#3991 = VERTEX_POINT ( 'NONE', #33855 ) ;
#3992 = CARTESIAN_POINT ( 'NONE',  ( 7.576114424932982594, -50.00000000000000711, 7.906207997025717304 ) ) ;
#3993 = CARTESIAN_POINT ( 'NONE',  ( 33.30402655318503946, -1.750000000000010658, 80.81828755692798438 ) ) ;
#3994 = DIRECTION ( 'NONE',  ( -1.000000000000000000, -0.000000000000000000, -0.000000000000000000 ) ) ;
#3995 = ORIENTED_EDGE ( 'NONE', *, *, #23764, .T. ) ;
#3996 = EDGE_LOOP ( 'NONE', ( #13400, #28611, #38508, #24216 ) ) ;
#3997 = DIRECTION ( 'NONE',  ( 0.000000000000000000, 0.000000000000000000, 1.000000000000000000 ) ) ;
#3998 = LINE ( 'NONE', #42476, #48834 ) ;
#3999 = EDGE_CURVE ( 'NONE', #45654, #40426, #19184, .T. ) ;
#4000 =( BOUNDED_CURVE ( )  B_SPLINE_CURVE ( 3, ( #39859, #12622, #36258, #24450 ),
 .UNSPECIFIED., .F., .F. ) 
 B_SPLINE_CURVE_WITH_KNOTS ( ( 4, 4 ),
 ( 1.570796326794896558, 3.141592653589793116 ),
 .UNSPECIFIED. ) 
 CURVE ( )  GEOMETRIC_REPRESENTATION_ITEM ( )  RATIONAL_B_SPLINE_CURVE ( ( 1.000000000000000000, 0.8047378541243649375, 0.8047378541243649375, 1.000000000000000000 ) ) 
 REPRESENTATION_ITEM ( '' )  );
#4001 = CARTESIAN_POINT ( 'NONE',  ( 112.2789002873379758, -1.749999999999996669, -0.2068387089191042749 ) ) ;
#4002 = UNCERTAINTY_MEASURE_WITH_UNIT (LENGTH_MEASURE( 1.000000000000000082E-05 ), #34161, 'distance_accuracy_value', 'NONE');
#4003 = VERTEX_POINT ( 'NONE', #50453 ) ;
#4004 = EDGE_LOOP ( 'NONE', ( #45643, #20142, #21708, #8905 ) ) ;
#4005 = CARTESIAN_POINT ( 'NONE',  ( 0.000000000000000000, 0.000000000000000000, 10.00000000000000000 ) ) ;
#4007 = EDGE_LOOP ( 'NONE', ( #3068, #30208, #39787, #782 ) ) ;
#4006 = AXIS2_PLACEMENT_3D ( 'NONE', #17381, #17135, #21731 ) ;
#4008 = CARTESIAN_POINT ( 'NONE',  ( 210.0000000000000568, 2.143131898507881116E-16, -40.93171244307203693 ) ) ;
#4009 = CARTESIAN_POINT ( 'NONE',  ( -164.4973046169135955, 70.03596893647589638, -93.79675437945476801 ) ) ;
#4010 = CARTESIAN_POINT ( 'NONE',  ( 181.0000000000000000, -164.9999999999999432, -350.0000000000001705 ) ) ;
#4011 = VECTOR ( 'NONE', #27751, 1000.000000000000000 ) ;
#4012 = CARTESIAN_POINT ( 'NONE',  ( -86.69597344681496054, 0.000000000000000000, 165.0000000000000000 ) ) ;
#4013 = VECTOR ( 'NONE', #39558, 1000.000000000000000 ) ;
#4014 = VERTEX_POINT ( 'NONE', #2780 ) ;
#4015 = VECTOR ( 'NONE', #3281, 1000.000000000000000 ) ;
#4016 = CARTESIAN_POINT ( 'NONE',  ( -50.64730461691362962, -42.31198943095992604, 742.8425600500171413 ) ) ;
#4017 = LINE ( 'NONE', #19413, #46952 ) ;
#4018 = DIRECTION ( 'NONE',  ( 1.000000000000000000, 0.000000000000000000, 0.000000000000000000 ) ) ;
#4019 = VECTOR ( 'NONE', #18189, 1000.000000000000000 ) ;
#4020 = CARTESIAN_POINT ( 'NONE',  ( 32.87128375420895310, 6.537745902885608196, -8.466730184410787174 ) ) ;
#4021 = VECTOR ( 'NONE', #29786, 1000.000000000000000 ) ;
#4022 =( REPRESENTATION_RELATIONSHIP ('NONE','NONE', #45699, #50327 ) REPRESENTATION_RELATIONSHIP_WITH_TRANSFORMATION ( #22556 )SHAPE_REPRESENTATION_RELATIONSHIP( ) );
#4023 = ORIENTED_EDGE ( 'NONE', *, *, #7311, .T. ) ;
#4024 = PLANE ( 'NONE',  #33528 ) ;
#4025 = CARTESIAN_POINT ( 'NONE',  ( 0.1287570809895604018, 0.3962735484563146282, 10.00000000000000000 ) ) ;
#4026 = CARTESIAN_POINT ( 'NONE',  ( 183.0000000000000568, 175.0000000000000284, 343.9999999999998863 ) ) ;
#4027 = EDGE_CURVE ( 'NONE', #23110, #34075, #10732, .T. ) ;
#4028 = VERTEX_POINT ( 'NONE', #18428 ) ;
#4029 = DIRECTION ( 'NONE',  ( -1.000000000000000000, 0.000000000000000000, -7.793956916774525800E-48 ) ) ;
#4030 = CARTESIAN_POINT ( 'NONE',  ( 181.0000000000000284, -174.9999999999999716, -113.0000000000001563 ) ) ;
#4031 = ORIENTED_EDGE ( 'NONE', *, *, #39464, .F. ) ;
#4032 = DIRECTION ( 'NONE',  ( -1.000000000000000000, 0.000000000000000000, 0.000000000000000000 ) ) ;
#4033 = FACE_OUTER_BOUND ( 'NONE', #36953, .T. ) ;
#4034 = CARTESIAN_POINT ( 'NONE',  ( 23.83799721022594298, -28.99517291086361581, 3.209567239418974705 ) ) ;
#4035 = ORIENTED_EDGE ( 'NONE', *, *, #24733, .F. ) ;
#4036 = CARTESIAN_POINT ( 'NONE',  ( 195.0540265531851105, 1.025126265847089879, -117.4317124430720156 ) ) ;
#4037 = ORIENTED_EDGE ( 'NONE', *, *, #26822, .T. ) ;
#4038 = ORIENTED_EDGE ( 'NONE', *, *, #49620, .T. ) ;
#4039 = CARTESIAN_POINT ( 'NONE',  ( 16.73672383626881199, 2.341008440548111302, -9.008049429158100807 ) ) ;
#4040 = DIRECTION ( 'NONE',  ( -1.000000000000000000, -0.000000000000000000, -0.000000000000000000 ) ) ;
#4041 = CIRCLE ( 'NONE', #7336, 3.500000000000003109 ) ;
#4042 = EDGE_CURVE ( 'NONE', #18475, #55, #46609, .T. ) ;
#4043 = AXIS2_PLACEMENT_3D ( 'NONE', #40755, #1508, #13033 ) ;
#4044 = EDGE_CURVE ( 'NONE', #49920, #14126, #34109, .T. ) ;
#4045 = ORIENTED_EDGE ( 'NONE', *, *, #1422, .F. ) ;
#4046 = FACE_OUTER_BOUND ( 'NONE', #4196, .T. ) ;
#4047 = LINE ( 'NONE', #8159, #24117 ) ;
#4048 =( GEOMETRIC_REPRESENTATION_CONTEXT ( 3 ) GLOBAL_UNCERTAINTY_ASSIGNED_CONTEXT ( ( #38700 ) ) GLOBAL_UNIT_ASSIGNED_CONTEXT ( ( #20976, #36658, #48372 ) ) REPRESENTATION_CONTEXT ( 'NONE', 'WORKASPACE' ) );
#4049 = VECTOR ( 'NONE', #32562, 1000.000000000000000 ) ;
#4050 = DIRECTION ( 'NONE',  ( -1.000000000000000000, 0.000000000000000000, 0.000000000000000000 ) ) ;
#4051 = VERTEX_POINT ( 'NONE', #15361 ) ;
#4053 = ADVANCED_FACE ( 'NONE', ( #25900 ), #26390, .F. ) ;
#4052 = CARTESIAN_POINT ( 'NONE',  ( 73.30402655318508209, 1.750000000000010658, 120.8182875569279702 ) ) ;
#4054 = DIRECTION ( 'NONE',  ( 1.000000000000000000, -3.172065784643302499E-16, -1.942330104924128867E-32 ) ) ;
#4055 = ADVANCED_FACE ( 'NONE', ( #14842 ), #30494, .F. ) ;
#4056 = CARTESIAN_POINT ( 'NONE',  ( 9.760995290733820440, -2.173239732351728293, 9.646707543097347681 ) ) ;
#4057 = AXIS2_PLACEMENT_3D ( 'NONE', #24752, #36814, #43720 ) ;
#4058 = VERTEX_POINT ( 'NONE', #2534 ) ;
#4059 = DIRECTION ( 'NONE',  ( -1.000000000000000000, 0.000000000000000000, 0.000000000000000000 ) ) ;
#4060 = CARTESIAN_POINT ( 'NONE',  ( 2.735102768439324983, -5.294960982149635953, 5.387129544537350156E-16 ) ) ;
#4061 = VERTEX_POINT ( 'NONE', #26650 ) ;
#4062 = ORIENTED_EDGE ( 'NONE', *, *, #44355, .T. ) ;
#4063 = ORIENTED_EDGE ( 'NONE', *, *, #33730, .T. ) ;
#4064 = DIRECTION ( 'NONE',  ( 1.000000000000000000, 0.000000000000000000, 0.000000000000000000 ) ) ;
#4065 = EDGE_CURVE ( 'NONE', #24372, #6656, #22031, .T. ) ;
#4066 = DIRECTION ( 'NONE',  ( 0.000000000000000000, 1.000000000000000000, 0.000000000000000000 ) ) ;
#4067 = PRODUCT_DEFINITION_SHAPE ( 'NONE', 'NONE',  #6792 ) ;
#4068 = ORIENTED_EDGE ( 'NONE', *, *, #9441, .T. ) ;
#4069 = DIRECTION ( 'NONE',  ( -1.000000000000000000, -0.000000000000000000, -0.000000000000000000 ) ) ;
#4070 = CARTESIAN_POINT ( 'NONE',  ( -556.8973046169135159, 54.43801056904003133, -64.63743994998280584 ) ) ;
#4071 = CARTESIAN_POINT ( 'NONE',  ( 0.1287570809895630941, -0.3962735484563133515, 10.00000000000000000 ) ) ;
#4072 = CARTESIAN_POINT ( 'NONE',  ( -4.763548243873389154, 16.57409059453848599, 8.727788335465566760 ) ) ;
#4073 = CARTESIAN_POINT ( 'NONE',  ( 8.813458710706171928, 4.724716452304571490, 0.000000000000000000 ) ) ;
#4074 = DIRECTION ( 'NONE',  ( 1.000000000000000000, 0.000000000000000000, 0.000000000000000000 ) ) ;
#4075 = FACE_OUTER_BOUND ( 'NONE', #46172, .T. ) ;
#4076 = FACE_OUTER_BOUND ( 'NONE', #31892, .T. ) ;
#4077 = FACE_OUTER_BOUND ( 'NONE', #33283, .T. ) ;
#4078 = B_SPLINE_CURVE_WITH_KNOTS ( 'NONE', 3,
 ( #1510, #36422, #13541, #4827 ),
 .UNSPECIFIED., .F., .F.,
 ( 4, 4 ),
 ( 0.002217981418809652702, 0.002368422649471284280 ),
 .UNSPECIFIED. ) ;
#4079 = CARTESIAN_POINT ( 'NONE',  ( 35.05402655318504657, 2.143131898507880377E-16, 119.0682875569279702 ) ) ;
#4080 = VECTOR ( 'NONE', #6104, 1000.000000000000000 ) ;
#4081 = DIRECTION ( 'NONE',  ( 0.000000000000000000, 1.000000000000000000, 7.004339610132985974E-48 ) ) ;
#4082 = CARTESIAN_POINT ( 'NONE',  ( -0.6538612634427415360, -1.160398818844775137, 9.951893257060017817 ) ) ;
#4083 = VECTOR ( 'NONE', #46518, 1000.000000000000000 ) ;
#4084 =( BOUNDED_CURVE ( )  B_SPLINE_CURVE ( 3, ( #29993, #38216, #10989, #45608 ),
 .UNSPECIFIED., .F., .F. ) 
 B_SPLINE_CURVE_WITH_KNOTS ( ( 4, 4 ),
 ( 3.141592653589793116, 4.712388980384689674 ),
 .UNSPECIFIED. ) 
 CURVE ( )  GEOMETRIC_REPRESENTATION_ITEM ( )  RATIONAL_B_SPLINE_CURVE ( ( 1.000000000000000000, 0.8047378541243649375, 0.8047378541243649375, 1.000000000000000000 ) ) 
 REPRESENTATION_ITEM ( '' )  );
#4085 = DIRECTION ( 'NONE',  ( -0.000000000000000000, 1.000000000000000000, 0.000000000000000000 ) ) ;
#4086 = CARTESIAN_POINT ( 'NONE',  ( -1.011271242968683204, -0.7347315653655928092, 9.972675548442467175 ) ) ;
#4087 = ORIENTED_EDGE ( 'NONE', *, *, #15514, .T. ) ;
#4088 = VECTOR ( 'NONE', #48245, 1000.000000000000000 ) ;
#4089 = LINE ( 'NONE', #19471, #3219 ) ;
#4090 = EDGE_CURVE ( 'NONE', #11678, #7132, #7150, .T. ) ;
#4091 = LINE ( 'NONE', #39506, #752 ) ;
#4092 = CARTESIAN_POINT ( 'NONE',  ( -114.9999999999984652, 17.00000000000000000, 35.00000000000000000 ) ) ;
#4093 = CARTESIAN_POINT ( 'NONE',  ( -164.9999999999997442, 17.00000000000000000, -60.00000000000000000 ) ) ;
#4094 = EDGE_CURVE ( 'NONE', #14213, #34995, #39982, .T. ) ;
#4095 = VECTOR ( 'NONE', #23354, 1000.000000000000000 ) ;
#4096 = ORIENTED_EDGE ( 'NONE', *, *, #42266, .F. ) ;
#4097 = DIRECTION ( 'NONE',  ( 1.000000000000000000, 0.000000000000000000, 0.000000000000000000 ) ) ;
#4098 = ORIENTED_EDGE ( 'NONE', *, *, #11415, .F. ) ;
#4099 = CARTESIAN_POINT ( 'NONE',  ( 154.1026953830863420, -67.00570555996102939, -94.69675437945474528 ) ) ;
#4100 = EDGE_LOOP ( 'NONE', ( #10245, #1725, #31201, #13474, #10113, #50113, #38344, #30433, #8919, #20264, #3675, #23335 ) ) ;
#4101 = FACE_OUTER_BOUND ( 'NONE', #10309, .T. ) ;
#4102 = CARTESIAN_POINT ( 'NONE',  ( -48.44597344681495343, 0.000000000000000000, 165.0000000000000000 ) ) ;
#4103 = ORIENTED_EDGE ( 'NONE', *, *, #35044, .F. ) ;
#4104 = FACE_OUTER_BOUND ( 'NONE', #4399, .T. ) ;
#4105 = ORIENTED_EDGE ( 'NONE', *, *, #28088, .T. ) ;
#4106 = EDGE_LOOP ( 'NONE', ( #5600, #5557, #11696, #10221 ) ) ;
#4107 = CARTESIAN_POINT ( 'NONE',  ( 29.99999999999998579, 17.00000000000000000, -90.00000000000000000 ) ) ;
#4108 = DIRECTION ( 'NONE',  ( -0.000000000000000000, -0.000000000000000000, -1.000000000000000000 ) ) ;
#4109 = ORIENTED_EDGE ( 'NONE', *, *, #35919, .F. ) ;
#4110 = CARTESIAN_POINT ( 'NONE',  ( -12.15085308559838317, 11.68662139125813226, 2.590526750877053086 ) ) ;
#4111 = CARTESIAN_POINT ( 'NONE',  ( -4.945973446814917018, 1.025126265847097429, -37.43171244307200851 ) ) ;
#4112 = LINE ( 'NONE', #47172, #17541 ) ;
#4113 = VERTEX_POINT ( 'NONE', #43803 ) ;
#4114 = CARTESIAN_POINT ( 'NONE',  ( -165.0000000000000284, 16.00000000000000000, 115.0000000000000142 ) ) ;
#4115 = AXIS2_PLACEMENT_3D ( 'NONE', #4245, #30424, #43231 ) ;
#4116 = B_SPLINE_CURVE_WITH_KNOTS ( 'NONE', 3,
 ( #8925, #28675, #13520, #9174 ),
 .UNSPECIFIED., .F., .F.,
 ( 4, 4 ),
 ( 1.734723475976807094E-18, 2.804146970187102689E-05 ),
 .UNSPECIFIED. ) ;
#4117 = CARTESIAN_POINT ( 'NONE',  ( -210.0000000000000568, 0.000000000000000000, 162.5682875569279702 ) ) ;
#4118 = VECTOR ( 'NONE', #13988, 1000.000000000000000 ) ;
#4119 = VECTOR ( 'NONE', #6423, 1000.000000000000000 ) ;
#4120 = ORIENTED_EDGE ( 'NONE', *, *, #26509, .T. ) ;
#4121 = CARTESIAN_POINT ( 'NONE',  ( -1.250000000000000222, 0.000000000000000000, 10.00000000000000000 ) ) ;
#4122 = AXIS2_PLACEMENT_3D ( 'NONE', #13723, #20925, #48072 ) ;
#4123 = VECTOR ( 'NONE', #17070, 1000.000000000000227 ) ;
#4124 = CARTESIAN_POINT ( 'NONE',  ( 168.9999999999999716, -164.9999999999999432, 339.9999999999997726 ) ) ;
#4125 = ORIENTED_EDGE ( 'NONE', *, *, #14574, .F. ) ;
#4126 = CARTESIAN_POINT ( 'NONE',  ( -88.44597344681494633, 1.025126265847089213, -0.9317124430720324924 ) ) ;
#4127 = EDGE_CURVE ( 'NONE', #323, #41298, #36624, .T. ) ;
#4128 = AXIS2_PLACEMENT_3D ( 'NONE', #35136, #26655, #23821 ) ;
#4129 = PRESENTATION_LAYER_ASSIGNMENT (  '', '', ( #2467 ) ) ;
#4130 = CARTESIAN_POINT ( 'NONE',  ( 135.0000000000003411, 16.00000000000000000, -60.00000000000000000 ) ) ;
#4131 = ORIENTED_EDGE ( 'NONE', *, *, #9276, .F. ) ;
#4132 = CARTESIAN_POINT ( 'NONE',  ( 25.40454589245968364, 27.58367357691700406, -8.192531242611265085 ) ) ;
#4133 = CARTESIAN_POINT ( 'NONE',  ( -33.08717642956897009, -5.870837526464926626, -8.016098858316205167 ) ) ;
#4134 = DIRECTION ( 'NONE',  ( 1.000000000000000000, 0.000000000000000000, 0.000000000000000000 ) ) ;
#4135 = VECTOR ( 'NONE', #44345, 1000.000000000000000 ) ;
#4136 = CARTESIAN_POINT ( 'NONE',  ( 4.204997580903516941, -7.388441598285492518, 229.0000000000000000 ) ) ;
#4137 = EDGE_LOOP ( 'NONE', ( #43328, #16531, #2229, #20430, #253 ) ) ;
#4138 = CARTESIAN_POINT ( 'NONE',  ( -85.67084718096784002, 1.750000000000009548, -160.2068387089191219 ) ) ;
#4139 = CARTESIAN_POINT ( 'NONE',  ( 29.18392875402930997, 17.44843138996603216, 7.906207997025717304 ) ) ;
#4140 = PLANE ( 'NONE',  #24805 ) ;
#4141 = ORIENTED_EDGE ( 'NONE', *, *, #39314, .T. ) ;
#4142 = EDGE_LOOP ( 'NONE', ( #9671, #14688, #699, #4511 ) ) ;
#4143 = APPLICATION_PROTOCOL_DEFINITION ( 'draft international standard', 'automotive_design', 1998, #18094 ) ;
#4144 =( BOUNDED_CURVE ( )  B_SPLINE_CURVE ( 3, ( #21576, #10292, #37269, #41335 ),
 .UNSPECIFIED., .F., .F. ) 
 B_SPLINE_CURVE_WITH_KNOTS ( ( 4, 4 ),
 ( 1.570796326794896558, 3.141592653589793116 ),
 .UNSPECIFIED. ) 
 CURVE ( )  GEOMETRIC_REPRESENTATION_ITEM ( )  RATIONAL_B_SPLINE_CURVE ( ( 1.000000000000000000, 0.8047378541243649375, 0.8047378541243649375, 1.000000000000000000 ) ) 
 REPRESENTATION_ITEM ( '' )  );
#4145 = FACE_OUTER_BOUND ( 'NONE', #18052, .T. ) ;
#4146 = PLANE ( 'NONE',  #39828 ) ;
#4147 = CYLINDRICAL_SURFACE ( 'NONE', #7760, 2.000000000000001776 ) ;
#4148 = CARTESIAN_POINT ( 'NONE',  ( -86.69597344681494633, 1.750000000000010658, -119.1817124430720440 ) ) ;
#4149 = ORIENTED_EDGE ( 'NONE', *, *, #50255, .T. ) ;
#4150 = LINE ( 'NONE', #814, #47619 ) ;
#4151 =( BOUNDED_CURVE ( )  B_SPLINE_CURVE ( 3, ( #39901, #7638, #15584, #46583 ),
 .UNSPECIFIED., .F., .F. ) 
 B_SPLINE_CURVE_WITH_KNOTS ( ( 4, 4 ),
 ( 4.712388980384689674, 6.283185307179586232 ),
 .UNSPECIFIED. ) 
 CURVE ( )  GEOMETRIC_REPRESENTATION_ITEM ( )  RATIONAL_B_SPLINE_CURVE ( ( 1.000000000000000000, 0.8047378541243649375, 0.8047378541243649375, 1.000000000000000000 ) ) 
 REPRESENTATION_ITEM ( '' )  );
#4152 = PLANE ( 'NONE',  #16321 ) ;
#4153 = CARTESIAN_POINT ( 'NONE',  ( -0.5672860446885946706, -37.53182223685058716, -6.568693074176339408 ) ) ;
#4154 = DIRECTION ( 'NONE',  ( 1.333906992743555050E-23, -1.000000000000000000, 0.000000000000000000 ) ) ;
#4155 = AXIS2_PLACEMENT_3D ( 'NONE', #17900, #17664, #48915 ) ;
#4156 = ORIENTED_EDGE ( 'NONE', *, *, #13284, .F. ) ;
#4157 = VECTOR ( 'NONE', #45461, 1000.000000000000000 ) ;
#4158 = CARTESIAN_POINT ( 'NONE',  ( 155.0540265531850537, 2.143131898507880377E-16, 159.0682875569279702 ) ) ;
#4159 = ORIENTED_EDGE ( 'NONE', *, *, #3919, .F. ) ;
#4160 = FACE_OUTER_BOUND ( 'NONE', #16280, .T. ) ;
#4161 = VERTEX_POINT ( 'NONE', #19707 ) ;
#4162 = CARTESIAN_POINT ( 'NONE',  ( -44.94597344681493922, 2.143131898507880377E-16, 165.0000000000000000 ) ) ;
#4163 = LINE ( 'NONE', #39836, #23280 ) ;
#4164 = AXIS2_PLACEMENT_3D ( 'NONE', #38541, #22611, #3611 ) ;
#4165 = VECTOR ( 'NONE', #10960, 1000.000000000000000 ) ;
#4166 = CARTESIAN_POINT ( 'NONE',  ( 75.05402655318509630, 2.143131898507880377E-16, 42.56828755692799859 ) ) ;
#4167 = CARTESIAN_POINT ( 'NONE',  ( 135.0000000000012790, 17.00000000000000000, 5.000000000000004441 ) ) ;
#4168 = EDGE_LOOP ( 'NONE', ( #34605, #11609, #27626, #32368 ) ) ;
#4169 = CARTESIAN_POINT ( 'NONE',  ( -215.0000000000000568, 164.9999999999999716, 500.0000000000000000 ) ) ;
#4170 = CARTESIAN_POINT ( 'NONE',  ( 359.9999999999999432, 181.0000000000002274, -356.0000000000003411 ) ) ;
#4171 = ORIENTED_EDGE ( 'NONE', *, *, #43549, .T. ) ;
#4172 = LINE ( 'NONE', #19302, #49987 ) ;
#4173 = DIRECTION ( 'NONE',  ( 0.000000000000000000, -1.000000000000000000, 0.000000000000000000 ) ) ;
#4174 = CARTESIAN_POINT ( 'NONE',  ( 0.000000000000000000, 317.3964497041420145, 132.2485207100591253 ) ) ;
#4175 = CYLINDRICAL_SURFACE ( 'NONE', #39814, 1.750000000000001554 ) ;
#4176 = EDGE_LOOP ( 'NONE', ( #8785, #33695, #17889, #30160, #42386, #35308 ) ) ;
#4177 = ORIENTED_EDGE ( 'NONE', *, *, #34369, .F. ) ;
#4178 = CARTESIAN_POINT ( 'NONE',  ( 111.5540265531850537, -1.025126265847082108, -117.4317124430720440 ) ) ;
#4179 = EDGE_CURVE ( 'NONE', #48410, #42209, #3802, .T. ) ;
#4180 = ORIENTED_EDGE ( 'NONE', *, *, #37806, .F. ) ;
#4181 = CARTESIAN_POINT ( 'NONE',  ( -86.69597344681496054, 0.000000000000000000, 165.0000000000000000 ) ) ;
#4182 = DIRECTION ( 'NONE',  ( 0.000000000000000000, 2.969158215481698263E-48, -1.000000000000000000 ) ) ;
#4183 = DIRECTION ( 'NONE',  ( 0.000000000000000000, 0.000000000000000000, 1.000000000000000000 ) ) ;
#4184 = EDGE_LOOP ( 'NONE', ( #47272, #39256, #17712, #24398 ) ) ;
#4185 = CARTESIAN_POINT ( 'NONE',  ( 195.0540265531851105, 1.025126265847089657, 79.06828755692797017 ) ) ;
#4186 = EDGE_CURVE ( 'NONE', #6015, #18793, #33541, .T. ) ;
#4187 = ORIENTED_EDGE ( 'NONE', *, *, #21739, .T. ) ;
#4188 = CARTESIAN_POINT ( 'NONE',  ( -48.33712804702535948, -13.03701565032741527, -9.367992836599954742 ) ) ;
#4189 = EDGE_CURVE ( 'NONE', #32520, #12217, #8170, .T. ) ;
#4190 = CARTESIAN_POINT ( 'NONE',  ( -0.8603719846020866369, 1.073163306095949121, 9.972175347158394487 ) ) ;
#4191 = VECTOR ( 'NONE', #46469, 1000.000000000000000 ) ;
#4192 = EDGE_CURVE ( 'NONE', #26282, #2880, #7924, .T. ) ;
#4193 = FACE_OUTER_BOUND ( 'NONE', #37782, .T. ) ;
#4194 = VERTEX_POINT ( 'NONE', #39222 ) ;
#4195 = ORIENTED_EDGE ( 'NONE', *, *, #29985, .F. ) ;
#4196 = EDGE_LOOP ( 'NONE', ( #24393, #2122, #39598, #1151 ) ) ;
#4197 = CARTESIAN_POINT ( 'NONE',  ( -114.9999999999994031, 17.00000000000000000, -30.00000000000000000 ) ) ;
#4198 = PLANE ( 'NONE',  #5409 ) ;
#4199 = VECTOR ( 'NONE', #7271, 1000.000000000000000 ) ;
#4200 = LINE ( 'NONE', #3937, #14220 ) ;
#4201 = EDGE_CURVE ( 'NONE', #20632, #2059, #39478, .T. ) ;
#4202 = PRODUCT_DEFINITION_CONTEXT ( 'detailed design', #39776, 'design' ) ;
#4203 = ORIENTED_EDGE ( 'NONE', *, *, #5443, .T. ) ;
#4204 = CARTESIAN_POINT ( 'NONE',  ( 191.5540265531850537, 1.025126265847089213, -0.9317124430720324924 ) ) ;
#4205 = VECTOR ( 'NONE', #1202, 1000.000000000000000 ) ;
#4206 = ORIENTED_EDGE ( 'NONE', *, *, #20417, .T. ) ;
#4207 = CARTESIAN_POINT ( 'NONE',  ( 35.00000000000152767, 16.00000000000000000, 35.00000000000000000 ) ) ;
#4208 = EDGE_LOOP ( 'NONE', ( #18998, #37444, #48111, #24651 ) ) ;
#4209 =( NAMED_UNIT ( * ) SI_UNIT ( $, .STERADIAN. ) SOLID_ANGLE_UNIT ( ) );
#4210 = DIRECTION ( 'NONE',  ( -0.000000000000000000, -0.000000000000000000, -1.000000000000000000 ) ) ;
#4211 = FACE_OUTER_BOUND ( 'NONE', #5918, .T. ) ;
#4212 = CARTESIAN_POINT ( 'NONE',  ( -168.4459734468149463, 0.000000000000000000, -117.4317124430720725 ) ) ;
#4213 = CARTESIAN_POINT ( 'NONE',  ( 0.6665230861360139647, -1.119719016451030891, 9.961922210043265835 ) ) ;
#4214 = CARTESIAN_POINT ( 'NONE',  ( 1.249999999999999778, 0.000000000000000000, 3.333333333333333481 ) ) ;
#4215 = ORIENTED_EDGE ( 'NONE', *, *, #39352, .T. ) ;
#4216 = ORIENTED_EDGE ( 'NONE', *, *, #30705, .T. ) ;
#4217 = DIRECTION ( 'NONE',  ( 0.000000000000000000, -1.000000000000000000, 0.000000000000000000 ) ) ;
#4218 = DIRECTION ( 'NONE',  ( 0.000000000000000000, -0.000000000000000000, -1.000000000000000000 ) ) ;
#4219 = FACE_OUTER_BOUND ( 'NONE', #26773, .T. ) ;
#4220 = EDGE_CURVE ( 'NONE', #2364, #50479, #6082, .T. ) ;
#4221 = ADVANCED_FACE ( 'NONE', ( #27663 ), #23292, .T. ) ;
#4222 = EDGE_CURVE ( 'NONE', #593, #23700, #23817, .T. ) ;
#4223 = EDGE_CURVE ( 'NONE', #43883, #12455, #35884, .T. ) ;
#4224 = DIRECTION ( 'NONE',  ( -0.000000000000000000, -1.000000000000000000, -0.000000000000000000 ) ) ;
#4225 = CARTESIAN_POINT ( 'NONE',  ( -28.96803024440907137, -18.11533787072017176, 7.455576670931136185 ) ) ;
#4226 = EDGE_CURVE ( 'NONE', #11669, #31642, #27373, .T. ) ;
#4227 = ORIENTED_EDGE ( 'NONE', *, *, #1690, .T. ) ;
#4228 = DIRECTION ( 'NONE',  ( -0.000000000000000000, -0.000000000000000000, 1.000000000000000000 ) ) ;
#4229 = EDGE_CURVE ( 'NONE', #16113, #9008, #3218, .T. ) ;
#4230 = CARTESIAN_POINT ( 'NONE',  ( -165.6708471809677974, 1.750000000000009548, -158.1565861772249377 ) ) ;
#4231 = VECTOR ( 'NONE', #24839, 1000.000000000000000 ) ;
#4232 = ORIENTED_EDGE ( 'NONE', *, *, #23170, .F. ) ;
#4233 = DIRECTION ( 'NONE',  ( 1.586032892321652236E-16, 1.000000000000000000, 2.288264760618012091E-48 ) ) ;
#4234 = CYLINDRICAL_SURFACE ( 'NONE', #14707, 0.5000000000000004441 ) ;
#4235 = CARTESIAN_POINT ( 'NONE',  ( 35.00000000000216716, 16.00000000000000000, 95.00000000000000000 ) ) ;
#4236 = ORIENTED_EDGE ( 'NONE', *, *, #28320, .F. ) ;
#4237 = VECTOR ( 'NONE', #49541, 1000.000000000000000 ) ;
#4238 = EDGE_LOOP ( 'NONE', ( #17859, #49257, #27859, #523, #20517, #8561 ) ) ;
#4239 = EDGE_CURVE ( 'NONE', #5007, #44276, #10595, .T. ) ;
#4240 = CARTESIAN_POINT ( 'NONE',  ( 153.3040265531850537, 0.000000000000000000, 165.0000000000000000 ) ) ;
#4241 = EDGE_CURVE ( 'NONE', #24669, #43437, #22901, .T. ) ;
#4242 = ORIENTED_EDGE ( 'NONE', *, *, #17612, .F. ) ;
#4243 = EDGE_CURVE ( 'NONE', #15209, #25755, #24335, .T. ) ;
#4244 = ORIENTED_EDGE ( 'NONE', *, *, #18390, .F. ) ;
#4245 = CARTESIAN_POINT ( 'NONE',  ( 350.0000000000000000, 169.0000000000000000, -340.0000000000001705 ) ) ;
#4246 = DIRECTION ( 'NONE',  ( 1.000000000000000000, -0.000000000000000000, -0.000000000000000000 ) ) ;
#4247 = DIRECTION ( 'NONE',  ( 1.000000000000000000, 0.000000000000000000, 0.000000000000000000 ) ) ;
#4248 = DIRECTION ( 'NONE',  ( 0.000000000000000000, 0.000000000000000000, 1.000000000000000000 ) ) ;
#4249 = ORIENTED_EDGE ( 'NONE', *, *, #27985, .F. ) ;
#4250 = ORIENTED_EDGE ( 'NONE', *, *, #13132, .F. ) ;
#4251 = ORIENTED_EDGE ( 'NONE', *, *, #40268, .F. ) ;
#4252 = EDGE_CURVE ( 'NONE', #34485, #38451, #34569, .T. ) ;
#4253 = ORIENTED_EDGE ( 'NONE', *, *, #26768, .T. ) ;
#4254 = CARTESIAN_POINT ( 'NONE',  ( -2.538055338523177440, -50.00000000000000711, -9.367992836599954742 ) ) ;
#4255 = DIRECTION ( 'NONE',  ( -0.000000000000000000, -1.000000000000000000, -0.000000000000000000 ) ) ;
#4256 = ORIENTED_EDGE ( 'NONE', *, *, #50333, .T. ) ;
#4257 = VERTEX_POINT ( 'NONE', #38968 ) ;
#4258 = LINE ( 'NONE', #31728, #46709 ) ;
#4259 = CARTESIAN_POINT ( 'NONE',  ( -12.78770032058971395, -31.68259716188267916, 7.455576670931136185 ) ) ;
#4260 = AXIS2_PLACEMENT_3D ( 'NONE', #32923, #33666, #24959 ) ;
#4261 = FACE_OUTER_BOUND ( 'NONE', #9905, .T. ) ;
#4262 = ORIENTED_EDGE ( 'NONE', *, *, #19250, .F. ) ;
#4263 = VERTEX_POINT ( 'NONE', #1974 ) ;
#4264 = EDGE_CURVE ( 'NONE', #31874, #20963, #40978, .T. ) ;
#4265 = CARTESIAN_POINT ( 'NONE',  ( -69.99999999999940314, 17.00000000000000000, -30.00000000000000000 ) ) ;
#4266 =( LENGTH_UNIT ( ) NAMED_UNIT ( * ) SI_UNIT ( .MILLI., .METRE. ) );
#4267 = ORIENTED_EDGE ( 'NONE', *, *, #38433, .T. ) ;
#4268 = CARTESIAN_POINT ( 'NONE',  ( 181.0000000000000000, -270.4999999999999432, -339.9999999999998863 ) ) ;
#4269 = PLANE ( 'NONE',  #12903 ) ;
#4270 = CARTESIAN_POINT ( 'NONE',  ( -164.9999999999997442, 17.00000000000000000, -60.00000000000000000 ) ) ;
#4271 = VECTOR ( 'NONE', #567, 1000.000000000000000 ) ;
#4272 = EDGE_CURVE ( 'NONE', #27650, #39465, #17370, .T. ) ;
#4273 = CARTESIAN_POINT ( 'NONE',  ( 2.920962725444330221, 37.39284056564468983, -9.011255500499645521 ) ) ;
#4274 = ORIENTED_EDGE ( 'NONE', *, *, #33425, .T. ) ;
#4275 = CARTESIAN_POINT ( 'NONE',  ( -5.107674452599877846, 2.961810711069517765, 9.586754400233969520 ) ) ;
#4276 = DIRECTION ( 'NONE',  ( 0.4740998230350172427, -0.3386427307392981811, -0.8127425537743158124 ) ) ;
#4277 = CARTESIAN_POINT ( 'NONE',  ( 360.0000000000000568, 175.0000000000000284, -94.00000000000019895 ) ) ;
#4278 = CARTESIAN_POINT ( 'NONE',  ( 341.9999999999999432, 181.0000000000001705, -356.0000000000003411 ) ) ;
#4279 = EDGE_CURVE ( 'NONE', #17107, #19110, #46657, .T. ) ;
#4280 = EDGE_CURVE ( 'NONE', #23932, #38451, #17620, .T. ) ;
#4281 = MANIFOLD_SOLID_BREP ( 'Cut-Extrude1[2]', #49809 ) ;
#4282 = CARTESIAN_POINT ( 'NONE',  ( 10.25676241992214877, 8.638513918217338272, 18.89424093979656405 ) ) ;
#4283 = ADVANCED_FACE ( 'NONE', ( #13255 ), #28920, .F. ) ;
#4284 = CARTESIAN_POINT ( 'NONE',  ( 1.035950918207909632, 33.23661552194049307, -2.408242355805840784 ) ) ;
#4285 = CARTESIAN_POINT ( 'NONE',  ( 8.569579719062522472, 5.179646911086180694, 3.092310436554641662 ) ) ;
#4286 = ADVANCED_FACE ( 'NONE', ( #45046 ), #48875, .T. ) ;
#4287 =( BOUNDED_CURVE ( )  B_SPLINE_CURVE ( 3, ( #46835, #31496, #30991, #11729 ),
 .UNSPECIFIED., .F., .F. ) 
 B_SPLINE_CURVE_WITH_KNOTS ( ( 4, 4 ),
 ( 0.000000000000000000, 1.570796326794896780 ),
 .UNSPECIFIED. ) 
 CURVE ( )  GEOMETRIC_REPRESENTATION_ITEM ( )  RATIONAL_B_SPLINE_CURVE ( ( 1.000000000000000000, 0.8047378541243649375, 0.8047378541243649375, 1.000000000000000000 ) ) 
 REPRESENTATION_ITEM ( '' )  );
#4288 = ORIENTED_EDGE ( 'NONE', *, *, #778, .F. ) ;
#4289 = CARTESIAN_POINT ( 'NONE',  ( 153.3040265531850537, 0.000000000000000000, 165.0000000000000000 ) ) ;
#4290 = AXIS2_PLACEMENT_3D ( 'NONE', #33802, #49390, #34296 ) ;
#4291 = ORIENTED_EDGE ( 'NONE', *, *, #40242, .T. ) ;
#4292 = DIRECTION ( 'NONE',  ( -0.000000000000000000, -0.000000000000000000, -1.000000000000000000 ) ) ;
#4293 = CARTESIAN_POINT ( 'NONE',  ( 210.0000000000000568, 0.000000000000000000, -157.4317124430720298 ) ) ;
#4294 =( BOUNDED_CURVE ( )  B_SPLINE_CURVE ( 3, ( #13777, #40240, #48391, #28937 ),
 .UNSPECIFIED., .F., .F. ) 
 B_SPLINE_CURVE_WITH_KNOTS ( ( 4, 4 ),
 ( 1.570796326794896558, 3.141592653589793116 ),
 .UNSPECIFIED. ) 
 CURVE ( )  GEOMETRIC_REPRESENTATION_ITEM ( )  RATIONAL_B_SPLINE_CURVE ( ( 1.000000000000000000, 0.8047378541243649375, 0.8047378541243649375, 1.000000000000000000 ) ) 
 REPRESENTATION_ITEM ( '' )  );
#4295 = AXIS2_PLACEMENT_3D ( 'NONE', #31411, #34496, #46745 ) ;
#4296 = ORIENTED_EDGE ( 'NONE', *, *, #23738, .F. ) ;
#4297 = CARTESIAN_POINT ( 'NONE',  ( -164.9459734468149463, -1.025126265847089435, -40.93171244307204404 ) ) ;
#4298 = ORIENTED_EDGE ( 'NONE', *, *, #23675, .T. ) ;
#4299 = ORIENTED_EDGE ( 'NONE', *, *, #6752, .F. ) ;
#4300 = CARTESIAN_POINT ( 'NONE',  ( 0.3862712429686978033, -1.188820645368937834, -3.333333333333333481 ) ) ;
#4301 = AXIS2_PLACEMENT_3D ( 'NONE', #34514, #22695, #42690 ) ;
#4302 = CARTESIAN_POINT ( 'NONE',  ( 113.3040265531850537, 0.000000000000000000, 165.0000000000000000 ) ) ;
#4303 = ORIENTED_EDGE ( 'NONE', *, *, #2658, .F. ) ;
#4304 = ADVANCED_FACE ( 'NONE', ( #28668 ), #44009, .T. ) ;
#4305 = VECTOR ( 'NONE', #10915, 1000.000000000000000 ) ;
#4306 = DIRECTION ( 'NONE',  ( 0.000000000000000000, 1.000000000000000000, 0.000000000000000000 ) ) ;
#4307 = CARTESIAN_POINT ( 'NONE',  ( -64.99999999999877787, 17.00000000000000000, 5.000000000000004441 ) ) ;
#4308 =( BOUNDED_CURVE ( )  B_SPLINE_CURVE ( 3, ( #44547, #5577, #21232, #17383 ),
 .UNSPECIFIED., .F., .F. ) 
 B_SPLINE_CURVE_WITH_KNOTS ( ( 4, 4 ),
 ( 1.570796326794896558, 3.141592653589793116 ),
 .UNSPECIFIED. ) 
 CURVE ( )  GEOMETRIC_REPRESENTATION_ITEM ( )  RATIONAL_B_SPLINE_CURVE ( ( 1.000000000000000000, 0.8047378541243649375, 0.8047378541243649375, 1.000000000000000000 ) ) 
 REPRESENTATION_ITEM ( '' )  );
#4309 = DIRECTION ( 'NONE',  ( 0.000000000000000000, 0.000000000000000000, 1.000000000000000000 ) ) ;
#4310 = ORIENTED_EDGE ( 'NONE', *, *, #9209, .F. ) ;
#4311 = B_SPLINE_CURVE_WITH_KNOTS ( 'NONE', 3,
 ( #39254, #4353, #8206, #47649 ),
 .UNSPECIFIED., .F., .F.,
 ( 4, 4 ),
 ( 0.000000000000000000, 2.647279941188464684E-05 ),
 .UNSPECIFIED. ) ;
#4312 = FACE_OUTER_BOUND ( 'NONE', #10861, .T. ) ;
#4313 = CARTESIAN_POINT ( 'NONE',  ( 185.0000000000000000, -256.4999999999999432, -339.9999999999999432 ) ) ;
#4314 = CARTESIAN_POINT ( 'NONE',  ( -1.337801958641930300, -1.088266084286974689, 9.928159647716134018 ) ) ;
#4315 = ORIENTED_EDGE ( 'NONE', *, *, #13029, .T. ) ;
#4316 = CARTESIAN_POINT ( 'NONE',  ( 210.0000000000000568, 2.143131898507881116E-16, 39.06828755692797728 ) ) ;
#4317 = CARTESIAN_POINT ( 'NONE',  ( -64.99999999999846523, 16.00000000000000000, 35.00000000000000000 ) ) ;
#4318 = ORIENTED_EDGE ( 'NONE', *, *, #1857, .T. ) ;
#4319 = ORIENTED_EDGE ( 'NONE', *, *, #5775, .F. ) ;
#4320 = ORIENTED_EDGE ( 'NONE', *, *, #23459, .T. ) ;
#4321 = LINE ( 'NONE', #7154, #18025 ) ;
#4322 = VECTOR ( 'NONE', #22280, 1000.000000000000000 ) ;
#4323 = DIRECTION ( 'NONE',  ( 2.874857526315639190E-31, -1.000000000000000000, 2.537652627714642000E-15 ) ) ;
#4324 = ORIENTED_EDGE ( 'NONE', *, *, #13583, .F. ) ;
#4325 = DIRECTION ( 'NONE',  ( -1.000000000000000000, 0.000000000000000000, 0.000000000000000000 ) ) ;
#4326 = PLANE ( 'NONE',  #4920 ) ;
#4327 = FACE_OUTER_BOUND ( 'NONE', #11889, .T. ) ;
#4328 = DIRECTION ( 'NONE',  ( 0.000000000000000000, -1.000000000000000000, 0.000000000000000000 ) ) ;
#4329 = DIRECTION ( 'NONE',  ( 0.4436251537532894806, 0.000000000000000000, 0.8962124318248270161 ) ) ;
#4330 = CARTESIAN_POINT ( 'NONE',  ( 3.996390545799824334, -16.57371371864897469, 8.953103998512858652 ) ) ;
#4331 = CARTESIAN_POINT ( 'NONE',  ( -3.798817505216114387, -5.709742178110357891, 9.753789706659947711 ) ) ;
#4332 = CARTESIAN_POINT ( 'NONE',  ( 1.655785408456140084, 0.7536129375913136474, 9.903764339332061795 ) ) ;
#4333 = VECTOR ( 'NONE', #6399, 1000.000000000000000 ) ;
#4334 = CARTESIAN_POINT ( 'NONE',  ( -4.945973446814917018, 1.025126265847096985, -0.9317124430720461481 ) ) ;
#4335 = LINE ( 'NONE', #3820, #11721 ) ;
#4336 = DIRECTION ( 'NONE',  ( -1.586032880504786307E-16, 1.654361225106055350E-24, -1.000000000000000000 ) ) ;
#4337 = VECTOR ( 'NONE', #17722, 1000.000000000000000 ) ;
#4338 = LINE ( 'NONE', #16901, #24087 ) ;
#4339 = CARTESIAN_POINT ( 'NONE',  ( -124.9459734468149463, 2.143131898507847836E-16, 42.56828755692795596 ) ) ;
#4340 = EDGE_CURVE ( 'NONE', #39670, #46399, #48119, .T. ) ;
#4341 = EDGE_CURVE ( 'NONE', #22510, #5553, #36863, .T. ) ;
#4342 = CARTESIAN_POINT ( 'NONE',  ( -205.6708471809678827, -1.750000000000009548, 39.79316129108089228 ) ) ;
#4343 = CARTESIAN_POINT ( 'NONE',  ( 153.3040265531850537, 1.750000000000010658, 120.8182875569279702 ) ) ;
#4344 = EDGE_LOOP ( 'NONE', ( #19608, #49372, #18854, #12937, #4227, #10937, #4320, #34801 ) ) ;
#4345 = DIRECTION ( 'NONE',  ( 1.000000000000000000, 0.000000000000000000, 0.000000000000000000 ) ) ;
#4346 = EDGE_CURVE ( 'NONE', #23180, #25776, #50129, .T. ) ;
#4347 = CARTESIAN_POINT ( 'NONE',  ( -28.96803024440907137, -18.11533787072017176, 7.455576670931136185 ) ) ;
#4348 = CARTESIAN_POINT ( 'NONE',  ( 3.345242017215822372, -2.159124855890657724, -4.878909776184769953E-16 ) ) ;
#4349 = CARTESIAN_POINT ( 'NONE',  ( -33.64889274059387958, 3.704246042440976439, 8.356839323120299312 ) ) ;
#4350 = EDGE_CURVE ( 'NONE', #24372, #46042, #30176, .T. ) ;
#4351 = ADVANCED_FACE ( 'NONE', ( #49381 ), #30436, .F. ) ;
#4352 = VERTEX_POINT ( 'NONE', #18364 ) ;
#4353 = CARTESIAN_POINT ( 'NONE',  ( -0.9985466430029077411, -1.124040728744828188, 9.944962737616616977 ) ) ;
#4354 = EDGE_LOOP ( 'NONE', ( #8608, #27915, #8498, #19628 ) ) ;
#4355 = CARTESIAN_POINT ( 'NONE',  ( 49.46074318306830975, -9.578883844006833570, 8.807470649214879543 ) ) ;
#4356 = EDGE_LOOP ( 'NONE', ( #33297, #34547, #24964, #35461 ) ) ;
#4357 = CARTESIAN_POINT ( 'NONE',  ( 181.0000000000000000, -272.5000000000000000, -110.9999999999999005 ) ) ;
#4358 = CARTESIAN_POINT ( 'NONE',  ( 75.05402655318509630, 2.143131898507880377E-16, -40.93171244307205825 ) ) ;
#4359 = CARTESIAN_POINT ( 'NONE',  ( 4.204997580903515164, -7.388441598285492518, 229.0000000000000000 ) ) ;
#4360 = EDGE_CURVE ( 'NONE', #36853, #40426, #11940, .T. ) ;
#4361 = VERTEX_POINT ( 'NONE', #26338 ) ;
#4362 = CARTESIAN_POINT ( 'NONE',  ( 33.26055721649974117, 17.33465289285476985, 8.506357886886741326 ) ) ;
#4363 = ORIENTED_EDGE ( 'NONE', *, *, #39990, .F. ) ;
#4364 = ORIENTED_EDGE ( 'NONE', *, *, #12501, .T. ) ;
#4365 = CYLINDRICAL_SURFACE ( 'NONE', #11434, 1.750000000000008438 ) ;
#4366 = CARTESIAN_POINT ( 'NONE',  ( -84.94597344681494633, 2.143131898507880377E-16, 122.5682875569279702 ) ) ;
#4367 = ORIENTED_EDGE ( 'NONE', *, *, #12538, .F. ) ;
#4368 = DIRECTION ( 'NONE',  ( 0.000000000000000000, 0.000000000000000000, 1.000000000000000000 ) ) ;
#4369 = CARTESIAN_POINT ( 'NONE',  ( -5.670847180967843570, 1.750000000000023315, -38.15658617722493062 ) ) ;
#4370 = DIRECTION ( 'NONE',  ( -1.000000000000000000, -0.000000000000000000, -0.000000000000000000 ) ) ;
#4371 = CARTESIAN_POINT ( 'NONE',  ( -88.44597344681494633, -1.025126265847089213, 162.5682875569279133 ) ) ;
#4372 = FACE_OUTER_BOUND ( 'NONE', #5239, .T. ) ;
#4373 = ORIENTED_EDGE ( 'NONE', *, *, #17362, .F. ) ;
#4374 = DIRECTION ( 'NONE',  ( -0.000000000000000000, -0.000000000000000000, 1.000000000000000000 ) ) ;
#4375 = LINE ( 'NONE', #35702, #16325 ) ;
#4376 = VERTEX_POINT ( 'NONE', #22480 ) ;
#4377 = CARTESIAN_POINT ( 'NONE',  ( -15.00000000000001421, 17.00000000000000000, -90.00000000000000000 ) ) ;
#4378 = CARTESIAN_POINT ( 'NONE',  ( -64.99999999999846523, 16.00000000000000000, 35.00000000000000000 ) ) ;
#4379 = B_SPLINE_SURFACE_WITH_KNOTS ( 'NONE', 3, 3, ( 
 ( #20646, #28352, #12192, #36321 ),
 ( #43734, #8603, #1415, #8355 ),
 ( #24258, #39914, #48302, #9106 ),
 ( #1164, #36064, #47804, #13196 ) ),
 .UNSPECIFIED., .F., .F., .F.,
 ( 4, 4 ),
 ( 4, 4 ),
 ( 0.000000000000000000, 1.000000000000000000 ),
 ( 0.000000000000000000, 1.000000000000000000 ),
 .UNSPECIFIED. ) ;
#4380 = ORIENTED_EDGE ( 'NONE', *, *, #427, .T. ) ;
#4381 = EDGE_CURVE ( 'NONE', #37527, #20642, #38155, .T. ) ;
#4382 = CARTESIAN_POINT ( 'NONE',  ( 46.11867747200574286, -19.86470446310233129, -8.016098858316205167 ) ) ;
#4383 = CARTESIAN_POINT ( 'NONE',  ( -165.0000000000000284, 16.00000000000000000, 115.0000000000000142 ) ) ;
#4384 = DIRECTION ( 'NONE',  ( -1.000000000000000000, 0.000000000000000000, -0.000000000000000000 ) ) ;
#4385 = CARTESIAN_POINT ( 'NONE',  ( 350.0000000000000000, 169.0000000000000000, -344.0000000000001705 ) ) ;
#4386 = EDGE_LOOP ( 'NONE', ( #15931, #16609, #44113, #2724, #14117 ) ) ;
#4387 =( BOUNDED_CURVE ( )  B_SPLINE_CURVE ( 3, ( #45771, #6555, #25809, #21695 ),
 .UNSPECIFIED., .F., .F. ) 
 B_SPLINE_CURVE_WITH_KNOTS ( ( 4, 4 ),
 ( 4.712388980384689674, 6.283185307179586232 ),
 .UNSPECIFIED. ) 
 CURVE ( )  GEOMETRIC_REPRESENTATION_ITEM ( )  RATIONAL_B_SPLINE_CURVE ( ( 1.000000000000000000, 0.8047378541243649375, 0.8047378541243649375, 1.000000000000000000 ) ) 
 REPRESENTATION_ITEM ( '' )  );
#4388 = FACE_OUTER_BOUND ( 'NONE', #1120, .T. ) ;
#4389 = DIRECTION ( 'NONE',  ( 4.625929269271635797E-16, -0.000000000000000000, 1.000000000000000000 ) ) ;
#4390 = FACE_OUTER_BOUND ( 'NONE', #29976, .T. ) ;
#4391 = ORIENTED_EDGE ( 'NONE', *, *, #6692, .F. ) ;
#4392 = VERTEX_POINT ( 'NONE', #34546 ) ;
#4393 = DIRECTION ( 'NONE',  ( -1.744108391771820078E-14, 1.702437461333236238E-17, -1.000000000000000000 ) ) ;
#4394 = CARTESIAN_POINT ( 'NONE',  ( 6.208157169185024138, -36.98937201184289592, 8.506357886886741326 ) ) ;
#4395 = DIRECTION ( 'NONE',  ( 0.000000000000000000, -0.2223603367690619725, -0.9749645535258958384 ) ) ;
#4396 = CARTESIAN_POINT ( 'NONE',  ( -1.011271242968683426, -0.7347315653655928092, -3.333333333333333481 ) ) ;
#4397 = CIRCLE ( 'NONE', #28174, 2.000000000000001776 ) ;
#4398 = CARTESIAN_POINT ( 'NONE',  ( 31.44259251615245887, 38.95901822126168668, -9.367992836599954742 ) ) ;
#4399 = EDGE_LOOP ( 'NONE', ( #26499, #28171, #23925, #10924 ) ) ;
#4400 = DIRECTION ( 'NONE',  ( -0.000000000000000000, -0.000000000000000000, -1.000000000000000000 ) ) ;
#4401 = AXIS2_PLACEMENT_3D ( 'NONE', #11536, #38995, #14870 ) ;
#4402 = PLANE ( 'NONE',  #40097 ) ;
#4403 = CARTESIAN_POINT ( 'NONE',  ( -166.6959734468149463, 1.750000000000009992, 160.8182875569279702 ) ) ;
#4404 =( GEOMETRIC_REPRESENTATION_CONTEXT ( 3 ) GLOBAL_UNCERTAINTY_ASSIGNED_CONTEXT ( ( #35331 ) ) GLOBAL_UNIT_ASSIGNED_CONTEXT ( ( #46966, #14238, #23660 ) ) REPRESENTATION_CONTEXT ( 'NONE', 'WORKASPACE' ) );
#4405 = DIRECTION ( 'NONE',  ( -1.000000000000000000, 0.000000000000000000, 0.000000000000000000 ) ) ;
#4406 = AXIS2_PLACEMENT_3D ( 'NONE', #30267, #45123, #10264 ) ;
#4407 = ORIENTED_EDGE ( 'NONE', *, *, #29641, .T. ) ;
#4408 = CARTESIAN_POINT ( 'NONE',  ( 191.5540265531851105, 0.000000000000000000, 119.0682875569279702 ) ) ;
#4409 = ORIENTED_EDGE ( 'NONE', *, *, #3297, .F. ) ;
#4410 = CARTESIAN_POINT ( 'NONE',  ( -19.99999999999908695, 17.00000000000000000, 0.000000000000000000 ) ) ;
#4411 = ORIENTED_EDGE ( 'NONE', *, *, #29292, .T. ) ;
#4412 = ADVANCED_FACE ( 'NONE', ( #25833 ), #26587, .F. ) ;
#4413 = CARTESIAN_POINT ( 'NONE',  ( -208.1473046169136580, 160.1880105690400171, 22.84256005001721945 ) ) ;
#4414 = CARTESIAN_POINT ( 'NONE',  ( 21.61731705588930907, 25.43568671410602278, -9.367992836599954742 ) ) ;
#4415 = CARTESIAN_POINT ( 'NONE',  ( 31.55402655318503236, 0.000000000000000000, 165.0000000000000000 ) ) ;
#4416 = CARTESIAN_POINT ( 'NONE',  ( -4.945973446814917018, -1.025126265847096763, -157.4317124430720014 ) ) ;
#4417 = ORIENTED_EDGE ( 'NONE', *, *, #3337, .T. ) ;
#4418 = VECTOR ( 'NONE', #39610, 1000.000000000000000 ) ;
#4419 = LINE ( 'NONE', #43404, #4847 ) ;
#4420 = CARTESIAN_POINT ( 'NONE',  ( -194.9999999999999432, 173.0000000000000000, 352.0000000000000000 ) ) ;
#4421 = VERTEX_POINT ( 'NONE', #18617 ) ;
#4422 = CARTESIAN_POINT ( 'NONE',  ( 343.9999999999993747, -183.0000000000000000, 357.9999999999998295 ) ) ;
#4423 = CARTESIAN_POINT ( 'NONE',  ( -4.945973446814903696, 2.143131898507912917E-16, -160.9317124430720582 ) ) ;
#4424 = CARTESIAN_POINT ( 'NONE',  ( 210.0000000000000568, 0.000000000000000000, -117.4317124430720298 ) ) ;
#4425 = CYLINDRICAL_SURFACE ( 'NONE', #17665, 2.000000000000001776 ) ;
#4426 = VERTEX_POINT ( 'NONE', #7092 ) ;
#4427 = ORIENTED_EDGE ( 'NONE', *, *, #32748, .F. ) ;
#4428 = CARTESIAN_POINT ( 'NONE',  ( 155.0540265531850537, 1.025126265847089435, -40.93171244307204404 ) ) ;
#4429 = ORIENTED_EDGE ( 'NONE', *, *, #28643, .T. ) ;
#4430 = CARTESIAN_POINT ( 'NONE',  ( 193.3040265531851105, 1.750000000000010658, -79.18171244307201562 ) ) ;
#4431 = CARTESIAN_POINT ( 'NONE',  ( 15.00000000000000000, 13.48684210526315930, 19.37312575500900280 ) ) ;
#4432 = AXIS2_PLACEMENT_3D ( 'NONE', #2095, #16985, #13124 ) ;
#4433 = DIRECTION ( 'NONE',  ( 1.612977847700450206E-50, 0.000000000000000000, -1.000000000000000000 ) ) ;
#4434 = ORIENTED_EDGE ( 'NONE', *, *, #15392, .T. ) ;
#4435 = DIRECTION ( 'NONE',  ( -1.586032892321652236E-16, -1.000000000000000000, -2.288264760618012091E-48 ) ) ;
#4436 = CIRCLE ( 'NONE', #38068, 2.000000000000001776 ) ;
#4437 = ORIENTED_EDGE ( 'NONE', *, *, #27623, .T. ) ;
#4438 =( GEOMETRIC_REPRESENTATION_CONTEXT ( 3 ) GLOBAL_UNCERTAINTY_ASSIGNED_CONTEXT ( ( #23426 ) ) GLOBAL_UNIT_ASSIGNED_CONTEXT ( ( #10973, #50166, #38953 ) ) REPRESENTATION_CONTEXT ( 'NONE', 'WORKASPACE' ) );
#4439 = EDGE_CURVE ( 'NONE', #17801, #46696, #11200, .T. ) ;
#4440 = CARTESIAN_POINT ( 'NONE',  ( -18.38319608353667434, 32.68498281710182596, -8.192531242611268638 ) ) ;
#4441 =( BOUNDED_CURVE ( )  B_SPLINE_CURVE ( 3, ( #14906, #38777, #45917, #33911 ),
 .UNSPECIFIED., .F., .F. ) 
 B_SPLINE_CURVE_WITH_KNOTS ( ( 4, 4 ),
 ( 4.712388980384689674, 6.283185307179586232 ),
 .UNSPECIFIED. ) 
 CURVE ( )  GEOMETRIC_REPRESENTATION_ITEM ( )  RATIONAL_B_SPLINE_CURVE ( ( 1.000000000000000000, 0.8047378541243649375, 0.8047378541243649375, 1.000000000000000000 ) ) 
 REPRESENTATION_ITEM ( '' )  );
#4442 = CARTESIAN_POINT ( 'NONE',  ( 185.0000000000000000, -180.9999999999999716, -350.0000000000001705 ) ) ;
#4443 = EDGE_LOOP ( 'NONE', ( #39054, #15018, #25441, #37982 ) ) ;
#4444 = VERTEX_POINT ( 'NONE', #2721 ) ;
#4445 = MANIFOLD_SOLID_BREP ( 'Square tube 20 X 20 X 2(1)[10]', #47371 ) ;
#4446 = VERTEX_POINT ( 'NONE', #10929 ) ;
#4447 = LINE ( 'NONE', #35513, #5019 ) ;
#4448 = CARTESIAN_POINT ( 'NONE',  ( 339.9999999999998863, -181.0000000000001990, -356.0000000000003411 ) ) ;
#4449 =( BOUNDED_CURVE ( )  B_SPLINE_CURVE ( 3, ( #49921, #38208, #6880, #2266 ),
 .UNSPECIFIED., .F., .F. ) 
 B_SPLINE_CURVE_WITH_KNOTS ( ( 4, 4 ),
 ( 4.712388980384689674, 6.283185307179586232 ),
 .UNSPECIFIED. ) 
 CURVE ( )  GEOMETRIC_REPRESENTATION_ITEM ( )  RATIONAL_B_SPLINE_CURVE ( ( 1.000000000000000000, 0.8047378541243649375, 0.8047378541243649375, 1.000000000000000000 ) ) 
 REPRESENTATION_ITEM ( '' )  );
#4450 = FACE_OUTER_BOUND ( 'NONE', #35951, .T. ) ;
#4451 = ORIENTED_EDGE ( 'NONE', *, *, #45572, .F. ) ;
#4452 = VERTEX_POINT ( 'NONE', #18864 ) ;
#4453 = FACE_OUTER_BOUND ( 'NONE', #30124, .T. ) ;
#4454 = ORIENTED_EDGE ( 'NONE', *, *, #16913, .F. ) ;
#4455 = PLANE ( 'NONE',  #8129 ) ;
#4456 = CARTESIAN_POINT ( 'NONE',  ( -8.445973446814964092, 1.025126265847097207, -117.4317124430720014 ) ) ;
#4457 = CARTESIAN_POINT ( 'NONE',  ( 350.0000000000000000, 165.0000000000000000, -340.0000000000001705 ) ) ;
#4458 = CIRCLE ( 'NONE', #13457, 0.5000000000000004441 ) ;
#4459 = SURFACE_SIDE_STYLE ('',( #876 ) ) ;
#4460 = FACE_OUTER_BOUND ( 'NONE', #3484, .T. ) ;
#4461 = CARTESIAN_POINT ( 'NONE',  ( 1.011271242968677653, 0.7347315653656002477, 10.00000000000000000 ) ) ;
#4462 = VERTEX_POINT ( 'NONE', #30698 ) ;
#4463 = ORIENTED_EDGE ( 'NONE', *, *, #9414, .F. ) ;
#4464 = CARTESIAN_POINT ( 'NONE',  ( 153.3040265531850537, 0.000000000000000000, 165.0000000000000000 ) ) ;
#4465 = CARTESIAN_POINT ( 'NONE',  ( 224.9999999999999432, -175.0000000000000000, 0.000000000000000000 ) ) ;
#4466 = FACE_OUTER_BOUND ( 'NONE', #46897, .T. ) ;
#4467 = CARTESIAN_POINT ( 'NONE',  ( -84.94597344681494633, 2.143131898507880377E-16, -117.4317124430720725 ) ) ;
#4468 = ORIENTED_EDGE ( 'NONE', *, *, #31539, .T. ) ;
#4469 = EDGE_CURVE ( 'NONE', #14362, #45172, #37649, .T. ) ;
#4470 = LINE ( 'NONE', #47025, #32763 ) ;
#4471 = CARTESIAN_POINT ( 'NONE',  ( -168.4459734468149463, 0.000000000000000000, 119.0682875569279702 ) ) ;
#4472 = VECTOR ( 'NONE', #46300, 1000.000000000000000 ) ;
#4473 = VERTEX_POINT ( 'NONE', #10428 ) ;
#4474 = CARTESIAN_POINT ( 'NONE',  ( -2.538055338523177440, -33.28424297489108596, -9.367992836599954742 ) ) ;
#4475 = LINE ( 'NONE', #42450, #21265 ) ;
#4476 = CARTESIAN_POINT ( 'NONE',  ( 46.76852358249013264, -17.86468378716708827, -9.367992836599951190 ) ) ;
#4477 = EDGE_CURVE ( 'NONE', #4444, #24185, #33794, .T. ) ;
#4478 = ADVANCED_FACE ( 'NONE', ( #11959 ), #410, .T. ) ;
#4479 = ORIENTED_EDGE ( 'NONE', *, *, #24296, .T. ) ;
#4480 = ORIENTED_EDGE ( 'NONE', *, *, #45948, .F. ) ;
#4481 = CARTESIAN_POINT ( 'NONE',  ( 169.0000000000000000, 2.775557561562891351E-14, -97.00000000000014211 ) ) ;
#4482 = EDGE_CURVE ( 'NONE', #29168, #9976, #32238, .T. ) ;
#4483 = CARTESIAN_POINT ( 'NONE',  ( 30.21887974406487487, -14.69854701517530060, -8.016098858316199838 ) ) ;
#4484 = EDGE_CURVE ( 'NONE', #17776, #17128, #20147, .T. ) ;
#4485 = VECTOR ( 'NONE', #38359, 1000.000000000000000 ) ;
#4486 = VERTEX_POINT ( 'NONE', #8611 ) ;
#4487 = ORIENTED_EDGE ( 'NONE', *, *, #20206, .F. ) ;
#4488 = CARTESIAN_POINT ( 'NONE',  ( 169.0000000000000284, 175.0000000000000284, 357.9999999999998863 ) ) ;
#4489 = CARTESIAN_POINT ( 'NONE',  ( 165.0000000000000284, 175.0000000000000284, 339.9999999999998863 ) ) ;
#4490 = FACE_OUTER_BOUND ( 'NONE', #5885, .T. ) ;
#4491 = CARTESIAN_POINT ( 'NONE',  ( 339.9999999999999432, 174.9999999999996589, -344.0000000000002842 ) ) ;
#4492 = CARTESIAN_POINT ( 'NONE',  ( 111.5540265531850537, -1.025126265847081886, -120.9317124430720440 ) ) ;
#4493 = ORIENTED_EDGE ( 'NONE', *, *, #41816, .F. ) ;
#4494 = VECTOR ( 'NONE', #21822, 1000.000000000000000 ) ;
#4495 = VERTEX_POINT ( 'NONE', #7864 ) ;
#4496 = ORIENTED_EDGE ( 'NONE', *, *, #7218, .F. ) ;
#4497 = EDGE_CURVE ( 'NONE', #20753, #29288, #19415, .T. ) ;
#4498 = EDGE_CURVE ( 'NONE', #4914, #35123, #27673, .T. ) ;
#4499 = CARTESIAN_POINT ( 'NONE',  ( -50.11058929355266400, 7.578863168071933387, 7.455576670931136185 ) ) ;
#4500 = EDGE_CURVE ( 'NONE', #24077, #6277, #35834, .T. ) ;
#4501 = ORIENTED_EDGE ( 'NONE', *, *, #7966, .F. ) ;
#4502 = EDGE_CURVE ( 'NONE', #26902, #39708, #9681, .T. ) ;
#4503 = CARTESIAN_POINT ( 'NONE',  ( 1.045807400993768788, -0.6549210616167769894, 9.969907203203808521 ) ) ;
#4504 = VECTOR ( 'NONE', #50122, 1000.000000000000000 ) ;
#4505 = ORIENTED_EDGE ( 'NONE', *, *, #18934, .T. ) ;
#4506 = ORIENTED_EDGE ( 'NONE', *, *, #50675, .F. ) ;
#4507 = CARTESIAN_POINT ( 'NONE',  ( 1.632255792517797621, -3.624924591517686867, 3.247138655587366696 ) ) ;
#4508 =( NAMED_UNIT ( * ) PLANE_ANGLE_UNIT ( ) SI_UNIT ( $, .RADIAN. ) );
#4509 = EDGE_CURVE ( 'NONE', #28907, #572, #16058, .T. ) ;
#4510 = CARTESIAN_POINT ( 'NONE',  ( -210.0000000000000568, 0.000000000000000000, 42.56828755692799149 ) ) ;
#4511 = ORIENTED_EDGE ( 'NONE', *, *, #21469, .T. ) ;
#4512 = ORIENTED_EDGE ( 'NONE', *, *, #15506, .T. ) ;
#4513 = CARTESIAN_POINT ( 'NONE',  ( 0.1287570809895575430, 0.3962735484563150168, 10.00000000000000000 ) ) ;
#4514 = LINE ( 'NONE', #20402, #1033 ) ;
#4515 = ORIENTED_EDGE ( 'NONE', *, *, #45651, .F. ) ;
#4516 = DIRECTION ( 'NONE',  ( -1.000000000000000000, -0.000000000000000000, -0.000000000000000000 ) ) ;
#4517 = DIRECTION ( 'NONE',  ( -0.000000000000000000, -0.000000000000000000, -1.000000000000000000 ) ) ;
#4518 = LINE ( 'NONE', #47068, #26246 ) ;
#4519 = CARTESIAN_POINT ( 'NONE',  ( 17.51065725283126895, -28.41934970907778890, -9.367992836599954742 ) ) ;
#4520 = ORIENTED_EDGE ( 'NONE', *, *, #46000, .T. ) ;
#4521 = DIRECTION ( 'NONE',  ( 0.000000000000000000, 0.000000000000000000, -1.000000000000000000 ) ) ;
#4522 = CARTESIAN_POINT ( 'NONE',  ( 191.5540265531851105, 0.000000000000000000, -120.9317124430720156 ) ) ;
#4523 = DIRECTION ( 'NONE',  ( -3.469446951953611724E-16, 0.000000000000000000, 1.000000000000000000 ) ) ;
#4524 = EDGE_CURVE ( 'NONE', #11547, #22255, #39599, .T. ) ;
#4525 = CARTESIAN_POINT ( 'NONE',  ( 356.0000000000000000, 167.0000000000001990, -342.0000000000002842 ) ) ;
#4526 = AXIS2_PLACEMENT_3D ( 'NONE', #4542, #24311, #17847 ) ;
#4527 = EDGE_CURVE ( 'NONE', #32976, #22529, #35573, .T. ) ;
#4528 = EDGE_CURVE ( 'NONE', #25778, #15830, #47310, .T. ) ;
#4529 = AXIS2_PLACEMENT_3D ( 'NONE', #32510, #24796, #12227 ) ;
#4530 = DIRECTION ( 'NONE',  ( -1.000000000000000000, 0.000000000000000000, -7.793956916774525800E-48 ) ) ;
#4531 = ADVANCED_FACE ( 'NONE', ( #39165 ), #15798, .T. ) ;
#4532 = DIRECTION ( 'NONE',  ( -0.000000000000000000, 1.544785076050074834E-48, 1.000000000000000000 ) ) ;
#4533 = CARTESIAN_POINT ( 'NONE',  ( -0.7455485644579464832, -0.9687920084208885285, 9.987567862361071747 ) ) ;
#4534 = EDGE_CURVE ( 'NONE', #40413, #41767, #47563, .T. ) ;
#4535 = ORIENTED_EDGE ( 'NONE', *, *, #22988, .F. ) ;
#4536 = AXIS2_PLACEMENT_3D ( 'NONE', #32172, #24726, #32670 ) ;
#4537 = CARTESIAN_POINT ( 'NONE',  ( 195.0540265531851105, -1.025126265847089435, 162.5682875569279133 ) ) ;
#4538 = VECTOR ( 'NONE', #36400, 1000.000000000000000 ) ;
#4539 = ORIENTED_EDGE ( 'NONE', *, *, #3004, .F. ) ;
#4540 = CARTESIAN_POINT ( 'NONE',  ( 155.0540265531850537, -1.025126265847089435, -40.93171244307204404 ) ) ;
#4541 = DIRECTION ( 'NONE',  ( -0.000000000000000000, -0.000000000000000000, -1.000000000000000000 ) ) ;
#4542 = CARTESIAN_POINT ( 'NONE',  ( -567.5000000000000000, 57.49999999999996447, -183.5999999999997954 ) ) ;
#4543 = ORIENTED_EDGE ( 'NONE', *, *, #47512, .T. ) ;
#4544 = LINE ( 'NONE', #24549, #10987 ) ;
#4545 = ORIENTED_EDGE ( 'NONE', *, *, #25529, .T. ) ;
#4546 = ORIENTED_EDGE ( 'NONE', *, *, #21898, .T. ) ;
#4547 = AXIS2_PLACEMENT_3D ( 'NONE', #42677, #42422, #34242 ) ;
#4548 = CARTESIAN_POINT ( 'NONE',  ( 214.9999999999999432, 164.9999999999999716, 10.00000000000000000 ) ) ;
#4549 = CARTESIAN_POINT ( 'NONE',  ( -7.721099712662037540, 1.750000000000023981, 79.79316129108087807 ) ) ;
#4550 = ORIENTED_EDGE ( 'NONE', *, *, #41213, .F. ) ;
#4551 = FACE_OUTER_BOUND ( 'NONE', #27339, .T. ) ;
#4552 = CARTESIAN_POINT ( 'NONE',  ( 34.38425513258721367, -36.82177522737820397, 8.807470649214879543 ) ) ;
#4553 = EDGE_CURVE ( 'NONE', #9206, #40841, #39922, .T. ) ;
#4554 = EDGE_LOOP ( 'NONE', ( #46438, #2822, #42039 ) ) ;
#4555 = PLANE ( 'NONE',  #2993 ) ;
#4556 = ADVANCED_FACE ( 'NONE', ( #31459 ), #24270, .T. ) ;
#4557 = ORIENTED_EDGE ( 'NONE', *, *, #39805, .T. ) ;
#4558 = CYLINDRICAL_SURFACE ( 'NONE', #31592, 1.750000000000015543 ) ;
#4559 = CARTESIAN_POINT ( 'NONE',  ( -50.00000000000000000, 50.00000000000000000, 800.0000000000000000 ) ) ;
#4560 = FACE_OUTER_BOUND ( 'NONE', #4137, .T. ) ;
#4561 = ADVANCED_FACE ( 'NONE', ( #1175 ), #28601, .T. ) ;
#4562 = ORIENTED_EDGE ( 'NONE', *, *, #29967, .T. ) ;
#4563 = EDGE_CURVE ( 'NONE', #19653, #1180, #33919, .T. ) ;
#4564 = CARTESIAN_POINT ( 'NONE',  ( 24.47767542868285062, -23.18653802921781448, 8.807470649214879543 ) ) ;
#4565 = DIRECTION ( 'NONE',  ( 0.000000000000000000, -1.000000000000000000, -3.186989995019654210E-49 ) ) ;
#4566 = ORIENTED_EDGE ( 'NONE', *, *, #31121, .F. ) ;
#4567 = VECTOR ( 'NONE', #44736, 1000.000000000000000 ) ;
#4568 = ORIENTED_EDGE ( 'NONE', *, *, #49970, .T. ) ;
#4569 = ORIENTED_EDGE ( 'NONE', *, *, #20828, .T. ) ;
#4570 = DIRECTION ( 'NONE',  ( -1.445602896647339410E-16, -1.000000000000000000, -0.000000000000000000 ) ) ;
#4571 = EDGE_CURVE ( 'NONE', #27616, #3725, #12944, .T. ) ;
#4572 = ADVANCED_FACE ( 'NONE', ( #37780 ), #29303, .T. ) ;
#4573 = CIRCLE ( 'NONE', #479, 2.000000000000001776 ) ;
#4574 = CARTESIAN_POINT ( 'NONE',  ( 35.05402655318504657, 2.143131898507880377E-16, 119.0682875569279702 ) ) ;
#4575 = ORIENTED_EDGE ( 'NONE', *, *, #34002, .T. ) ;
#4576 = CARTESIAN_POINT ( 'NONE',  ( -45.67084718096785423, -1.750000000000009548, 121.8434138227750623 ) ) ;
#4577 = LINE ( 'NONE', #20224, #22970 ) ;
#4578 = CARTESIAN_POINT ( 'NONE',  ( -164.9999999999997442, 17.00000000000000000, -84.99999999999998579 ) ) ;
#4579 = VECTOR ( 'NONE', #19946, 1000.000000000000000 ) ;
#4580 = LINE ( 'NONE', #44545, #21892 ) ;
#4581 = CARTESIAN_POINT ( 'NONE',  ( 214.9999999999999432, -173.0000000000000000, 111.9999999999999858 ) ) ;
#4582 = CARTESIAN_POINT ( 'NONE',  ( 3.229232847726260403, -16.57333684275945629, 9.178419661560148768 ) ) ;
#4583 = VECTOR ( 'NONE', #38297, 1000.000000000000000 ) ;
#4584 = CARTESIAN_POINT ( 'NONE',  ( -84.94597344681493212, -1.025126265847089435, 39.06828755692797728 ) ) ;
#4585 = DIRECTION ( 'NONE',  ( -1.000000000000000000, 0.000000000000000000, 0.000000000000000000 ) ) ;
#4586 = CARTESIAN_POINT ( 'NONE',  ( -10.00000000000117062, 0.7319447344825763535, 9.406212099229145807 ) ) ;
#4587 = CARTESIAN_POINT ( 'NONE',  ( 32.57170742938662755, 18.58316106410423174, 7.697694107796188234 ) ) ;
#4588 = DIRECTION ( 'NONE',  ( -1.000000000000000000, 4.105366553918459587E-48, 1.586032880504786307E-16 ) ) ;
#4589 = AXIS2_PLACEMENT_3D ( 'NONE', #21174, #1686, #4521 ) ;
#4590 = AXIS2_PLACEMENT_3D ( 'NONE', #1653, #32698, #25004 ) ;
#4591 = CARTESIAN_POINT ( 'NONE',  ( -65.00000000000002842, 16.00000000000000000, -114.9999999999999858 ) ) ;
#4592 =( BOUNDED_CURVE ( )  B_SPLINE_CURVE ( 3, ( #3296, #44920, #11007, #7163 ),
 .UNSPECIFIED., .F., .F. ) 
 B_SPLINE_CURVE_WITH_KNOTS ( ( 4, 4 ),
 ( 1.570796326794896558, 3.141592653589793116 ),
 .UNSPECIFIED. ) 
 CURVE ( )  GEOMETRIC_REPRESENTATION_ITEM ( )  RATIONAL_B_SPLINE_CURVE ( ( 1.000000000000000000, 0.8047378541243649375, 0.8047378541243649375, 1.000000000000000000 ) ) 
 REPRESENTATION_ITEM ( '' )  );
#4593 = EDGE_CURVE ( 'NONE', #45598, #5571, #919, .T. ) ;
#4594 = PLANE ( 'NONE',  #28179 ) ;
#4595 = CARTESIAN_POINT ( 'NONE',  ( 151.5540265531850537, 0.000000000000000000, 119.0682875569279702 ) ) ;
#4596 = EDGE_LOOP ( 'NONE', ( #30129, #44161, #27134, #24118 ) ) ;
#4597 = DIRECTION ( 'NONE',  ( 0.000000000000000000, 0.000000000000000000, 1.000000000000000000 ) ) ;
#4598 =( BOUNDED_CURVE ( )  B_SPLINE_CURVE ( 3, ( #5970, #18013, #37310, #29077 ),
 .UNSPECIFIED., .F., .F. ) 
 B_SPLINE_CURVE_WITH_KNOTS ( ( 4, 4 ),
 ( 4.712388980384689674, 6.283185307179586232 ),
 .UNSPECIFIED. ) 
 CURVE ( )  GEOMETRIC_REPRESENTATION_ITEM ( )  RATIONAL_B_SPLINE_CURVE ( ( 1.000000000000000000, 0.8047378541243649375, 0.8047378541243649375, 1.000000000000000000 ) ) 
 REPRESENTATION_ITEM ( '' )  );
#4599 = CARTESIAN_POINT ( 'NONE',  ( -19.99999999999878142, 17.00000000000000000, 5.000000000000004441 ) ) ;
#4600 = CARTESIAN_POINT ( 'NONE',  ( 2.242409830259191494, -37.46921084408874947, 3.209567239418970708 ) ) ;
#4601 = CARTESIAN_POINT ( 'NONE',  ( -0.3862712429686977478, 1.188820645368937390, 10.00000000000000000 ) ) ;
#4602 = VERTEX_POINT ( 'NONE', #45421 ) ;
#4603 = VECTOR ( 'NONE', #23093, 1000.000000000000114 ) ;
#4604 = CARTESIAN_POINT ( 'NONE',  ( -64.99999999999815259, 17.00000000000000000, 65.00000000000000000 ) ) ;
#4605 = VECTOR ( 'NONE', #22848, 1000.000000000000000 ) ;
#4606 = DIRECTION ( 'NONE',  ( 0.7233555441435720601, -0.6904757466825006684, 0.000000000000000000 ) ) ;
#4607 = AXIS2_PLACEMENT_3D ( 'NONE', #14913, #45676, #34685 ) ;
#4608 = ORIENTED_EDGE ( 'NONE', *, *, #3877, .F. ) ;
#4609 = CARTESIAN_POINT ( 'NONE',  ( 48.99656738986517723, -11.00747004110342431, 1.847720168420772691 ) ) ;
#4611 = EDGE_CURVE ( 'NONE', #11124, #41652, #20908, .T. ) ;
#4610 = DIRECTION ( 'NONE',  ( 1.000000000000000000, 0.000000000000000000, 1.612977847700450206E-50 ) ) ;
#4612 = CARTESIAN_POINT ( 'NONE',  ( 135.0000000000006253, 17.00000000000000000, -30.00000000000000000 ) ) ;
#4613 =( BOUNDED_CURVE ( )  B_SPLINE_CURVE ( 3, ( #48134, #37168, #47888, #32552 ),
 .UNSPECIFIED., .F., .F. ) 
 B_SPLINE_CURVE_WITH_KNOTS ( ( 4, 4 ),
 ( 1.570796326794896558, 3.141592653589793116 ),
 .UNSPECIFIED. ) 
 CURVE ( )  GEOMETRIC_REPRESENTATION_ITEM ( )  RATIONAL_B_SPLINE_CURVE ( ( 1.000000000000000000, 0.8047378541243649375, 0.8047378541243649375, 1.000000000000000000 ) ) 
 REPRESENTATION_ITEM ( '' )  );
#4614 = ORIENTED_EDGE ( 'NONE', *, *, #23802, .F. ) ;
#4615 = FACE_OUTER_BOUND ( 'NONE', #17247, .T. ) ;
#4616 = EDGE_LOOP ( 'NONE', ( #23040, #33537, #3836, #29847, #40588, #31326 ) ) ;
#4617 = EDGE_LOOP ( 'NONE', ( #15516, #44597, #12349, #35678 ) ) ;
#4618 = CARTESIAN_POINT ( 'NONE',  ( -206.6959734468149463, 1.750000000000010658, 120.8182875569279702 ) ) ;
#4619 = EDGE_CURVE ( 'NONE', #35739, #48420, #23779, .T. ) ;
#4620 = ORIENTED_EDGE ( 'NONE', *, *, #5814, .T. ) ;
#4621 = DIRECTION ( 'NONE',  ( -4.996003610813203446E-16, -1.000000000000000000, 0.000000000000000000 ) ) ;
#4622 = FACE_OUTER_BOUND ( 'NONE', #43088, .T. ) ;
#4623 = FACE_OUTER_BOUND ( 'NONE', #36457, .T. ) ;
#4624 = CARTESIAN_POINT ( 'NONE',  ( 168.9999999999999147, -272.5000000000000000, -96.99999999999988631 ) ) ;
#4625 = ORIENTED_EDGE ( 'NONE', *, *, #39462, .T. ) ;
#4626 = AXIS2_PLACEMENT_3D ( 'NONE', #26012, #29596, #18790 ) ;
#4627 = CARTESIAN_POINT ( 'NONE',  ( -84.94597344681494633, 2.143131898507880377E-16, -117.4317124430720725 ) ) ;
#4628 = EDGE_CURVE ( 'NONE', #6245, #49119, #32621, .T. ) ;
#4629 = VERTEX_POINT ( 'NONE', #44485 ) ;
#4630 = EDGE_CURVE ( 'NONE', #45663, #44427, #43389, .T. ) ;
#4631 = CARTESIAN_POINT ( 'NONE',  ( -1.250000000000000222, 0.000000000000000000, 3.333333333333333481 ) ) ;
#4632 = CARTESIAN_POINT ( 'NONE',  ( -239.0000000000000853, -153.6999999999999602, 254.8599999999999852 ) ) ;
#4633 = ORIENTED_EDGE ( 'NONE', *, *, #7158, .T. ) ;
#4634 = LINE ( 'NONE', #16672, #3256 ) ;
#4635 = EDGE_CURVE ( 'NONE', #23429, #35155, #31705, .T. ) ;
#4636 = CARTESIAN_POINT ( 'NONE',  ( 344.0000000000000568, 165.0000000000000000, 339.9999999999998295 ) ) ;
#4637 = VERTEX_POINT ( 'NONE', #6213 ) ;
#4638 = CARTESIAN_POINT ( 'NONE',  ( -45.67084718096785423, 1.750000000000010214, 79.79316129108087807 ) ) ;
#4639 = EDGE_CURVE ( 'NONE', #46409, #16952, #10550, .T. ) ;
#4640 = CARTESIAN_POINT ( 'NONE',  ( 71.55402655318505367, 1.025126265847089213, 159.0682875569279418 ) ) ;
#4641 = CARTESIAN_POINT ( 'NONE',  ( 169.0000000000000000, 2.775557561562891351E-14, -115.0000000000001563 ) ) ;
#4642 = EDGE_CURVE ( 'NONE', #13147, #6226, #49255, .T. ) ;
#4643 = FACE_OUTER_BOUND ( 'NONE', #22886, .T. ) ;
#4644 = VECTOR ( 'NONE', #42594, 1000.000000000000000 ) ;
#4645 = VERTEX_POINT ( 'NONE', #5000 ) ;
#4646 = CARTESIAN_POINT ( 'NONE',  ( -45.67084718096785423, 1.750000000000010214, 119.7931612910808781 ) ) ;
#4647 = VECTOR ( 'NONE', #1923, 1000.000000000000000 ) ;
#4648 = CARTESIAN_POINT ( 'NONE',  ( -0.3862712429686977478, 1.188820645368937390, 10.00000000000000000 ) ) ;
#4649 = ADVANCED_FACE ( 'NONE', ( #20653 ), #38293, .F. ) ;
#4650 = DIRECTION ( 'NONE',  ( 0.000000000000000000, 0.000000000000000000, 1.000000000000000000 ) ) ;
#4651 = ORIENTED_EDGE ( 'NONE', *, *, #28220, .F. ) ;
#4652 = ORIENTED_EDGE ( 'NONE', *, *, #34626, .F. ) ;
#4653 = APPLICATION_PROTOCOL_DEFINITION ( 'draft international standard', 'automotive_design', 1998, #4994 ) ;
#4654 = CARTESIAN_POINT ( 'NONE',  ( 181.0000000000000000, -93.49999999999998579, -350.0000000000001705 ) ) ;
#4655 = DIRECTION ( 'NONE',  ( -0.000000000000000000, -1.000000000000000000, -0.000000000000000000 ) ) ;
#4656 = CARTESIAN_POINT ( 'NONE',  ( -1.011271242968683426, -0.7347315653655928092, 10.00000000000000000 ) ) ;
#4657 = CARTESIAN_POINT ( 'NONE',  ( -19.99999999999846523, 16.00000000000000000, 35.00000000000000000 ) ) ;
#4658 = CARTESIAN_POINT ( 'NONE',  ( 210.0000000000000568, 0.000000000000000000, -119.1817124430720440 ) ) ;
#4659 = ORIENTED_EDGE ( 'NONE', *, *, #4896, .F. ) ;
#4660 = DIRECTION ( 'NONE',  ( 1.000000000000000000, 0.000000000000000000, -2.312964634635864737E-16 ) ) ;
#4661 = CARTESIAN_POINT ( 'NONE',  ( 196.8526953830863135, -154.8119894309599260, 472.8425600500171981 ) ) ;
#4662 = CARTESIAN_POINT ( 'NONE',  ( -2.210477865340801706, -37.43479381012853224, -9.422646554964178023 ) ) ;
#4663 = DIRECTION ( 'NONE',  ( 0.000000000000000000, 0.000000000000000000, -1.000000000000000000 ) ) ;
#4664 = VECTOR ( 'NONE', #27657, 1000.000000000000000 ) ;
#4665 = ORIENTED_EDGE ( 'NONE', *, *, #2071, .F. ) ;
#4666 = DIRECTION ( 'NONE',  ( -0.000000000000000000, -0.000000000000000000, -1.000000000000000000 ) ) ;
#4667 = EDGE_LOOP ( 'NONE', ( #3743, #25148, #44337, #20755 ) ) ;
#4668 = CARTESIAN_POINT ( 'NONE',  ( -164.9999999999994031, 17.00000000000000000, -54.99999999999999289 ) ) ;
#4669 = ORIENTED_EDGE ( 'NONE', *, *, #3120, .T. ) ;
#4670 = CARTESIAN_POINT ( 'NONE',  ( -13.92102703536724384, -30.85732372859812500, 8.356839323120299312 ) ) ;
#4671 = CARTESIAN_POINT ( 'NONE',  ( -225.0000000000000568, -175.0000000000000000, 474.0000000000000000 ) ) ;
#4672 = LINE ( 'NONE', #44397, #46955 ) ;
#4673 = DIRECTION ( 'NONE',  ( 0.000000000000000000, -1.000000000000000000, 0.000000000000000000 ) ) ;
#4674 = EDGE_LOOP ( 'NONE', ( #39071, #15651, #40427, #12695 ) ) ;
#4675 = EDGE_CURVE ( 'NONE', #30474, #19896, #34182, .T. ) ;
#4676 = DIRECTION ( 'NONE',  ( 0.000000000000000000, -0.3846153846153845812, -0.9230769230769231282 ) ) ;
#4677 = AXIS2_PLACEMENT_3D ( 'NONE', #39477, #43554, #27409 ) ;
#4678 = CARTESIAN_POINT ( 'NONE',  ( 210.0000000000000568, 0.000000000000000000, 162.5682875569279702 ) ) ;
#4679 = ORIENTED_EDGE ( 'NONE', *, *, #44953, .F. ) ;
#4680 = FACE_OUTER_BOUND ( 'NONE', #45680, .T. ) ;
#4681 = FACE_OUTER_BOUND ( 'NONE', #374, .T. ) ;
#4682 = CARTESIAN_POINT ( 'NONE',  ( 0.3862712429686727678, 1.188820645368945605, 10.00000000000000000 ) ) ;
#4683 = FACE_OUTER_BOUND ( 'NONE', #36084, .T. ) ;
#4684 = EDGE_LOOP ( 'NONE', ( #47062, #20099, #110, #37219 ) ) ;
#4685 = ORIENTED_EDGE ( 'NONE', *, *, #23613, .F. ) ;
#4686 = DIRECTION ( 'NONE',  ( 0.000000000000000000, 1.000000000000000000, -7.004339610132985974E-48 ) ) ;
#4687 = EDGE_CURVE ( 'NONE', #35926, #43437, #34948, .T. ) ;
#4688 = EDGE_LOOP ( 'NONE', ( #31087, #510, #30808, #41552, #18648 ) ) ;
#4689 = ADVANCED_FACE ( 'NONE', ( #50517 ), #35196, .F. ) ;
#4690 = LINE ( 'NONE', #20581, #6917 ) ;
#4691 = DIRECTION ( 'NONE',  ( 0.000000000000000000, 0.000000000000000000, 1.000000000000000000 ) ) ;
#4692 = FACE_OUTER_BOUND ( 'NONE', #35270, .T. ) ;
#4693 =( BOUNDED_CURVE ( )  B_SPLINE_CURVE ( 3, ( #49650, #49400, #34067, #14541 ),
 .UNSPECIFIED., .F., .F. ) 
 B_SPLINE_CURVE_WITH_KNOTS ( ( 4, 4 ),
 ( 0.000000000000000000, 1.570796326794896558 ),
 .UNSPECIFIED. ) 
 CURVE ( )  GEOMETRIC_REPRESENTATION_ITEM ( )  RATIONAL_B_SPLINE_CURVE ( ( 1.000000000000000000, 0.8047378541243649375, 0.8047378541243649375, 1.000000000000000000 ) ) 
 REPRESENTATION_ITEM ( '' )  );
#4694 = ORIENTED_EDGE ( 'NONE', *, *, #24357, .F. ) ;
#4695 = CARTESIAN_POINT ( 'NONE',  ( 166.9999999999999716, -180.9999999999999716, -340.0000000000001137 ) ) ;
#4696 = FACE_OUTER_BOUND ( 'NONE', #34839, .T. ) ;
#4697 = ADVANCED_FACE ( 'NONE', ( #6705 ), #30572, .F. ) ;
#4698 = EDGE_CURVE ( 'NONE', #22032, #7355, #20172, .T. ) ;
#4699 = CARTESIAN_POINT ( 'NONE',  ( 2.538055338523177440, 33.28424297489108596, -9.367992836599954742 ) ) ;
#4700 = ORIENTED_EDGE ( 'NONE', *, *, #14862, .T. ) ;
#4701 = ORIENTED_EDGE ( 'NONE', *, *, #19984, .T. ) ;
#4702 = ORIENTED_EDGE ( 'NONE', *, *, #12383, .F. ) ;
#4703 = DIRECTION ( 'NONE',  ( -1.586032880504786307E-16, 1.654361225106055350E-24, -1.000000000000000000 ) ) ;
#4704 = EDGE_CURVE ( 'NONE', #36023, #25767, #19001, .T. ) ;
#4705 = SURFACE_STYLE_USAGE ( .BOTH. , #47002 ) ;
#4706 = CARTESIAN_POINT ( 'NONE',  ( -8.445973446814976526, 0.000000000000000000, 82.56828755692801280 ) ) ;
#4707 = ORIENTED_EDGE ( 'NONE', *, *, #3110, .F. ) ;
#4708 = CARTESIAN_POINT ( 'NONE',  ( 191.5540265531851105, 0.000000000000000000, -0.9317124430720247208 ) ) ;
#4709 = VERTEX_POINT ( 'NONE', #50009 ) ;
#4710 = LINE ( 'NONE', #47262, #25030 ) ;
#4711 = ORIENTED_EDGE ( 'NONE', *, *, #40067, .F. ) ;
#4712 =( LENGTH_UNIT ( ) NAMED_UNIT ( * ) SI_UNIT ( .MILLI., .METRE. ) );
#4713 = CARTESIAN_POINT ( 'NONE',  ( 0.9494396179258391966, -9.954826186926261755, 9.646707543097345905 ) ) ;
#4714 = CARTESIAN_POINT ( 'NONE',  ( -8.445973446814976526, 0.000000000000000000, -117.4317124430720156 ) ) ;
#4715 = DIRECTION ( 'NONE',  ( -0.000000000000000000, -0.000000000000000000, -1.000000000000000000 ) ) ;
#4716 = AXIS2_PLACEMENT_3D ( 'NONE', #19387, #50389, #27611 ) ;
#4717 = CARTESIAN_POINT ( 'NONE',  ( -114.9999999999991047, 16.00000000000000000, -24.99999999999999289 ) ) ;
#4718 = DIRECTION ( 'NONE',  ( 1.000000000000000000, 6.938893903907233308E-16, 0.000000000000000000 ) ) ;
#4719 = CARTESIAN_POINT ( 'NONE',  ( 341.9999999999999432, 169.0000000000001990, -344.0000000000002842 ) ) ;
#4720 = ORIENTED_EDGE ( 'NONE', *, *, #6786, .T. ) ;
#4721 = EDGE_LOOP ( 'NONE', ( #30390, #101, #27010, #3516 ) ) ;
#4722 = DIRECTION ( 'NONE',  ( 1.000000000000000000, 0.000000000000000000, 0.000000000000000000 ) ) ;
#4723 = LINE ( 'NONE', #28068, #49597 ) ;
#4724 = DIRECTION ( 'NONE',  ( 0.000000000000000000, 0.000000000000000000, 1.000000000000000000 ) ) ;
#4725 = ORIENTED_EDGE ( 'NONE', *, *, #23850, .F. ) ;
#4726 = CARTESIAN_POINT ( 'NONE',  ( -37.27397286063865778, 4.111076158911805223, 7.697694107796192675 ) ) ;
#4727 = CARTESIAN_POINT ( 'NONE',  ( -208.4459734468149463, 0.000000000000000000, -117.4317124430720725 ) ) ;
#4728 = EDGE_CURVE ( 'NONE', #38804, #36506, #3355, .T. ) ;
#4729 = ORIENTED_EDGE ( 'NONE', *, *, #33672, .F. ) ;
#4730 = LINE ( 'NONE', #31435, #48310 ) ;
#4731 = LINE ( 'NONE', #3780, #32041 ) ;
#4732 = DIRECTION ( 'NONE',  ( 0.000000000000000000, 0.000000000000000000, -1.000000000000000000 ) ) ;
#4733 = LINE ( 'NONE', #20375, #38965 ) ;
#4734 = VERTEX_POINT ( 'NONE', #39 ) ;
#4735 = VERTEX_POINT ( 'NONE', #22856 ) ;
#4736 = CARTESIAN_POINT ( 'NONE',  ( 80.00000000000028422, 17.00000000000000000, -84.99999999999998579 ) ) ;
#4737 = CARTESIAN_POINT ( 'NONE',  ( 7.749480817862238524, 14.85497772329518895, 9.403735324607438884 ) ) ;
#4738 =( BOUNDED_CURVE ( )  B_SPLINE_CURVE ( 3, ( #19204, #23319, #43070, #6915 ),
 .UNSPECIFIED., .F., .F. ) 
 B_SPLINE_CURVE_WITH_KNOTS ( ( 4, 4 ),
 ( 3.141592653589793116, 4.712388980384689674 ),
 .UNSPECIFIED. ) 
 CURVE ( )  GEOMETRIC_REPRESENTATION_ITEM ( )  RATIONAL_B_SPLINE_CURVE ( ( 1.000000000000000000, 0.8047378541243649375, 0.8047378541243649375, 1.000000000000000000 ) ) 
 REPRESENTATION_ITEM ( '' )  );
#4739 = AXIS2_PLACEMENT_3D ( 'NONE', #47067, #15047, #11972 ) ;
#4740 = ORIENTED_EDGE ( 'NONE', *, *, #15770, .F. ) ;
#4741 = VERTEX_POINT ( 'NONE', #18502 ) ;
#4742 = LINE ( 'NONE', #47550, #10008 ) ;
#4743 = CARTESIAN_POINT ( 'NONE',  ( 7.608425291889091113, -36.72004717559254772, 7.697694107796188234 ) ) ;
#4744 = CARTESIAN_POINT ( 'NONE',  ( 192.2789002873380184, -1.750000000000010214, -78.15658617722490931 ) ) ;
#4745 = CYLINDRICAL_SURFACE ( 'NONE', #3450, 1.750000000000001554 ) ;
#4746 = ORIENTED_EDGE ( 'NONE', *, *, #46903, .T. ) ;
#4747 = ORIENTED_EDGE ( 'NONE', *, *, #2101, .F. ) ;
#4748 = VERTEX_POINT ( 'NONE', #42359 ) ;
#4749 =( BOUNDED_CURVE ( )  B_SPLINE_CURVE ( 3, ( #9787, #33173, #25707, #48753 ),
 .UNSPECIFIED., .F., .F. ) 
 B_SPLINE_CURVE_WITH_KNOTS ( ( 4, 4 ),
 ( 4.712388980384689674, 6.283185307179586232 ),
 .UNSPECIFIED. ) 
 CURVE ( )  GEOMETRIC_REPRESENTATION_ITEM ( )  RATIONAL_B_SPLINE_CURVE ( ( 1.000000000000000000, 0.8047378541243649375, 0.8047378541243649375, 1.000000000000000000 ) ) 
 REPRESENTATION_ITEM ( '' )  );
#4750 = PLANE ( 'NONE',  #34099 ) ;
#4751 = CARTESIAN_POINT ( 'NONE',  ( -18.69789054174323084, 27.49790346457746182, -2.408242355805840784 ) ) ;
#4752 = EDGE_LOOP ( 'NONE', ( #20974, #12743, #21409, #26520 ) ) ;
#4753 = ORIENTED_EDGE ( 'NONE', *, *, #43004, .T. ) ;
#4754 = CARTESIAN_POINT ( 'NONE',  ( 0.9870575514054733546, 1.980598328282569653, 9.881002359080278907 ) ) ;
#4755 = ADVANCED_FACE ( 'NONE', ( #42858 ), #3870, .F. ) ;
#4756 = DIRECTION ( 'NONE',  ( 0.000000000000000000, 0.000000000000000000, 1.000000000000000000 ) ) ;
#4757 = CARTESIAN_POINT ( 'NONE',  ( -239.0000000000000853, -165.6999999999999602, 250.3600000000000136 ) ) ;
#4758 = ORIENTED_EDGE ( 'NONE', *, *, #4027, .T. ) ;
#4759 = ORIENTED_EDGE ( 'NONE', *, *, #41700, .T. ) ;
#4760 = PLANE ( 'NONE',  #16783 ) ;
#4761 = CARTESIAN_POINT ( 'NONE',  ( -124.9459734468149321, 1.025126265847081886, 79.06828755692797017 ) ) ;
#4762 = VERTEX_POINT ( 'NONE', #34431 ) ;
#4763 = DIRECTION ( 'NONE',  ( -1.000000000000000000, 0.000000000000000000, 0.000000000000000000 ) ) ;
#4764 = CARTESIAN_POINT ( 'NONE',  ( -84.94597344681493212, -1.025126265847089213, -160.9317124430720014 ) ) ;
#4765 = DIRECTION ( 'NONE',  ( -1.000000000000000000, 0.000000000000000000, 0.000000000000000000 ) ) ;
#4766 = ORIENTED_EDGE ( 'NONE', *, *, #46361, .T. ) ;
#4767 = DIRECTION ( 'NONE',  ( 0.000000000000000000, 0.2981428420003837121, 0.9545212652235329776 ) ) ;
#4768 = LINE ( 'NONE', #15816, #17470 ) ;
#4769 = CARTESIAN_POINT ( 'NONE',  ( 1.011271242968683648, 0.7347315653655930312, -10.00000000000000000 ) ) ;
#4770 = CARTESIAN_POINT ( 'NONE',  ( -0.6721397084974984892, -9.977385840602783773, 0.000000000000000000 ) ) ;
#4771 = VECTOR ( 'NONE', #14422, 1000.000000000000000 ) ;
#4772 = DIRECTION ( 'NONE',  ( -0.000000000000000000, 1.000000000000000000, 0.000000000000000000 ) ) ;
#4773 = LINE ( 'NONE', #12731, #46270 ) ;
#4774 = CARTESIAN_POINT ( 'NONE',  ( 343.9999999999993747, -183.0000000000000000, 357.9999999999998295 ) ) ;
#4775 = ORIENTED_EDGE ( 'NONE', *, *, #30409, .T. ) ;
#4776 = FILL_AREA_STYLE ('',( #27641 ) ) ;
#4777 = CARTESIAN_POINT ( 'NONE',  ( 155.0540265531850537, 2.143131898507880377E-16, 42.56828755692798438 ) ) ;
#4778 = VERTEX_POINT ( 'NONE', #15671 ) ;
#4779 = CARTESIAN_POINT ( 'NONE',  ( 9.999999999999962697, 8.486842105263161073, 18.38522261288946780 ) ) ;
#4780 = CARTESIAN_POINT ( 'NONE',  ( 1.011271242968677653, 0.7347315653656002477, 10.00000000000000000 ) ) ;
#4781 = ORIENTED_EDGE ( 'NONE', *, *, #20610, .T. ) ;
#4782 = DIRECTION ( 'NONE',  ( -3.172065784643302499E-16, -1.000000000000000000, 2.537652627714642000E-15 ) ) ;
#4783 = B_SPLINE_SURFACE_WITH_KNOTS ( 'NONE', 3, 3, ( 
 ( #39406, #35554, #4737, #8347 ),
 ( #395, #20890, #36060, #12186 ),
 ( #31954, #40405, #16042, #43475 ),
 ( #39908, #44223, #5241, #23990 ) ),
 .UNSPECIFIED., .F., .F., .F.,
 ( 4, 4 ),
 ( 4, 4 ),
 ( 0.000000000000000000, 1.000000000000000000 ),
 ( 0.000000000000000000, 1.000000000000000000 ),
 .UNSPECIFIED. ) ;
#4784 = VERTEX_POINT ( 'NONE', #14915 ) ;
#4785 = ORIENTED_EDGE ( 'NONE', *, *, #43874, .T. ) ;
#4786 = CARTESIAN_POINT ( 'NONE',  ( 45.64490844644691236, 21.32281559348795952, 8.807470649214879543 ) ) ;
#4787 = ORIENTED_EDGE ( 'NONE', *, *, #20326, .F. ) ;
#4788 = CARTESIAN_POINT ( 'NONE',  ( 1.917969350850768029, -0.3547183498316657801, 9.896382706792435258 ) ) ;
#4789 = CARTESIAN_POINT ( 'NONE',  ( 0.000000000000000000, -165.1999999999999602, 359.7999999999997840 ) ) ;
#4790 = VERTEX_POINT ( 'NONE', #31079 ) ;
#4791 = FACE_OUTER_BOUND ( 'NONE', #13855, .T. ) ;
#4792 = ORIENTED_EDGE ( 'NONE', *, *, #4127, .F. ) ;
#4793 = DIRECTION ( 'NONE',  ( -0.000000000000000000, -1.000000000000000000, -0.000000000000000000 ) ) ;
#4794 = LINE ( 'NONE', #469, #21733 ) ;
#4795 = CARTESIAN_POINT ( 'NONE',  ( -31.44259251615275019, -38.95901822126145220, -9.367992836599954742 ) ) ;
#4796 = EDGE_LOOP ( 'NONE', ( #46929, #32323, #13463, #23269, #24151, #2295, #23463, #49917, #30279, #15234, #47814, #24622, #25644, #5470, #684, #2532, #10930 ) ) ;
#4797 = CIRCLE ( 'NONE', #38417, 1.750000000000015543 ) ;
#4798 = ADVANCED_FACE ( 'NONE', ( #26460 ), #26966, .F. ) ;
#4799 = CARTESIAN_POINT ( 'NONE',  ( -1.011271242968677875, -0.7347315653656004697, 10.00000000000000000 ) ) ;
#4800 = CARTESIAN_POINT ( 'NONE',  ( 75.05402655318509630, 2.143131898507880377E-16, 122.5682875569279844 ) ) ;
#4801 = ORIENTED_EDGE ( 'NONE', *, *, #37775, .F. ) ;
#4802 = VERTEX_POINT ( 'NONE', #42603 ) ;
#4803 = VERTEX_POINT ( 'NONE', #7484 ) ;
#4804 = CARTESIAN_POINT ( 'NONE',  ( -86.69597344681494633, 1.750000000000010658, 80.81828755692798438 ) ) ;
#4805 = EDGE_CURVE ( 'NONE', #46904, #16166, #23114, .T. ) ;
#4806 = CARTESIAN_POINT ( 'NONE',  ( 224.9999999999999716, -175.0000000000000000, 474.9999999999998863 ) ) ;
#4807 = ORIENTED_EDGE ( 'NONE', *, *, #8704, .T. ) ;
#4808 = EDGE_CURVE ( 'NONE', #11842, #39424, #45925, .T. ) ;
#4809 = DIRECTION ( 'NONE',  ( 1.000000000000000000, 0.000000000000000000, 0.000000000000000000 ) ) ;
#4810 = DIRECTION ( 'NONE',  ( 0.000000000000000000, 1.000000000000000000, 0.000000000000000000 ) ) ;
#4811 = ADVANCED_FACE ( 'NONE', ( #11578 ), #42097, .T. ) ;
#4812 = CARTESIAN_POINT ( 'NONE',  ( -124.9459734468149463, 2.143131898507847836E-16, 82.56828755692797017 ) ) ;
#4813 = CARTESIAN_POINT ( 'NONE',  ( 34.32915281903212446, 1.750000000000009548, -160.2068387089191219 ) ) ;
#4814 = CARTESIAN_POINT ( 'NONE',  ( 0.09523839817332763191, 1.466467394239034050, 9.958264684458713489 ) ) ;
#4815 = DIRECTION ( 'NONE',  ( -0.000000000000000000, -0.000000000000000000, -1.000000000000000000 ) ) ;
#4816 = LINE ( 'NONE', #48135, #43873 ) ;
#4817 = CARTESIAN_POINT ( 'NONE',  ( 33.30402655318503946, -1.750000000000010658, 80.81828755692798438 ) ) ;
#4818 = CARTESIAN_POINT ( 'NONE',  ( -194.9999999999999432, -173.0000000000000000, 132.0000000000000853 ) ) ;
#4819 = DIRECTION ( 'NONE',  ( -0.7233555441435720601, 0.6904757466825006684, 0.000000000000000000 ) ) ;
#4820 = LINE ( 'NONE', #35667, #18329 ) ;
#4821 = ORIENTED_EDGE ( 'NONE', *, *, #32289, .T. ) ;
#4822 = DIRECTION ( 'NONE',  ( -1.000000000000000000, -0.000000000000000000, -0.000000000000000000 ) ) ;
#4823 = CARTESIAN_POINT ( 'NONE',  ( 0.1287570809895630941, -0.3962735484563133515, 10.00000000000000000 ) ) ;
#4824 = DIRECTION ( 'NONE',  ( 0.000000000000000000, -1.000000000000000000, -0.000000000000000000 ) ) ;
#4825 = EDGE_CURVE ( 'NONE', #15344, #37516, #44243, .T. ) ;
#4826 = EDGE_CURVE ( 'NONE', #13377, #46801, #19773, .T. ) ;
#4827 = CARTESIAN_POINT ( 'NONE',  ( -9.998889670239194061, -0.1490146381531308739, 9.282506307616474217 ) ) ;
#4828 = AXIS2_PLACEMENT_3D ( 'NONE', #3770, #19420, #15572 ) ;
#4830 = EDGE_LOOP ( 'NONE', ( #10, #3738, #28768, #18671 ) ) ;
#4829 = EDGE_CURVE ( 'NONE', #25755, #24963, #8991, .T. ) ;
#4831 = LINE ( 'NONE', #47394, #28905 ) ;
#4832 = EDGE_CURVE ( 'NONE', #357, #47536, #47438, .T. ) ;
#4833 = VECTOR ( 'NONE', #35972, 1000.000000000000000 ) ;
#4834 = DIRECTION ( 'NONE',  ( 1.000000000000000000, 0.000000000000000000, 0.000000000000000000 ) ) ;
#4835 = VECTOR ( 'NONE', #39057, 1000.000000000000000 ) ;
#4836 = ORIENTED_EDGE ( 'NONE', *, *, #41224, .T. ) ;
#4837 = EDGE_CURVE ( 'NONE', #30887, #12850, #27733, .T. ) ;
#4838 = CARTESIAN_POINT ( 'NONE',  ( -1.011271242968688533, 0.7347315653655859258, -10.00000000000000000 ) ) ;
#4839 = LINE ( 'NONE', #13296, #28132 ) ;
#4840 = VECTOR ( 'NONE', #10206, 1000.000000000000000 ) ;
#4841 = CYLINDRICAL_SURFACE ( 'NONE', #35859, 2.000000000000001776 ) ;
#4842 = EDGE_CURVE ( 'NONE', #25256, #46047, #1042, .T. ) ;
#4843 = ORIENTED_EDGE ( 'NONE', *, *, #7323, .T. ) ;
#4844 = CARTESIAN_POINT ( 'NONE',  ( 165.0000000000000000, -174.9999999999999716, -115.0000000000001563 ) ) ;
#4845 = VERTEX_POINT ( 'NONE', #15935 ) ;
#4846 = ORIENTED_EDGE ( 'NONE', *, *, #45236, .F. ) ;
#4847 = VECTOR ( 'NONE', #50043, 1000.000000000000000 ) ;
#4848 = ORIENTED_EDGE ( 'NONE', *, *, #17713, .F. ) ;
#4849 = DIRECTION ( 'NONE',  ( 1.000000000000000000, 0.000000000000000000, 0.000000000000000000 ) ) ;
#4850 = CARTESIAN_POINT ( 'NONE',  ( 181.0000000000000000, -256.5000000000000000, -114.9999999999999574 ) ) ;
#4851 = VERTEX_POINT ( 'NONE', #39288 ) ;
#4852 = CARTESIAN_POINT ( 'NONE',  ( -114.9999999999997158, 17.00000000000000000, -84.99999999999998579 ) ) ;
#4853 = CARTESIAN_POINT ( 'NONE',  ( 55.00000000000002132, 52.49999999999999289, -5.000000000000000000 ) ) ;
#4854 = PLANE ( 'NONE',  #31475 ) ;
#4855 = CARTESIAN_POINT ( 'NONE',  ( 111.5540265531850679, 0.000000000000000000, -37.43171244307205825 ) ) ;
#4856 = EDGE_CURVE ( 'NONE', #39319, #34689, #36203, .T. ) ;
#4857 = ORIENTED_EDGE ( 'NONE', *, *, #10866, .F. ) ;
#4858 = FACE_OUTER_BOUND ( 'NONE', #14635, .T. ) ;
#4859 = ADVANCED_FACE ( 'NONE', ( #24149 ), #16437, .F. ) ;
#4860 = ORIENTED_EDGE ( 'NONE', *, *, #44400, .T. ) ;
#4861 = ADVANCED_FACE ( 'NONE', ( #16949 ), #28492, .F. ) ;
#4862 = FACE_OUTER_BOUND ( 'NONE', #30834, .T. ) ;
#4863 = ORIENTED_EDGE ( 'NONE', *, *, #49340, .F. ) ;
#4864 = CARTESIAN_POINT ( 'NONE',  ( 210.0000000000000568, 0.000000000000000000, -77.43171244307200141 ) ) ;
#4865 = DIRECTION ( 'NONE',  ( 1.000000000000000000, 0.000000000000000000, 0.000000000000000000 ) ) ;
#4866 = B_SPLINE_CURVE_WITH_KNOTS ( 'NONE', 3,
 ( #18993, #31071, #39033, #22604, #15162, #22849 ),
 .UNSPECIFIED., .F., .F.,
 ( 4, 2, 4 ),
 ( 4.982613841084487634E-17, 0.009882509389272372408, 0.01976501877854469277 ),
 .UNSPECIFIED. ) ;
#4867 = VERTEX_POINT ( 'NONE', #43124 ) ;
#4868 = DIRECTION ( 'NONE',  ( -0.000000000000000000, -0.000000000000000000, -1.000000000000000000 ) ) ;
#4869 = AXIS2_PLACEMENT_3D ( 'NONE', #10277, #33888, #49481 ) ;
#4870 = LINE ( 'NONE', #28242, #50272 ) ;
#4871 = DIRECTION ( 'NONE',  ( 0.000000000000000000, 0.000000000000000000, -1.000000000000000000 ) ) ;
#4872 =( BOUNDED_CURVE ( )  B_SPLINE_CURVE ( 3, ( #602, #4185, #43667, #90 ),
 .UNSPECIFIED., .F., .F. ) 
 B_SPLINE_CURVE_WITH_KNOTS ( ( 4, 4 ),
 ( 0.000000000000000000, 1.570796326794896558 ),
 .UNSPECIFIED. ) 
 CURVE ( )  GEOMETRIC_REPRESENTATION_ITEM ( )  RATIONAL_B_SPLINE_CURVE ( ( 1.000000000000000000, 0.8047378541243649375, 0.8047378541243649375, 1.000000000000000000 ) ) 
 REPRESENTATION_ITEM ( '' )  );
#4873 = DIRECTION ( 'NONE',  ( 1.000000000000000000, 0.000000000000000000, 0.000000000000000000 ) ) ;
#4874 = VERTEX_POINT ( 'NONE', #43619 ) ;
#4875 = DIRECTION ( 'NONE',  ( 1.000000000000000000, 0.000000000000000000, 0.000000000000000000 ) ) ;
#4876 = CARTESIAN_POINT ( 'NONE',  ( 79.99999999999997158, 17.00000000000000000, -114.9999999999999858 ) ) ;
#4877 = EDGE_CURVE ( 'NONE', #47806, #36821, #293, .T. ) ;
#4878 = AXIS2_PLACEMENT_3D ( 'NONE', #40789, #12566, #28740 ) ;
#4879 =( BOUNDED_CURVE ( )  B_SPLINE_CURVE ( 3, ( #15037, #18616, #27613, #3740 ),
 .UNSPECIFIED., .F., .F. ) 
 B_SPLINE_CURVE_WITH_KNOTS ( ( 4, 4 ),
 ( 5.723266580096324496, 6.283185307179586232 ),
 .UNSPECIFIED. ) 
 CURVE ( )  GEOMETRIC_REPRESENTATION_ITEM ( )  RATIONAL_B_SPLINE_CURVE ( ( 1.000000000000000000, 0.9740444450880465510, 0.9740444450880465510, 1.000000000000000000 ) ) 
 REPRESENTATION_ITEM ( '' )  );
#4880 = DIRECTION ( 'NONE',  ( -1.000000000000000000, 0.000000000000000000, 0.000000000000000000 ) ) ;
#4881 = ORIENTED_EDGE ( 'NONE', *, *, #49715, .T. ) ;
#4882 = ORIENTED_EDGE ( 'NONE', *, *, #33394, .F. ) ;
#4883 = APPLICATION_PROTOCOL_DEFINITION ( 'draft international standard', 'automotive_design', 1998, #29271 ) ;
#4885 = CARTESIAN_POINT ( 'NONE',  ( 360.0000000000000000, 165.0000000000000000, -106.0000000000001990 ) ) ;
#4884 = VECTOR ( 'NONE', #27836, 1000.000000000000000 ) ;
#4886 = CARTESIAN_POINT ( 'NONE',  ( 168.9999999999999147, -182.9999999999999716, -340.0000000000001137 ) ) ;
#4887 = EDGE_CURVE ( 'NONE', #9722, #32176, #8748, .T. ) ;
#4888 = CARTESIAN_POINT ( 'NONE',  ( -177.4999999999999716, 57.49999999999996447, -130.5992382549688671 ) ) ;
#4889 = DIRECTION ( 'NONE',  ( 1.000000000000000000, 0.000000000000000000, 0.000000000000000000 ) ) ;
#4890 = VERTEX_POINT ( 'NONE', #8239 ) ;
#4891 = CARTESIAN_POINT ( 'NONE',  ( 183.0000000000000000, 6.000000000000060396, -340.0000000000001137 ) ) ;
#4892 =( BOUNDED_CURVE ( )  B_SPLINE_CURVE ( 3, ( #12322, #1040, #4638, #20281 ),
 .UNSPECIFIED., .F., .F. ) 
 B_SPLINE_CURVE_WITH_KNOTS ( ( 4, 4 ),
 ( 0.000000000000000000, 1.570796326794896558 ),
 .UNSPECIFIED. ) 
 CURVE ( )  GEOMETRIC_REPRESENTATION_ITEM ( )  RATIONAL_B_SPLINE_CURVE ( ( 1.000000000000000000, 0.8047378541243649375, 0.8047378541243649375, 1.000000000000000000 ) ) 
 REPRESENTATION_ITEM ( '' )  );
#4893 = CARTESIAN_POINT ( 'NONE',  ( -204.9459734468148895, -1.025126265847088991, 162.5682875569279133 ) ) ;
#4894 = DIRECTION ( 'NONE',  ( 0.000000000000000000, 0.000000000000000000, -1.000000000000000000 ) ) ;
#4895 = CARTESIAN_POINT ( 'NONE',  ( 155.0540265531850537, 2.143131898507880377E-16, -80.93171244307201562 ) ) ;
#4897 = VERTEX_POINT ( 'NONE', #31604 ) ;
#4896 = EDGE_CURVE ( 'NONE', #49775, #46959, #16678, .T. ) ;
#4898 = ADVANCED_FACE ( 'NONE', ( #16189 ), #24403, .F. ) ;
#4899 = ORIENTED_EDGE ( 'NONE', *, *, #42974, .T. ) ;
#4900 = DIRECTION ( 'NONE',  ( -6.938893903907221278E-15, -0.000000000000000000, -1.000000000000000000 ) ) ;
#4901 = ORIENTED_EDGE ( 'NONE', *, *, #35450, .F. ) ;
#4902 = CARTESIAN_POINT ( 'NONE',  ( 155.0540265531850537, 1.025126265847089657, 119.0682875569279560 ) ) ;
#4903 = PLANE ( 'NONE',  #10984 ) ;
#4904 = EDGE_CURVE ( 'NONE', #13485, #19656, #34263, .T. ) ;
#4905 = CARTESIAN_POINT ( 'NONE',  ( -84.94597344681493212, 1.025126265847089657, -80.93171244307201562 ) ) ;
#4906 = CARTESIAN_POINT ( 'NONE',  ( 344.0000000000000000, -165.0000000000001137, -349.9999999999999432 ) ) ;
#4907 = CIRCLE ( 'NONE', #10656, 4.000000000000003553 ) ;
#4908 = EDGE_LOOP ( 'NONE', ( #17498, #20340, #44801, #29110, #43346 ) ) ;
#4909 = EDGE_CURVE ( 'NONE', #17018, #42553, #6381, .T. ) ;
#4910 = CIRCLE ( 'NONE', #30304, 4.000000000000003553 ) ;
#4911 = EDGE_CURVE ( 'NONE', #46936, #20632, #30350, .T. ) ;
#4912 = VECTOR ( 'NONE', #47284, 1000.000000000000000 ) ;
#4913 = FACE_OUTER_BOUND ( 'NONE', #21349, .T. ) ;
#4914 = VERTEX_POINT ( 'NONE', #7990 ) ;
#4915 = CARTESIAN_POINT ( 'NONE',  ( -164.9459734468149463, 2.143131898507880377E-16, 39.06828755692798438 ) ) ;
#4916 = CARTESIAN_POINT ( 'NONE',  ( 4.641001526964561030, 50.00000000000000000, -8.016098858316205167 ) ) ;
#4917 = CARTESIAN_POINT ( 'NONE',  ( -119.9999999999987921, 17.00000000000000000, 30.00000000000000000 ) ) ;
#4918 = CARTESIAN_POINT ( 'NONE',  ( -205.6708471809678827, -1.750000000000009548, -0.2068387089191121020 ) ) ;
#4919 = VECTOR ( 'NONE', #33797, 1000.000000000000000 ) ;
#4920 = AXIS2_PLACEMENT_3D ( 'NONE', #47373, #47125, #24346 ) ;
#4921 = EDGE_CURVE ( 'NONE', #23363, #45598, #36726, .T. ) ;
#4922 = ORIENTED_EDGE ( 'NONE', *, *, #5195, .T. ) ;
#4923 = ORIENTED_EDGE ( 'NONE', *, *, #11591, .F. ) ;
#4924 = DIRECTION ( 'NONE',  ( 0.000000000000000000, 0.000000000000000000, 1.000000000000000000 ) ) ;
#4925 = VECTOR ( 'NONE', #26702, 1000.000000000000000 ) ;
#4926 = ORIENTED_EDGE ( 'NONE', *, *, #7368, .F. ) ;
#4927 = EDGE_CURVE ( 'NONE', #27084, #43076, #48440, .T. ) ;
#4928 = LINE ( 'NONE', #12880, #43793 ) ;
#4929 = CARTESIAN_POINT ( 'NONE',  ( 192.2789002873380184, -1.750000000000009548, 39.79316129108089228 ) ) ;
#4930 = CARTESIAN_POINT ( 'NONE',  ( 85.00000000000056843, 16.00000000000000000, -30.00000000000000000 ) ) ;
#4931 = ORIENTED_EDGE ( 'NONE', *, *, #37246, .F. ) ;
#4932 = DIRECTION ( 'NONE',  ( 0.000000000000000000, 0.000000000000000000, 1.000000000000000000 ) ) ;
#4933 = CARTESIAN_POINT ( 'NONE',  ( -48.44597344681492501, 2.143131898507880377E-16, -160.9317124430720298 ) ) ;
#4934 = LINE ( 'NONE', #31908, #11163 ) ;
#4935 = DIRECTION ( 'NONE',  ( 0.000000000000000000, 0.000000000000000000, 1.000000000000000000 ) ) ;
#4936 = LINE ( 'NONE', #31401, #27188 ) ;
#4937 = ORIENTED_EDGE ( 'NONE', *, *, #13729, .F. ) ;
#4938 = ORIENTED_EDGE ( 'NONE', *, *, #6764, .F. ) ;
#4939 = ORIENTED_EDGE ( 'NONE', *, *, #32846, .F. ) ;
#4940 = LINE ( 'NONE', #47751, #16498 ) ;
#4941 = SURFACE_STYLE_FILL_AREA ( #31915 ) ;
#4942 = FACE_OUTER_BOUND ( 'NONE', #33154, .T. ) ;
#4943 = EDGE_LOOP ( 'NONE', ( #49783, #19621, #40461 ) ) ;
#4944 = CARTESIAN_POINT ( 'NONE',  ( -8.445973446814976526, 0.000000000000000000, -0.9317124430720524764 ) ) ;
#4945 = ORIENTED_EDGE ( 'NONE', *, *, #1846, .T. ) ;
#4946 = CARTESIAN_POINT ( 'NONE',  ( 210.0000000000000568, 2.143131898507881856E-16, -80.93171244307202983 ) ) ;
#4948 = ORIENTED_EDGE ( 'NONE', *, *, #44613, .F. ) ;
#4947 = CIRCLE ( 'NONE', #3290, 2.000000000000001776 ) ;
#4949 =( NAMED_UNIT ( * ) PLANE_ANGLE_UNIT ( ) SI_UNIT ( $, .RADIAN. ) );
#4950 = DIRECTION ( 'NONE',  ( 1.000000000000000000, -1.586032997072805650E-16, -4.759647537211363479E-16 ) ) ;
#4951 = PLANE ( 'NONE',  #21111 ) ;
#4952 = CARTESIAN_POINT ( 'NONE',  ( -46.69597344681494633, 1.750000000000010658, -119.1817124430720440 ) ) ;
#4953 = VECTOR ( 'NONE', #50294, 1000.000000000000000 ) ;
#4954 = CARTESIAN_POINT ( 'NONE',  ( 356.0000000000001137, 185.0000000000000284, 359.9999999999998295 ) ) ;
#4955 = CARTESIAN_POINT ( 'NONE',  ( 2.210477865340801706, 37.43479381012853224, -9.422646554964178023 ) ) ;
#4956 = CARTESIAN_POINT ( 'NONE',  ( 1.249999999999999778, -0.000000000000000000, -3.333333333333333481 ) ) ;
#4957 = EDGE_LOOP ( 'NONE', ( #34276, #33944, #15179, #17325 ) ) ;
#4958 = B_SPLINE_CURVE_WITH_KNOTS ( 'NONE', 3,
 ( #46506, #43632, #5142, #42687 ),
 .UNSPECIFIED., .F., .F.,
 ( 4, 4 ),
 ( 0.9688112071879386722, 0.9724175925769219520 ),
 .UNSPECIFIED. ) ;
#4960 = AXIS2_PLACEMENT_3D ( 'NONE', #922, #47566, #16308 ) ;
#4959 = CARTESIAN_POINT ( 'NONE',  ( -164.4973046169135955, 69.44873401059479079, -93.79675437945476801 ) ) ;
#4961 = AXIS2_PLACEMENT_3D ( 'NONE', #35075, #19126, #50644 ) ;
#4963 = AXIS2_PLACEMENT_3D ( 'NONE', #10016, #44629, #36745 ) ;
#4962 = FACE_OUTER_BOUND ( 'NONE', #22538, .T. ) ;
#4964 = DIRECTION ( 'NONE',  ( 0.000000000000000000, -1.000000000000000000, 0.000000000000000000 ) ) ;
#4965 = EDGE_CURVE ( 'NONE', #9737, #35077, #42029, .T. ) ;
#4966 = DIRECTION ( 'NONE',  ( 0.000000000000000000, 0.000000000000000000, -1.000000000000000000 ) ) ;
#4967 = ADVANCED_FACE ( 'NONE', ( #9486 ), #25396, .T. ) ;
#4968 = ORIENTED_EDGE ( 'NONE', *, *, #16129, .T. ) ;
#4969 = DIRECTION ( 'NONE',  ( -0.000000000000000000, 0.000000000000000000, 1.000000000000000000 ) ) ;
#4970 = ORIENTED_EDGE ( 'NONE', *, *, #13329, .T. ) ;
#4971 = LINE ( 'NONE', #1394, #33610 ) ;
#4972 = ADVANCED_FACE ( 'NONE', ( #21800 ), #21088, .T. ) ;
#4973 = LINE ( 'NONE', #5229, #45981 ) ;
#4974 = EDGE_CURVE ( 'NONE', #45538, #29858, #6146, .T. ) ;
#4975 = ADVANCED_FACE ( 'NONE', ( #21536 ), #2291, .T. ) ;
#4976 = VERTEX_POINT ( 'NONE', #2049 ) ;
#4977 = CARTESIAN_POINT ( 'NONE',  ( 33.30402655318503946, -1.750000000000010658, -119.1817124430720440 ) ) ;
#4978 = CARTESIAN_POINT ( 'NONE',  ( -30.77287599203642188, -12.70002479445974686, 3.199614146704519602 ) ) ;
#4979 = EDGE_CURVE ( 'NONE', #42541, #19163, #14084, .T. ) ;
#4980 = CARTESIAN_POINT ( 'NONE',  ( 9.999999999999994671, 0.04964634316242984985, 9.296265711053614211 ) ) ;
#4981 = EDGE_CURVE ( 'NONE', #38568, #20319, #25728, .T. ) ;
#4982 = ORIENTED_EDGE ( 'NONE', *, *, #1720, .T. ) ;
#4983 = ORIENTED_EDGE ( 'NONE', *, *, #31542, .F. ) ;
#4984 = FACE_BOUND ( 'NONE', #6640, .T. ) ;
#4985 = FACE_OUTER_BOUND ( 'NONE', #42044, .T. ) ;
#4986 = VECTOR ( 'NONE', #39844, 1000.000000000000000 ) ;
#4987 = VECTOR ( 'NONE', #33155, 1000.000000000000000 ) ;
#4988 = EDGE_LOOP ( 'NONE', ( #48397, #20655, #17417, #2673, #10655 ) ) ;
#4989 = EDGE_LOOP ( 'NONE', ( #24819, #3104, #38758 ) ) ;
#4990 = CARTESIAN_POINT ( 'NONE',  ( -48.44597344681495343, 0.000000000000000000, -37.43171244307200141 ) ) ;
#4991 = DIRECTION ( 'NONE',  ( 0.000000000000000000, 0.000000000000000000, 1.000000000000000000 ) ) ;
#4992 = CARTESIAN_POINT ( 'NONE',  ( 224.9999999999999716, -164.9999999999999716, 474.9999999999998863 ) ) ;
#4993 = DIRECTION ( 'NONE',  ( -0.000000000000000000, -0.000000000000000000, -1.000000000000000000 ) ) ;
#4994 = APPLICATION_CONTEXT ( 'automotive_design' ) ;
#4995 = ORIENTED_EDGE ( 'NONE', *, *, #34184, .F. ) ;
#4996 = ORIENTED_EDGE ( 'NONE', *, *, #34082, .F. ) ;
#4997 = VERTEX_POINT ( 'NONE', #45113 ) ;
#4998 = VECTOR ( 'NONE', #29646, 1000.000000000000000 ) ;
#4999 = CARTESIAN_POINT ( 'NONE',  ( 71.55402655318505367, -1.025126265847089657, 42.56828755692799149 ) ) ;
#5000 = CARTESIAN_POINT ( 'NONE',  ( 214.5896300087916302, 164.9999999999999716, 498.0000000000001137 ) ) ;
#5001 = ORIENTED_EDGE ( 'NONE', *, *, #4502, .T. ) ;
#5002 = EDGE_LOOP ( 'NONE', ( #34463, #19470, #9346, #1309 ) ) ;
#5003 = B_SPLINE_CURVE_WITH_KNOTS ( 'NONE', 3,
 ( #50365, #22954, #42206, #39143 ),
 .UNSPECIFIED., .F., .F.,
 ( 4, 4 ),
 ( 0.0001535465953326383131, 0.0005837444810855588412 ),
 .UNSPECIFIED. ) ;
#5004 = CARTESIAN_POINT ( 'NONE',  ( 1.011271242968688311, -0.7347315653655855927, 10.00000000000000000 ) ) ;
#5005 = FACE_OUTER_BOUND ( 'NONE', #31134, .T. ) ;
#5006 = ORIENTED_EDGE ( 'NONE', *, *, #39938, .T. ) ;
#5007 = VERTEX_POINT ( 'NONE', #33865 ) ;
#5008 = EDGE_CURVE ( 'NONE', #29800, #22662, #9994, .T. ) ;
#5009 = CYLINDRICAL_SURFACE ( 'NONE', #29890, 1.750000000000015543 ) ;
#5010 = DIRECTION ( 'NONE',  ( 0.000000000000000000, 0.000000000000000000, -1.000000000000000000 ) ) ;
#5011 = ORIENTED_EDGE ( 'NONE', *, *, #7749, .T. ) ;
#5012 = DIRECTION ( 'NONE',  ( -0.000000000000000000, -0.000000000000000000, -1.000000000000000000 ) ) ;
#5013 = FACE_OUTER_BOUND ( 'NONE', #34492, .T. ) ;
#5014 = PLANE ( 'NONE',  #47391 ) ;
#5015 = CARTESIAN_POINT ( 'NONE',  ( -206.6959734468149463, 1.750000000000010214, -39.18171244307202983 ) ) ;
#5016 = ORIENTED_EDGE ( 'NONE', *, *, #42212, .F. ) ;
#5017 = LINE ( 'NONE', #17077, #20143 ) ;
#5018 = PLANE ( 'NONE',  #17902 ) ;
#5019 = VECTOR ( 'NONE', #19580, 1000.000000000000000 ) ;
#5020 = CARTESIAN_POINT ( 'NONE',  ( 155.0540265531850537, 2.143131898507880377E-16, 165.0000000000000000 ) ) ;
#5021 = MANIFOLD_SOLID_BREP ( 'Square tube 20 X 20 X 2(1)[17]', #722 ) ;
#5022 = PLANE ( 'NONE',  #32724 ) ;
#5023 = CARTESIAN_POINT ( 'NONE',  ( -207.7210997126620384, -1.750000000000010214, 119.7931612910808781 ) ) ;
#5024 = CARTESIAN_POINT ( 'NONE',  ( -1.872530400643504400, 0.3103573527827566680, 9.900811091504554184 ) ) ;
#5025 = CARTESIAN_POINT ( 'NONE',  ( -114.9999999999981526, 17.00000000000000000, 65.00000000000000000 ) ) ;
#5026 = VERTEX_POINT ( 'NONE', #11003 ) ;
#5027 = CARTESIAN_POINT ( 'NONE',  ( -1.275994128725546739, 0.1230186051320636409, 9.948547179989615685 ) ) ;
#5028 = CARTESIAN_POINT ( 'NONE',  ( -48.98697415750977768, -11.03699497439218646, -8.016098858316199838 ) ) ;
#5029 = VERTEX_POINT ( 'NONE', #26145 ) ;
#5030 = CARTESIAN_POINT ( 'NONE',  ( -84.94597344681494633, 2.143131898507880377E-16, -120.9317124430720156 ) ) ;
#5031 = EDGE_CURVE ( 'NONE', #10907, #21273, #49200, .T. ) ;
#5032 = DIRECTION ( 'NONE',  ( 3.172065745548403743E-16, 1.000000000000000000, 0.000000000000000000 ) ) ;
#5033 = CARTESIAN_POINT ( 'NONE',  ( -205.6708471809678827, -1.750000000000009548, -78.15658617722490931 ) ) ;
#5034 =( BOUNDED_CURVE ( )  B_SPLINE_CURVE ( 3, ( #31983, #43756, #931, #12714 ),
 .UNSPECIFIED., .F., .F. ) 
 B_SPLINE_CURVE_WITH_KNOTS ( ( 4, 4 ),
 ( 3.141592653589793116, 4.712388980384689674 ),
 .UNSPECIFIED. ) 
 CURVE ( )  GEOMETRIC_REPRESENTATION_ITEM ( )  RATIONAL_B_SPLINE_CURVE ( ( 1.000000000000000000, 0.8047378541243649375, 0.8047378541243649375, 1.000000000000000000 ) ) 
 REPRESENTATION_ITEM ( '' )  );
#5035 = EDGE_LOOP ( 'NONE', ( #12053, #2783, #27028, #33906 ) ) ;
#5036 = CARTESIAN_POINT ( 'NONE',  ( 181.0000000000000284, -174.9999999999999716, -99.00000000000014211 ) ) ;
#5037 = VERTEX_POINT ( 'NONE', #14853 ) ;
#5038 = ORIENTED_EDGE ( 'NONE', *, *, #6128, .F. ) ;
#5039 = CARTESIAN_POINT ( 'NONE',  ( 4.641001526964560142, 50.00000000000000711, -8.016098858316199838 ) ) ;
#5040 = CARTESIAN_POINT ( 'NONE',  ( -168.4459734468149463, 0.000000000000000000, 122.5682875569279702 ) ) ;
#5041 = VERTEX_POINT ( 'NONE', #14340 ) ;
#5042 = FACE_OUTER_BOUND ( 'NONE', #24888, .T. ) ;
#5043 = CARTESIAN_POINT ( 'NONE',  ( 210.0000000000000568, 2.143131898507881116E-16, -40.93171244307203693 ) ) ;
#5044 = ORIENTED_EDGE ( 'NONE', *, *, #40567, .T. ) ;
#5045 = EDGE_LOOP ( 'NONE', ( #35830, #8512, #6821, #35832, #38909, #31294, #7414, #40020, #46003, #49566, #30367, #37292 ) ) ;
#5046 = AXIS2_PLACEMENT_3D ( 'NONE', #10177, #29932, #10676 ) ;
#5047 = CARTESIAN_POINT ( 'NONE',  ( 210.0000000000000568, 0.000000000000000000, 160.8182875569279702 ) ) ;
#5048 = EDGE_LOOP ( 'NONE', ( #40796, #18660, #49133, #47207 ) ) ;
#5049 = CARTESIAN_POINT ( 'NONE',  ( -4.763548243873389154, 16.57409059453848599, 8.727788335465566760 ) ) ;
#5050 = DIRECTION ( 'NONE',  ( 0.000000000000000000, 0.000000000000000000, 1.000000000000000000 ) ) ;
#5051 = FACE_OUTER_BOUND ( 'NONE', #31565, .T. ) ;
#5052 = VERTEX_POINT ( 'NONE', #42794 ) ;
#5053 = LINE ( 'NONE', #17118, #10391 ) ;
#5054 = AXIS2_PLACEMENT_3D ( 'NONE', #46257, #4217, #377 ) ;
#5055 = CARTESIAN_POINT ( 'NONE',  ( 23.26005729352310425, 44.90397804740356236, 7.906207997025717304 ) ) ;
#5056 = ORIENTED_EDGE ( 'NONE', *, *, #34066, .F. ) ;
#5057 = ORIENTED_EDGE ( 'NONE', *, *, #34937, .F. ) ;
#5058 = ORIENTED_EDGE ( 'NONE', *, *, #11541, .T. ) ;
#5059 = DIRECTION ( 'NONE',  ( -3.172065784643302499E-16, -1.000000000000000000, 2.537652627714642000E-15 ) ) ;
#5060 = CARTESIAN_POINT ( 'NONE',  ( 0.000000000000000000, -184.7999999999999545, 340.1999999999997044 ) ) ;
#5061 = VERTEX_POINT ( 'NONE', #11515 ) ;
#5062 = EDGE_CURVE ( 'NONE', #24255, #26993, #38722, .T. ) ;
#5063 = CARTESIAN_POINT ( 'NONE',  ( 35.05402655318504657, 1.025126265847089879, -77.43171244307200141 ) ) ;
#5064 = DIRECTION ( 'NONE',  ( 0.000000000000000000, 0.000000000000000000, -1.000000000000000000 ) ) ;
#5065 = LINE ( 'NONE', #49323, #10838 ) ;
#5066 = FACE_OUTER_BOUND ( 'NONE', #19576, .T. ) ;
#5067 = CARTESIAN_POINT ( 'NONE',  ( -206.6959734468149463, -1.750000000000010658, -119.1817124430720440 ) ) ;
#5068 = DIRECTION ( 'NONE',  ( 0.000000000000000000, -0.9253776417389547593, -0.3790464617558786942 ) ) ;
#5069 = DIRECTION ( 'NONE',  ( 0.000000000000000000, 0.000000000000000000, -1.000000000000000000 ) ) ;
#5070 = CARTESIAN_POINT ( 'NONE',  ( -165.0000000000000284, 16.00000000000000000, -60.00000000000000000 ) ) ;
#5071 = CARTESIAN_POINT ( 'NONE',  ( -64.99999999999846523, 17.00000000000000000, 35.00000000000000000 ) ) ;
#5072 = PLANE ( 'NONE',  #48594 ) ;
#5073 = UNCERTAINTY_MEASURE_WITH_UNIT (LENGTH_MEASURE( 1.000000000000000082E-05 ), #4266, 'distance_accuracy_value', 'NONE');
#5074 = DIRECTION ( 'NONE',  ( 1.000000000000000000, 0.000000000000000000, -0.000000000000000000 ) ) ;
#5075 = VERTEX_POINT ( 'NONE', #31025 ) ;
#5076 = CARTESIAN_POINT ( 'NONE',  ( 210.0000000000000568, 0.000000000000000000, -37.43171244307202272 ) ) ;
#5077 = VECTOR ( 'NONE', #20845, 1000.000000000000000 ) ;
#5078 = DIRECTION ( 'NONE',  ( -0.000000000000000000, -1.000000000000000000, -0.000000000000000000 ) ) ;
#5079 = FACE_OUTER_BOUND ( 'NONE', #46048, .T. ) ;
#5080 = B_SPLINE_CURVE_WITH_KNOTS ( 'NONE', 3,
 ( #48756, #13648, #29307, #44913 ),
 .UNSPECIFIED., .F., .F.,
 ( 4, 4 ),
 ( 3.397412858278222916E-17, 0.0004072981213156856356 ),
 .UNSPECIFIED. ) ;
#5081 = CARTESIAN_POINT ( 'NONE',  ( 194.3291528190321742, 1.750000000000009548, -0.2068387089191121020 ) ) ;
#5082 = COLOUR_RGB ( '',0.7921568627450980005, 0.8196078431372548767, 0.9333333333333333481 ) ;
#5083 = ORIENTED_EDGE ( 'NONE', *, *, #42429, .T. ) ;
#5084 = CARTESIAN_POINT ( 'NONE',  ( 181.0000000000000284, -182.9999999999999716, -340.0000000000001137 ) ) ;
#5085 = VECTOR ( 'NONE', #35941, 1000.000000000000000 ) ;
#5086 = CARTESIAN_POINT ( 'NONE',  ( 84.99999999999997158, 17.00000000000000000, -114.9999999999999858 ) ) ;
#5087 = ORIENTED_EDGE ( 'NONE', *, *, #5791, .T. ) ;
#5088 = CARTESIAN_POINT ( 'NONE',  ( -44.94597344681493922, 2.143131898507880377E-16, -117.4317124430720156 ) ) ;
#5089 = ADVANCED_FACE ( 'NONE', ( #14594 ), #42542, .F. ) ;
#5090 = DIRECTION ( 'NONE',  ( 1.000000000000000000, 0.000000000000000000, 0.000000000000000000 ) ) ;
#5091 = LINE ( 'NONE', #40260, #39952 ) ;
#5092 = ORIENTED_EDGE ( 'NONE', *, *, #50468, .F. ) ;
#5093 = B_SPLINE_SURFACE_WITH_KNOTS ( 'NONE', 3, 3, ( 
 ( #23002, #26363, #46066, #6860 ),
 ( #49895, #27125, #7116, #38678 ),
 ( #10958, #22502, #2998, #42258 ),
 ( #34841, #50421, #27375, #30984 ) ),
 .UNSPECIFIED., .F., .F., .F.,
 ( 4, 4 ),
 ( 4, 4 ),
 ( 0.000000000000000000, 1.000000000000000000 ),
 ( 0.000000000000000000, 1.000000000000000000 ),
 .UNSPECIFIED. ) ;
#5094 = B_SPLINE_CURVE_WITH_KNOTS ( 'NONE', 3,
 ( #46591, #23550, #50437, #38957 ),
 .UNSPECIFIED., .F., .F.,
 ( 4, 4 ),
 ( 0.000000000000000000, 0.0001252128669263237850 ),
 .UNSPECIFIED. ) ;
#5095 = ORIENTED_EDGE ( 'NONE', *, *, #12796, .T. ) ;
#5096 = ORIENTED_EDGE ( 'NONE', *, *, #20669, .F. ) ;
#5097 = EDGE_CURVE ( 'NONE', #39980, #23318, #32938, .T. ) ;
#5098 = EDGE_CURVE ( 'NONE', #35933, #22449, #36081, .T. ) ;
#5099 = EDGE_LOOP ( 'NONE', ( #8851, #44841, #22069, #50245 ) ) ;
#5100 = DIRECTION ( 'NONE',  ( 1.000000000000000000, 0.000000000000000000, 0.000000000000000000 ) ) ;
#5101 = FACE_OUTER_BOUND ( 'NONE', #6898, .T. ) ;
#5102 = MANIFOLD_SOLID_BREP ( 'Square tube 20 X 20 X 2(1)[4]', #21186 ) ;
#5103 = VERTEX_POINT ( 'NONE', #30256 ) ;
#5104 = LINE ( 'NONE', #48920, #48325 ) ;
#5105 = CARTESIAN_POINT ( 'NONE',  ( -6.174150299305392053, 33.14591993373988998, 8.807470649214879543 ) ) ;
#5106 = EDGE_CURVE ( 'NONE', #32944, #4897, #39522, .T. ) ;
#5107 = DIRECTION ( 'NONE',  ( -0.000000000000000000, 1.000000000000000000, 0.000000000000000000 ) ) ;
#5108 = AXIS2_PLACEMENT_3D ( 'NONE', #18291, #13940, #14460 ) ;
#5109 = EDGE_CURVE ( 'NONE', #44615, #44330, #30011, .T. ) ;
#5110 = CARTESIAN_POINT ( 'NONE',  ( -8.640097307817388383, 14.29292567250791102, -9.458680755252684591 ) ) ;
#5111 = ORIENTED_EDGE ( 'NONE', *, *, #11475, .T. ) ;
#5112 = DIRECTION ( 'NONE',  ( 0.000000000000000000, -1.000000000000000000, 0.000000000000000000 ) ) ;
#5113 = EDGE_CURVE ( 'NONE', #11032, #7258, #6905, .T. ) ;
#5114 = VERTEX_POINT ( 'NONE', #24581 ) ;
#5115 = CARTESIAN_POINT ( 'NONE',  ( 210.0000000000000568, 0.000000000000000000, 162.5682875569279702 ) ) ;
#5116 = CARTESIAN_POINT ( 'NONE',  ( 339.9999999999999432, -171.9999999999998863, 346.9999999999998295 ) ) ;
#5117 = AXIS2_PLACEMENT_3D ( 'NONE', #11211, #26349, #18377 ) ;
#5118 = ORIENTED_EDGE ( 'NONE', *, *, #32213, .T. ) ;
#5119 = ORIENTED_EDGE ( 'NONE', *, *, #5771, .F. ) ;
#5120 = CARTESIAN_POINT ( 'NONE',  ( -5.000000000000000000, 184.8000000000000114, 340.1999999999997044 ) ) ;
#5121 = VECTOR ( 'NONE', #11586, 1000.000000000000000 ) ;
#5122 = DIRECTION ( 'NONE',  ( -1.612977847700450206E-50, 0.000000000000000000, -1.000000000000000000 ) ) ;
#5123 = EDGE_CURVE ( 'NONE', #36547, #14416, #47531, .T. ) ;
#5124 = ORIENTED_EDGE ( 'NONE', *, *, #1720, .F. ) ;
#5125 = ADVANCED_FACE ( 'NONE', ( #11768 ), #230, .F. ) ;
#5126 = CARTESIAN_POINT ( 'NONE',  ( 1.337801958641917199, 1.088266084286984015, 9.928159647716135794 ) ) ;
#5127 = FACE_OUTER_BOUND ( 'NONE', #34294, .T. ) ;
#5128 = CARTESIAN_POINT ( 'NONE',  ( 183.0000000000000000, -164.9999999999999432, -356.0000000000001705 ) ) ;
#5129 = CARTESIAN_POINT ( 'NONE',  ( 195.0540265531851105, 2.143131898507880377E-16, 159.0682875569279702 ) ) ;
#5130 = EDGE_CURVE ( 'NONE', #8610, #593, #27928, .T. ) ;
#5131 = ADVANCED_FACE ( 'NONE', ( #35142 ), #12027, .F. ) ;
#5132 = VECTOR ( 'NONE', #42621, 1000.000000000000000 ) ;
#5133 = ORIENTED_EDGE ( 'NONE', *, *, #3795, .F. ) ;
#5134 = CARTESIAN_POINT ( 'NONE',  ( -206.6959734468149463, -1.750000000000009992, -159.1817124430720298 ) ) ;
#5135 = CARTESIAN_POINT ( 'NONE',  ( -0.6108107228405769140, 1.056024183042602482, 9.963925895596188909 ) ) ;
#5136 = EDGE_CURVE ( 'NONE', #46920, #25256, #4577, .T. ) ;
#5137 = LINE ( 'NONE', #12841, #2664 ) ;
#5138 = EDGE_LOOP ( 'NONE', ( #9903, #6864 ) ) ;
#5139 = ORIENTED_EDGE ( 'NONE', *, *, #11088, .T. ) ;
#5140 = PLANE ( 'NONE',  #42523 ) ;
#5141 = CARTESIAN_POINT ( 'NONE',  ( 181.0000000000000284, 2.775557561562891351E-14, -113.0000000000001563 ) ) ;
#5142 = CARTESIAN_POINT ( 'NONE',  ( -2.097926912204285177, 0.2448757052704424453, 9.890170120223997330 ) ) ;
#5143 = CARTESIAN_POINT ( 'NONE',  ( -168.4459734468149463, 0.000000000000000000, -80.93171244307201562 ) ) ;
#5144 = ORIENTED_EDGE ( 'NONE', *, *, #8038, .T. ) ;
#5145 = CARTESIAN_POINT ( 'NONE',  ( -2.052549611693787135, 0.2039603569406744088, 9.894754715216729224 ) ) ;
#5146 = AXIS2_PLACEMENT_3D ( 'NONE', #33166, #13637, #6696 ) ;
#5147 = CARTESIAN_POINT ( 'NONE',  ( -48.44597344681495343, 0.000000000000000000, 42.56828755692798438 ) ) ;
#5148 = LINE ( 'NONE', #36744, #14333 ) ;
#5149 = ADVANCED_FACE ( 'NONE', ( #31536 ), #4326, .F. ) ;
#5150 = CARTESIAN_POINT ( 'NONE',  ( -5.000000000000000000, 165.2000000000000171, 359.7999999999997840 ) ) ;
#5151 = EDGE_LOOP ( 'NONE', ( #47247, #28527, #3595, #14498 ) ) ;
#5152 = EDGE_CURVE ( 'NONE', #39676, #9652, #15872, .T. ) ;
#5153 = ORIENTED_EDGE ( 'NONE', *, *, #19035, .T. ) ;
#5154 = ADVANCED_FACE ( 'NONE', ( #40231 ), #27671, .F. ) ;
#5155 = PLANE ( 'NONE',  #28610 ) ;
#5156 = ORIENTED_EDGE ( 'NONE', *, *, #11085, .F. ) ;
#5157 = CYLINDRICAL_SURFACE ( 'NONE', #35274, 1.750000000000001554 ) ;
#5158 = EDGE_CURVE ( 'NONE', #30382, #48120, #37725, .T. ) ;
#5159 = CIRCLE ( 'NONE', #32211, 6.000000000000000888 ) ;
#5160 = FACE_OUTER_BOUND ( 'NONE', #46527, .T. ) ;
#5161 = B_SPLINE_CURVE_WITH_KNOTS ( 'NONE', 3,
 ( #19063, #34752, #47249, #4440 ),
 .UNSPECIFIED., .F., .F.,
 ( 4, 4 ),
 ( 0.000000000000000000, 0.2545280377015988749 ),
 .UNSPECIFIED. ) ;
#5162 = DIRECTION ( 'NONE',  ( -0.000000000000000000, -0.000000000000000000, -1.000000000000000000 ) ) ;
#5163 = DIRECTION ( 'NONE',  ( -1.000000000000000000, -0.000000000000000000, -0.000000000000000000 ) ) ;
#5164 = ORIENTED_EDGE ( 'NONE', *, *, #36112, .T. ) ;
#5165 = EDGE_CURVE ( 'NONE', #30282, #4735, #15614, .T. ) ;
#5166 = CARTESIAN_POINT ( 'NONE',  ( -5.320787806781440921, 8.466948512633457824, -1.544988095791843818E-15 ) ) ;
#5168 = B_SPLINE_CURVE_WITH_KNOTS ( 'NONE', 3,
 ( #39715, #24814, #4788, #29169 ),
 .UNSPECIFIED., .F., .F.,
 ( 4, 4 ),
 ( 2.262036551361258466E-17, 0.0004072981213155198611 ),
 .UNSPECIFIED. ) ;
#5167 = AXIS2_PLACEMENT_3D ( 'NONE', #17587, #21943, #1941 ) ;
#5169 = EDGE_LOOP ( 'NONE', ( #16225, #46487, #29076, #34908 ) ) ;
#5170 = CARTESIAN_POINT ( 'NONE',  ( 339.9999999999998863, -168.9999999999999432, 339.9999999999997726 ) ) ;
#5171 = CARTESIAN_POINT ( 'NONE',  ( -10.00000000000000533, 0.4417425667975929948, 5.558078895815943277 ) ) ;
#5172 = CARTESIAN_POINT ( 'NONE',  ( 16.76006782980217125, -2.050259795448531541, 9.178419661560148768 ) ) ;
#5173 = CARTESIAN_POINT ( 'NONE',  ( -128.4459734468149463, 1.025126265847081664, -117.4317124430720440 ) ) ;
#5174 = DIRECTION ( 'NONE',  ( -1.000000000000000000, 0.000000000000000000, 0.000000000000000000 ) ) ;
#5175 = ORIENTED_EDGE ( 'NONE', *, *, #31986, .F. ) ;
#5176 = EDGE_LOOP ( 'NONE', ( #23301, #12458, #37630, #48825, #24406, #11538 ) ) ;
#5177 = CARTESIAN_POINT ( 'NONE',  ( 210.0000000000000568, 0.000000000000000000, -39.18171244307202983 ) ) ;
#5178 = ADVANCED_FACE ( 'NONE', ( #35652 ), #39232, .T. ) ;
#5179 =( BOUNDED_CURVE ( )  B_SPLINE_CURVE ( 3, ( #25306, #21444, #40462, #48859 ),
 .UNSPECIFIED., .F., .F. ) 
 B_SPLINE_CURVE_WITH_KNOTS ( ( 4, 4 ),
 ( 1.570796326794896780, 3.141592653589793116 ),
 .UNSPECIFIED. ) 
 CURVE ( )  GEOMETRIC_REPRESENTATION_ITEM ( )  RATIONAL_B_SPLINE_CURVE ( ( 1.000000000000000000, 0.8047378541243650485, 0.8047378541243650485, 1.000000000000000000 ) ) 
 REPRESENTATION_ITEM ( '' )  );
#5180 = VERTEX_POINT ( 'NONE', #43307 ) ;
#5181 = CARTESIAN_POINT ( 'NONE',  ( 85.00000000000184741, 17.00000000000000000, 90.00000000000000000 ) ) ;
#5182 = DIRECTION ( 'NONE',  ( 6.203854594147707562E-25, -2.067951531382569187E-25, 1.000000000000000000 ) ) ;
#5183 = CARTESIAN_POINT ( 'NONE',  ( 0.000000000000000000, 0.000000000000000000, 0.000000000000000000 ) ) ;
#5184 = EDGE_CURVE ( 'NONE', #38709, #9291, #35281, .T. ) ;
#5185 = ORIENTED_EDGE ( 'NONE', *, *, #3628, .F. ) ;
#5186 = CARTESIAN_POINT ( 'NONE',  ( 3.627208138665139803, 3.377809768366639828E-15, -27.58190990837850265 ) ) ;
#5187 =( BOUNDED_CURVE ( )  B_SPLINE_CURVE ( 3, ( #11474, #3775, #7633, #19424 ),
 .UNSPECIFIED., .F., .F. ) 
 B_SPLINE_CURVE_WITH_KNOTS ( ( 4, 4 ),
 ( 3.141592653589793116, 4.712388980384689674 ),
 .UNSPECIFIED. ) 
 CURVE ( )  GEOMETRIC_REPRESENTATION_ITEM ( )  RATIONAL_B_SPLINE_CURVE ( ( 1.000000000000000000, 0.8047378541243649375, 0.8047378541243649375, 1.000000000000000000 ) ) 
 REPRESENTATION_ITEM ( '' )  );
#5188 = CARTESIAN_POINT ( 'NONE',  ( 342.0000000000000000, 165.0000000000000000, -106.0000000000001990 ) ) ;
#5189 = B_SPLINE_CURVE_WITH_KNOTS ( 'NONE', 3,
 ( #35279, #27311, #42433, #34507 ),
 .UNSPECIFIED., .F., .F.,
 ( 4, 4 ),
 ( 0.000000000000000000, 0.2637263876330695478 ),
 .UNSPECIFIED. ) ;
#5190 = LINE ( 'NONE', #35572, #21043 ) ;
#5191 = CARTESIAN_POINT ( 'NONE',  ( 210.0000000000000568, 0.000000000000000000, 0.8182875569279768335 ) ) ;
#5192 = LINE ( 'NONE', #16998, #17585 ) ;
#5193 = DIRECTION ( 'NONE',  ( -1.000000000000000000, 0.000000000000000000, 0.000000000000000000 ) ) ;
#5194 = EDGE_CURVE ( 'NONE', #15554, #17436, #25419, .T. ) ;
#5196 = ORIENTED_EDGE ( 'NONE', *, *, #14651, .F. ) ;
#5195 = EDGE_CURVE ( 'NONE', #31812, #8645, #12515, .T. ) ;
#5197 = VERTEX_POINT ( 'NONE', #46872 ) ;
#5198 = VECTOR ( 'NONE', #3506, 1000.000000000000000 ) ;
#5199 = VERTEX_POINT ( 'NONE', #19716 ) ;
#5200 = CARTESIAN_POINT ( 'NONE',  ( 191.5540265531851105, 0.000000000000000000, 165.0000000000000000 ) ) ;
#5201 = ADVANCED_FACE ( 'NONE', ( #20464 ), #986, .T. ) ;
#5202 = CARTESIAN_POINT ( 'NONE',  ( 181.0000000000000000, -174.9999999999999716, -360.0000000000001705 ) ) ;
#5203 = CARTESIAN_POINT ( 'NONE',  ( -175.0000000000000000, 15.00000000000000000, 122.5000000000000142 ) ) ;
#5204 = EDGE_CURVE ( 'NONE', #49960, #8523, #49876, .T. ) ;
#5205 =( BOUNDED_CURVE ( )  B_SPLINE_CURVE ( 3, ( #30857, #12342, #24168, #7756 ),
 .UNSPECIFIED., .F., .T. ) 
 B_SPLINE_CURVE_WITH_KNOTS ( ( 4, 4 ),
 ( 0.000000000000000000, 1.570796326794896558 ),
 .UNSPECIFIED. ) 
 CURVE ( )  GEOMETRIC_REPRESENTATION_ITEM ( )  RATIONAL_B_SPLINE_CURVE ( ( 1.000000000000000000, 0.8047378541243649375, 0.8047378541243649375, 1.000000000000000000 ) ) 
 REPRESENTATION_ITEM ( '' )  );
#5206 = LINE ( 'NONE', #20851, #28066 ) ;
#5207 = ORIENTED_EDGE ( 'NONE', *, *, #46093, .T. ) ;
#5208 = EDGE_CURVE ( 'NONE', #21162, #17655, #21727, .T. ) ;
#5209 = CARTESIAN_POINT ( 'NONE',  ( -8.445973446814976526, 0.000000000000000000, 165.0000000000000000 ) ) ;
#5210 = VERTEX_POINT ( 'NONE', #17630 ) ;
#5211 = CARTESIAN_POINT ( 'NONE',  ( 355.9999999999998863, -185.0000000000002558, -360.0000000000003411 ) ) ;
#5212 = DIRECTION ( 'NONE',  ( 0.000000000000000000, -1.000000000000000000, -0.000000000000000000 ) ) ;
#5213 = DIRECTION ( 'NONE',  ( -0.000000000000000000, -0.000000000000000000, 1.000000000000000000 ) ) ;
#5214 =( LENGTH_UNIT ( ) NAMED_UNIT ( * ) SI_UNIT ( .MILLI., .METRE. ) );
#5215 = DIRECTION ( 'NONE',  ( -0.000000000000000000, 0.000000000000000000, 1.000000000000000000 ) ) ;
#5216 = CARTESIAN_POINT ( 'NONE',  ( 13.59579750444771307, -10.60877755095900632, 8.727788335465566760 ) ) ;
#5217 = EDGE_LOOP ( 'NONE', ( #26376, #30953, #46345, #22316 ) ) ;
#5218 = B_SPLINE_SURFACE_WITH_KNOTS ( 'NONE', 3, 3, ( 
 ( #28915, #45039, #5049, #13754 ),
 ( #28663, #32534, #24820, #44791 ),
 ( #29414, #1229, #41210, #9913 ),
 ( #44530, #9662, #44043, #20710 ) ),
 .UNSPECIFIED., .F., .F., .F.,
 ( 4, 4 ),
 ( 4, 4 ),
 ( 0.000000000000000000, 1.000000000000000000 ),
 ( 0.000000000000000000, 1.000000000000000000 ),
 .UNSPECIFIED. ) ;
#5219 = CARTESIAN_POINT ( 'NONE',  ( -69.99999999999847944, 17.00000000000000000, 35.00000000000000000 ) ) ;
#5220 = DIRECTION ( 'NONE',  ( 0.000000000000000000, 0.000000000000000000, 1.000000000000000000 ) ) ;
#5221 = VECTOR ( 'NONE', #20152, 1000.000000000000000 ) ;
#5222 = CARTESIAN_POINT ( 'NONE',  ( 181.0000000000000000, -184.9999999999999716, -340.0000000000001137 ) ) ;
#5223 = ORIENTED_EDGE ( 'NONE', *, *, #18836, .F. ) ;
#5224 = EDGE_CURVE ( 'NONE', #43947, #44210, #1157, .T. ) ;
#5225 = CARTESIAN_POINT ( 'NONE',  ( 181.0000000000000000, -184.9999999999999716, -356.0000000000001705 ) ) ;
#5226 = ORIENTED_EDGE ( 'NONE', *, *, #41644, .T. ) ;
#5227 = CARTESIAN_POINT ( 'NONE',  ( 135.0000000000012790, 16.00000000000000000, 30.00000000000000000 ) ) ;
#5228 = DIRECTION ( 'NONE',  ( 0.000000000000000000, -0.9749645535258959494, -0.2223603367690620558 ) ) ;
#5229 = CARTESIAN_POINT ( 'NONE',  ( 181.0000000000000000, -166.9999999999999432, -350.0000000000001705 ) ) ;
#5230 = ORIENTED_EDGE ( 'NONE', *, *, #2406, .T. ) ;
#5231 = ORIENTED_EDGE ( 'NONE', *, *, #20245, .F. ) ;
#5232 = CARTESIAN_POINT ( 'NONE',  ( 181.0000000000000000, -256.5000000000000000, -114.9999999999999574 ) ) ;
#5233 = CARTESIAN_POINT ( 'NONE',  ( 24.39427009665985224, 44.07992421011656603, 8.807470649214879543 ) ) ;
#5234 = DIRECTION ( 'NONE',  ( 0.000000000000000000, 1.604368532695312981E-16, 1.000000000000000000 ) ) ;
#5235 = DIRECTION ( 'NONE',  ( 1.586032892321651989E-16, -8.666415220619855873E-32, 1.000000000000000000 ) ) ;
#5236 = VECTOR ( 'NONE', #17309, 1000.000000000000000 ) ;
#5237 = EDGE_CURVE ( 'NONE', #31581, #24012, #33305, .T. ) ;
#5238 = ORIENTED_EDGE ( 'NONE', *, *, #40359, .F. ) ;
#5239 = EDGE_LOOP ( 'NONE', ( #45106, #33408, #44020, #33929 ) ) ;
#5240 = CARTESIAN_POINT ( 'NONE',  ( -6.408332700304190332, -7.676800896350769676, 0.000000000000000000 ) ) ;
#5241 = CARTESIAN_POINT ( 'NONE',  ( 5.888214538810389698, 16.20866436362417673, 8.727788335465566760 ) ) ;
#5242 = AXIS2_PLACEMENT_3D ( 'NONE', #4654, #5900, #14605 ) ;
#5243 = EDGE_LOOP ( 'NONE', ( #4659, #1921, #31577, #49527, #10802, #20257 ) ) ;
#5244 = ORIENTED_EDGE ( 'NONE', *, *, #13930, .T. ) ;
#5245 = DIRECTION ( 'NONE',  ( -1.860490536778032451E-50, 0.000000000000000000, 1.000000000000000000 ) ) ;
#5246 = CYLINDRICAL_SURFACE ( 'NONE', #21674, 2.000000000000001776 ) ;
#5247 = CARTESIAN_POINT ( 'NONE',  ( 191.5540265531851105, 0.000000000000000000, -77.43171244307204404 ) ) ;
#5248 = PLANE ( 'NONE',  #28891 ) ;
#5249 = ORIENTED_EDGE ( 'NONE', *, *, #39960, .F. ) ;
#5250 = ORIENTED_EDGE ( 'NONE', *, *, #17713, .T. ) ;
#5251 = ORIENTED_EDGE ( 'NONE', *, *, #37371, .T. ) ;
#5252 = LINE ( 'NONE', #27857, #43890 ) ;
#5253 = EDGE_CURVE ( 'NONE', #9269, #16197, #41143, .T. ) ;
#5254 = EDGE_CURVE ( 'NONE', #27283, #42074, #29435, .T. ) ;
#5255 = DIRECTION ( 'NONE',  ( -1.000000000000000000, 0.000000000000000000, 0.000000000000000000 ) ) ;
#5256 = ORIENTED_EDGE ( 'NONE', *, *, #25549, .T. ) ;
#5257 = ORIENTED_EDGE ( 'NONE', *, *, #3608, .T. ) ;
#5258 = CARTESIAN_POINT ( 'NONE',  ( -15.73090589902298042, -29.60029367929041655, 1.847720168420772691 ) ) ;
#5259 = EDGE_CURVE ( 'NONE', #38406, #13052, #15736, .T. ) ;
#5260 = LINE ( 'NONE', #4757, #1934 ) ;
#5261 = EDGE_CURVE ( 'NONE', #38804, #41095, #10189, .T. ) ;
#5262 = ORIENTED_EDGE ( 'NONE', *, *, #43730, .T. ) ;
#5263 = ORIENTED_EDGE ( 'NONE', *, *, #16747, .T. ) ;
#5264 = EDGE_CURVE ( 'NONE', #39465, #8778, #21489, .T. ) ;
#5265 = FACE_OUTER_BOUND ( 'NONE', #42762, .T. ) ;
#5266 = CARTESIAN_POINT ( 'NONE',  ( -127.7210997126620242, 1.749999999999996669, 81.84341382277506227 ) ) ;
#5267 = EDGE_LOOP ( 'NONE', ( #16213, #13340, #29410, #39219, #28843, #6897 ) ) ;
#5268 = EDGE_CURVE ( 'NONE', #39269, #42413, #13769, .T. ) ;
#5269 = FACE_OUTER_BOUND ( 'NONE', #43195, .T. ) ;
#5270 = LINE ( 'NONE', #35587, #30947 ) ;
#5271 = CARTESIAN_POINT ( 'NONE',  ( 210.0000000000000568, 2.143131898507881116E-16, 39.06828755692797728 ) ) ;
#5272 = AXIS2_PLACEMENT_3D ( 'NONE', #1716, #29409, #36381 ) ;
#5273 = CARTESIAN_POINT ( 'NONE',  ( 210.0000000000000568, 0.000000000000000000, -159.1817124430720298 ) ) ;
#5274 = ORIENTED_EDGE ( 'NONE', *, *, #32620, .F. ) ;
#5275 = AXIS2_PLACEMENT_3D ( 'NONE', #33892, #22578, #42072 ) ;
#5276 = DIRECTION ( 'NONE',  ( 0.8090169943749465631, 0.5877852522924742473, 0.000000000000000000 ) ) ;
#5277 = CARTESIAN_POINT ( 'NONE',  ( -119.9999999999981668, 17.00000000000000000, 90.00000000000000000 ) ) ;
#5278 = EDGE_CURVE ( 'NONE', #46833, #29795, #28929, .T. ) ;
#5279 = CARTESIAN_POINT ( 'NONE',  ( 153.3040265531850537, 1.750000000000010658, 120.8182875569279702 ) ) ;
#5280 = PLANE ( 'NONE',  #23440 ) ;
#5281 = AXIS2_PLACEMENT_3D ( 'NONE', #42718, #26838, #38911 ) ;
#5282 = DIRECTION ( 'NONE',  ( 6.203854594147707562E-25, -2.067951531382569187E-25, 1.000000000000000000 ) ) ;
#5283 = DIRECTION ( 'NONE',  ( 1.000000000000000000, 0.000000000000000000, 0.000000000000000000 ) ) ;
#5284 = CARTESIAN_POINT ( 'NONE',  ( -8.445973446814976526, 0.000000000000000000, -117.4317124430720156 ) ) ;
#5285 = CARTESIAN_POINT ( 'NONE',  ( -46.69597344681494633, -1.750000000000010658, 80.81828755692798438 ) ) ;
#5286 = EDGE_LOOP ( 'NONE', ( #33348, #36382, #21791, #17622 ) ) ;
#5287 = AXIS2_PLACEMENT_3D ( 'NONE', #877, #4718, #17016 ) ;
#5288 = CARTESIAN_POINT ( 'NONE',  ( -32.57170742938676256, -18.58316106410400437, 7.697694107796192675 ) ) ;
#5289 = APPLICATION_CONTEXT ( 'automotive_design' ) ;
#5290 = CIRCLE ( 'NONE', #40536, 3.500000000000003109 ) ;
#5291 = VERTEX_POINT ( 'NONE', #41228 ) ;
#5292 = CARTESIAN_POINT ( 'NONE',  ( 181.0000000000000568, 175.0000000000000284, 339.9999999999998863 ) ) ;
#5293 = CARTESIAN_POINT ( 'NONE',  ( 342.8284271247460993, 183.0000000000002558, -358.0000000000002842 ) ) ;
#5294 = ORIENTED_EDGE ( 'NONE', *, *, #5261, .F. ) ;
#5295 = CARTESIAN_POINT ( 'NONE',  ( -1.553222296440334826, 1.431397764604077860, 9.884520316594374023 ) ) ;
#5296 = EDGE_LOOP ( 'NONE', ( #35875, #32658, #39711, #202, #25420, #36700 ) ) ;
#5297 = CARTESIAN_POINT ( 'NONE',  ( -33.86622497129646092, 3.037805405905158462, 7.906207997025717304 ) ) ;
#5298 = EDGE_CURVE ( 'NONE', #32944, #4845, #46364, .T. ) ;
#5299 = CARTESIAN_POINT ( 'NONE',  ( 32.27890028733795447, -1.750000000000010214, -120.2068387089191219 ) ) ;
#5300 = ORIENTED_EDGE ( 'NONE', *, *, #42207, .T. ) ;
#5301 = CARTESIAN_POINT ( 'NONE',  ( -5.505322767148756569, 37.09368438467003415, 8.914903342594564961 ) ) ;
#5302 = DIRECTION ( 'NONE',  ( 1.000000000000000000, 0.000000000000000000, 0.000000000000000000 ) ) ;
#5303 = VECTOR ( 'NONE', #18047, 1000.000000000000000 ) ;
#5304 = VERTEX_POINT ( 'NONE', #21474 ) ;
#5305 = ORIENTED_EDGE ( 'NONE', *, *, #14245, .T. ) ;
#5306 = CARTESIAN_POINT ( 'NONE',  ( 74.32915281903215998, 1.750000000000010214, 81.84341382277507648 ) ) ;
#5307 = VERTEX_POINT ( 'NONE', #13016 ) ;
#5308 = AXIS2_PLACEMENT_3D ( 'NONE', #16570, #47819, #12711 ) ;
#5309 = CARTESIAN_POINT ( 'NONE',  ( 0.3862712429686894211, -1.188820645368940276, 9.972675548442463622 ) ) ;
#5310 = DIRECTION ( 'NONE',  ( 0.000000000000000000, 0.000000000000000000, -1.000000000000000000 ) ) ;
#5311 = CARTESIAN_POINT ( 'NONE',  ( -25.60949810002096783, -43.19700938445173932, 1.847720168420772691 ) ) ;
#5312 = EDGE_LOOP ( 'NONE', ( #20604, #5207, #2100, #13380, #30065, #50084 ) ) ;
#5313 = CARTESIAN_POINT ( 'NONE',  ( -124.9459734468149463, 2.143131898507847836E-16, -157.4317124430720582 ) ) ;
#5314 = EDGE_CURVE ( 'NONE', #17018, #6332, #1739, .T. ) ;
#5315 = CARTESIAN_POINT ( 'NONE',  ( 12.78770032058947237, 31.68259716188277864, 7.455576670931136185 ) ) ;
#5316 = ORIENTED_EDGE ( 'NONE', *, *, #3735, .F. ) ;
#5317 = ORIENTED_EDGE ( 'NONE', *, *, #18328, .F. ) ;
#5318 = ORIENTED_EDGE ( 'NONE', *, *, #14260, .T. ) ;
#5319 = CARTESIAN_POINT ( 'NONE',  ( -214.9999999999999432, -172.9999999999999716, 232.0000000000000284 ) ) ;
#5320 = DIRECTION ( 'NONE',  ( -1.000000000000000000, -0.000000000000000000, -0.000000000000000000 ) ) ;
#5321 = ORIENTED_EDGE ( 'NONE', *, *, #26939, .T. ) ;
#5322 = EDGE_CURVE ( 'NONE', #22009, #36281, #11331, .T. ) ;
#5323 = DIRECTION ( 'NONE',  ( 0.000000000000000000, 0.000000000000000000, 1.000000000000000000 ) ) ;
#5324 = CARTESIAN_POINT ( 'NONE',  ( 360.0000000000001137, -172.0000000000000000, -3.000000000000058620 ) ) ;
#5325 = EDGE_CURVE ( 'NONE', #42661, #3719, #1245, .T. ) ;
#5326 = DIRECTION ( 'NONE',  ( -3.172065745548403743E-16, -1.000000000000000000, 0.000000000000000000 ) ) ;
#5327 = AXIS2_PLACEMENT_3D ( 'NONE', #3117, #7235, #50532 ) ;
#5328 = CARTESIAN_POINT ( 'NONE',  ( -124.9459734468149321, 1.025126265847082108, 82.56828755692798438 ) ) ;
#5329 = LINE ( 'NONE', #29437, #38449 ) ;
#5330 = LINE ( 'NONE', #20729, #45365 ) ;
#5331 = AXIS2_PLACEMENT_3D ( 'NONE', #44627, #1568, #5655 ) ;
#5333 = EDGE_CURVE ( 'NONE', #47613, #980, #40488, .T. ) ;
#5332 = CARTESIAN_POINT ( 'NONE',  ( 25.63461350838963426, -43.17876197216376966, -8.016098858316199838 ) ) ;
#5334 = CARTESIAN_POINT ( 'NONE',  ( 79.99999999999997158, 17.00000000000000000, -114.9999999999999858 ) ) ;
#5335 = FACE_OUTER_BOUND ( 'NONE', #9411, .T. ) ;
#5336 = CARTESIAN_POINT ( 'NONE',  ( 15.57957361750251302, 5.755602074545510760, 3.266473740018926541 ) ) ;
#5337 = DIRECTION ( 'NONE',  ( 9.711650524620651178E-33, -1.223873602809432483E-48, 1.000000000000000000 ) ) ;
#5338 = CIRCLE ( 'NONE', #38104, 1.880036658038868103 ) ;
#5339 = CARTESIAN_POINT ( 'NONE',  ( -11.73320209285699889, 11.96063479729179768, 9.403735324607438884 ) ) ;
#5340 = ORIENTED_EDGE ( 'NONE', *, *, #28158, .F. ) ;
#5341 = LINE ( 'NONE', #5076, #50699 ) ;
#5342 =( BOUNDED_CURVE ( )  B_SPLINE_CURVE ( 3, ( #2921, #30140, #45503, #34505 ),
 .UNSPECIFIED., .F., .F. ) 
 B_SPLINE_CURVE_WITH_KNOTS ( ( 4, 4 ),
 ( 4.712388980384689674, 6.283185307179586232 ),
 .UNSPECIFIED. ) 
 CURVE ( )  GEOMETRIC_REPRESENTATION_ITEM ( )  RATIONAL_B_SPLINE_CURVE ( ( 1.000000000000000000, 0.8047378541243649375, 0.8047378541243649375, 1.000000000000000000 ) ) 
 REPRESENTATION_ITEM ( '' )  );
#5343 = CARTESIAN_POINT ( 'NONE',  ( 181.0000000000000284, -174.9999999999999716, -115.0000000000001563 ) ) ;
#5344 = CARTESIAN_POINT ( 'NONE',  ( -128.4459734468149179, 0.000000000000000000, 165.0000000000000000 ) ) ;
#5345 = AXIS2_PLACEMENT_3D ( 'NONE', #30844, #38552, #4393 ) ;
#5346 = VECTOR ( 'NONE', #20854, 1000.000000000000000 ) ;
#5347 = LINE ( 'NONE', #44824, #40202 ) ;
#5348 = EDGE_LOOP ( 'NONE', ( #11752, #34730, #47560, #9812 ) ) ;
#5349 = DIRECTION ( 'NONE',  ( -0.000000000000000000, 1.000000000000000000, 0.000000000000000000 ) ) ;
#5350 = EDGE_LOOP ( 'NONE', ( #17797, #28284, #30245, #12155 ) ) ;
#5351 = DIRECTION ( 'NONE',  ( -0.000000000000000000, -1.000000000000000000, -0.000000000000000000 ) ) ;
#5352 = CARTESIAN_POINT ( 'NONE',  ( 181.0000000000000000, -182.9999999999999716, -350.0000000000001705 ) ) ;
#5353 = EDGE_LOOP ( 'NONE', ( #24773, #47702, #43505, #11575 ) ) ;
#5354 = CARTESIAN_POINT ( 'NONE',  ( -0.4402948852767746279, 2.015117899693936732, 9.894754715216722118 ) ) ;
#5355 = ORIENTED_EDGE ( 'NONE', *, *, #10249, .T. ) ;
#5356 = ORIENTED_EDGE ( 'NONE', *, *, #1852, .T. ) ;
#5357 = ADVANCED_FACE ( 'NONE', ( #36667 ), #2730, .T. ) ;
#5358 = AXIS2_PLACEMENT_3D ( 'NONE', #34993, #19305, #23154 ) ;
#5359 = EDGE_LOOP ( 'NONE', ( #4141, #20638, #11759, #36577, #24083, #2743, #17002, #41325, #14180, #1513, #25332, #49327 ) ) ;
#5360 = CARTESIAN_POINT ( 'NONE',  ( -167.7210997126620384, -1.750000000000009548, 39.79316129108089228 ) ) ;
#5361 = MANIFOLD_SOLID_BREP ( 'CirPattern1', #23649 ) ;
#5362 = ORIENTED_EDGE ( 'NONE', *, *, #34367, .F. ) ;
#5363 = DIRECTION ( 'NONE',  ( -5.551115123125782086E-17, -0.7071067811865475727, -0.7071067811865474617 ) ) ;
#5364 = CARTESIAN_POINT ( 'NONE',  ( -6.875132362119187768, 50.00000000000000711, 8.356839323120299312 ) ) ;
#5365 = CARTESIAN_POINT ( 'NONE',  ( -48.44597344681495343, 0.000000000000000000, 165.0000000000000000 ) ) ;
#5366 = VECTOR ( 'NONE', #36991, 1000.000000000000000 ) ;
#5367 = CARTESIAN_POINT ( 'NONE',  ( 0.8433491450857230065, -0.9182416014173362395, 9.981352469109934233 ) ) ;
#5368 = ORIENTED_EDGE ( 'NONE', *, *, #46578, .T. ) ;
#5369 = CARTESIAN_POINT ( 'NONE',  ( -206.6959734468149463, 0.000000000000000000, 165.0000000000000000 ) ) ;
#5370 = VECTOR ( 'NONE', #38706, 1000.000000000000000 ) ;
#5371 = ORIENTED_EDGE ( 'NONE', *, *, #16278, .F. ) ;
#5372 = DIRECTION ( 'NONE',  ( -1.000000000000000000, 0.000000000000000000, -0.000000000000000000 ) ) ;
#5373 = CARTESIAN_POINT ( 'NONE',  ( 356.0000000000001137, 165.0000000000000000, -108.0000000000002132 ) ) ;
#5374 = VERTEX_POINT ( 'NONE', #46313 ) ;
#5375 = VECTOR ( 'NONE', #24342, 1000.000000000000000 ) ;
#5376 = EDGE_LOOP ( 'NONE', ( #3204, #47357, #7903, #27457 ) ) ;
#5377 = ORIENTED_EDGE ( 'NONE', *, *, #34426, .T. ) ;
#5378 = PLANE ( 'NONE',  #4878 ) ;
#5379 = CARTESIAN_POINT ( 'NONE',  ( -8.760073316077734873, 222.4999999999999716, -228.6347188485896140 ) ) ;
#5380 = EDGE_LOOP ( 'NONE', ( #10022, #34348, #22990, #49445, #2829 ) ) ;
#5381 = VECTOR ( 'NONE', #13271, 1000.000000000000000 ) ;
#5382 = AXIS2_PLACEMENT_3D ( 'NONE', #3453, #10158, #33774 ) ;
#5383 = CARTESIAN_POINT ( 'NONE',  ( -164.9459734468149463, 2.143131898507880377E-16, 165.0000000000000000 ) ) ;
#5384 = CARTESIAN_POINT ( 'NONE',  ( -208.4459734468148611, -1.025126265847089435, -157.4317124430720582 ) ) ;
#5385 = ORIENTED_EDGE ( 'NONE', *, *, #20891, .F. ) ;
#5386 = CYLINDRICAL_SURFACE ( 'NONE', #16329, 1.750000000000008438 ) ;
#5388 = EDGE_CURVE ( 'NONE', #4058, #47505, #16583, .T. ) ;
#5387 = CARTESIAN_POINT ( 'NONE',  ( 210.0000000000000568, 2.143131898507881856E-16, -120.9317124430720582 ) ) ;
#5389 = LINE ( 'NONE', #13830, #33860 ) ;
#5390 = ORIENTED_EDGE ( 'NONE', *, *, #47503, .F. ) ;
#5391 = ORIENTED_EDGE ( 'NONE', *, *, #27997, .F. ) ;
#5392 = APPLICATION_PROTOCOL_DEFINITION ( 'draft international standard', 'automotive_design', 1998, #21033 ) ;
#5393 = CARTESIAN_POINT ( 'NONE',  ( -6.695973446814940111, 1.750000000000023759, -39.18171244307202983 ) ) ;
#5394 = DIRECTION ( 'NONE',  ( 0.000000000000000000, 0.000000000000000000, -1.000000000000000000 ) ) ;
#5395 = VECTOR ( 'NONE', #37270, 1000.000000000000000 ) ;
#5397 = AXIS2_PLACEMENT_3D ( 'NONE', #34541, #50123, #30691 ) ;
#5396 = CARTESIAN_POINT ( 'NONE',  ( -14.52758583651993618, -8.922352469211071835, 8.953103998512858652 ) ) ;
#5398 = CARTESIAN_POINT ( 'NONE',  ( 342.0000000000000000, 182.1715728752538439, 357.1715728752535597 ) ) ;
#5399 = VERTEX_POINT ( 'NONE', #42482 ) ;
#5400 = CARTESIAN_POINT ( 'NONE',  ( 25.40454589245968364, 27.58367357691700406, -8.192531242611265085 ) ) ;
#5401 = CARTESIAN_POINT ( 'NONE',  ( -48.33712804702535948, -13.03701565032741527, -9.367992836599954742 ) ) ;
#5402 = CARTESIAN_POINT ( 'NONE',  ( 210.0000000000000568, 0.000000000000000000, 120.8182875569279702 ) ) ;
#5403 = FACE_OUTER_BOUND ( 'NONE', #4208, .T. ) ;
#5404 = AXIS2_PLACEMENT_3D ( 'NONE', #17365, #48617, #32777 ) ;
#5405 = ORIENTED_EDGE ( 'NONE', *, *, #48093, .F. ) ;
#5406 = CARTESIAN_POINT ( 'NONE',  ( -14.99999999999845812, 16.00000000000000000, 60.00000000000000000 ) ) ;
#5407 = ORIENTED_EDGE ( 'NONE', *, *, #2180, .F. ) ;
#5408 = DIRECTION ( 'NONE',  ( -0.000000000000000000, -1.000000000000000000, -0.000000000000000000 ) ) ;
#5409 = AXIS2_PLACEMENT_3D ( 'NONE', #28302, #43193, #36275 ) ;
#5410 = VERTEX_POINT ( 'NONE', #2978 ) ;
#5411 = DIRECTION ( 'NONE',  ( -1.000000000000000000, -0.000000000000000000, -0.000000000000000000 ) ) ;
#5412 = FACE_OUTER_BOUND ( 'NONE', #25586, .T. ) ;
#5413 = ADVANCED_FACE ( 'NONE', ( #30185 ), #41992, .F. ) ;
#5414 = CARTESIAN_POINT ( 'NONE',  ( -325.0507910275983932, 325.0507910275983932, 321.8002831173224649 ) ) ;
#5415 = ORIENTED_EDGE ( 'NONE', *, *, #10741, .T. ) ;
#5416 = VECTOR ( 'NONE', #26952, 1000.000000000000000 ) ;
#5417 = EDGE_CURVE ( 'NONE', #40834, #34025, #18627, .T. ) ;
#5418 = CARTESIAN_POINT ( 'NONE',  ( -119.9999999999990905, 17.00000000000000000, -24.99999999999999289 ) ) ;
#5419 = VERTEX_POINT ( 'NONE', #3479 ) ;
#5420 = LINE ( 'NONE', #9770, #30303 ) ;
#5421 = CARTESIAN_POINT ( 'NONE',  ( 0.7604583772899720095, -1.297021979204312725, 9.944962737616615200 ) ) ;
#5422 =( BOUNDED_CURVE ( )  B_SPLINE_CURVE ( 3, ( #30650, #49079, #41429, #45742 ),
 .UNSPECIFIED., .F., .F. ) 
 B_SPLINE_CURVE_WITH_KNOTS ( ( 4, 4 ),
 ( 4.712388980384689674, 6.283185307179586232 ),
 .UNSPECIFIED. ) 
 CURVE ( )  GEOMETRIC_REPRESENTATION_ITEM ( )  RATIONAL_B_SPLINE_CURVE ( ( 1.000000000000000000, 0.8047378541243649375, 0.8047378541243649375, 1.000000000000000000 ) ) 
 REPRESENTATION_ITEM ( '' )  );
#5423 = DIRECTION ( 'NONE',  ( -0.000000000000000000, -0.000000000000000000, -1.000000000000000000 ) ) ;
#5424 = CARTESIAN_POINT ( 'NONE',  ( -167.4999999999999432, -102.5000000000000142, -8.575805527524005711 ) ) ;
#5425 = CARTESIAN_POINT ( 'NONE',  ( 30.12518629743562926, 14.70074613238908157, 1.847720168420772691 ) ) ;
#5426 = VERTEX_POINT ( 'NONE', #29943 ) ;
#5427 = ORIENTED_EDGE ( 'NONE', *, *, #7999, .F. ) ;
#5428 = DIRECTION ( 'NONE',  ( 0.000000000000000000, 7.004339610132985974E-48, 1.000000000000000000 ) ) ;
#5429 = VECTOR ( 'NONE', #4247, 1000.000000000000000 ) ;
#5430 = ORIENTED_EDGE ( 'NONE', *, *, #35263, .T. ) ;
#5431 = VECTOR ( 'NONE', #42152, 1000.000000000000000 ) ;
#5432 = DIRECTION ( 'NONE',  ( -0.000000000000000000, -1.000000000000000000, -0.000000000000000000 ) ) ;
#5433 = PLANE ( 'NONE',  #14146 ) ;
#5434 = ORIENTED_EDGE ( 'NONE', *, *, #16175, .T. ) ;
#5435 = FACE_OUTER_BOUND ( 'NONE', #31932, .T. ) ;
#5436 = CARTESIAN_POINT ( 'NONE',  ( -5.000000000000000000, 0.000000000000000000, 0.000000000000000000 ) ) ;
#5437 = VERTEX_POINT ( 'NONE', #21985 ) ;
#5438 = DIRECTION ( 'NONE',  ( 0.000000000000000000, 0.000000000000000000, -1.000000000000000000 ) ) ;
#5440 = CIRCLE ( 'NONE', #12012, 1.750000000000001554 ) ;
#5439 = DIRECTION ( 'NONE',  ( -0.000000000000000000, -0.000000000000000000, -1.000000000000000000 ) ) ;
#5441 = ADVANCED_FACE ( 'NONE', ( #26600, #10437, #22490, #10940, #18130, #19136 ), #38165, .F. ) ;
#5442 = ORIENTED_EDGE ( 'NONE', *, *, #29353, .T. ) ;
#5443 = EDGE_CURVE ( 'NONE', #31445, #37995, #45558, .T. ) ;
#5444 = ORIENTED_EDGE ( 'NONE', *, *, #37795, .F. ) ;
#5445 = VECTOR ( 'NONE', #24901, 1000.000000000000000 ) ;
#5446 = ORIENTED_EDGE ( 'NONE', *, *, #18323, .T. ) ;
#5447 = CARTESIAN_POINT ( 'NONE',  ( -167.7210997126620384, -1.750000000000010214, -118.1565861772249519 ) ) ;
#5449 = EDGE_CURVE ( 'NONE', #35427, #5026, #34826, .T. ) ;
#5448 = CARTESIAN_POINT ( 'NONE',  ( 48.34672127938079456, -13.00749071703866555, 3.199614146704519602 ) ) ;
#5450 = DIRECTION ( 'NONE',  ( -1.000000000000000000, 0.000000000000000000, -0.000000000000000000 ) ) ;
#5452 = B_SPLINE_CURVE_WITH_KNOTS ( 'NONE', 3,
 ( #42868, #35726, #19013, #308 ),
 .UNSPECIFIED., .F., .F.,
 ( 4, 4 ),
 ( 0.0004536450142761632299, 0.006592155078637213644 ),
 .UNSPECIFIED. ) ;
#5451 = CARTESIAN_POINT ( 'NONE',  ( -8.277096487746778308, 50.00000000000000711, 7.455576670931136185 ) ) ;
#5453 = ORIENTED_EDGE ( 'NONE', *, *, #4509, .F. ) ;
#5454 = EDGE_CURVE ( 'NONE', #14517, #7888, #6588, .T. ) ;
#5455 = AXIS2_PLACEMENT_3D ( 'NONE', #16608, #12250, #4309 ) ;
#5456 = DIRECTION ( 'NONE',  ( 0.000000000000000000, 0.000000000000000000, 1.000000000000000000 ) ) ;
#5457 = ORIENTED_EDGE ( 'NONE', *, *, #30071, .F. ) ;
#5458 =( NAMED_UNIT ( * ) SI_UNIT ( $, .STERADIAN. ) SOLID_ANGLE_UNIT ( ) );
#5459 = CARTESIAN_POINT ( 'NONE',  ( 7.303894382572782007, -3.196591120352752835, -1.423015351387224570E-15 ) ) ;
#5460 = LINE ( 'NONE', #9807, #33466 ) ;
#5461 = CARTESIAN_POINT ( 'NONE',  ( -164.9999999999981526, 16.00000000000000000, 90.00000000000000000 ) ) ;
#5462 = FACE_OUTER_BOUND ( 'NONE', #38966, .T. ) ;
#5463 = CARTESIAN_POINT ( 'NONE',  ( -46.69597344681494633, -1.750000000000010658, 120.8182875569279702 ) ) ;
#5464 = LINE ( 'NONE', #2373, #5978 ) ;
#5465 = VERTEX_POINT ( 'NONE', #46050 ) ;
#5466 = CARTESIAN_POINT ( 'NONE',  ( 4.204997580903516941, 7.611558401714507482, 229.0000000000000000 ) ) ;
#5467 = FACE_OUTER_BOUND ( 'NONE', #2798, .T. ) ;
#5468 = CARTESIAN_POINT ( 'NONE',  ( -1.104213410210672430, -0.6509177773818179968, 9.976582533991678048 ) ) ;
#5469 = DIRECTION ( 'NONE',  ( 1.000000000000000000, 0.000000000000000000, 0.000000000000000000 ) ) ;
#5470 = ORIENTED_EDGE ( 'NONE', *, *, #2631, .T. ) ;
#5471 = CARTESIAN_POINT ( 'NONE',  ( -4.999999999999948486, -204.9999999999999716, -234.7500000000000000 ) ) ;
#5472 = ORIENTED_EDGE ( 'NONE', *, *, #46969, .F. ) ;
#5473 = CARTESIAN_POINT ( 'NONE',  ( 193.3040265531851105, 1.750000000000009992, 0.8182875569279768335 ) ) ;
#5474 = CARTESIAN_POINT ( 'NONE',  ( 9.174209336589868258, 3.979181203266223488, 9.646707543097347681 ) ) ;
#5475 = ADVANCED_FACE ( 'NONE', ( #3226 ), #34556, .T. ) ;
#5476 = CARTESIAN_POINT ( 'NONE',  ( 341.9999999999999432, -174.9999999999999432, 355.9999999999998295 ) ) ;
#5477 = EDGE_CURVE ( 'NONE', #24521, #41260, #28118, .T. ) ;
#5478 = ORIENTED_EDGE ( 'NONE', *, *, #458, .F. ) ;
#5479 =( BOUNDED_CURVE ( )  B_SPLINE_CURVE ( 3, ( #21753, #10208, #25860, #14550 ),
 .UNSPECIFIED., .F., .F. ) 
 B_SPLINE_CURVE_WITH_KNOTS ( ( 4, 4 ),
 ( 0.000000000000000000, 1.570796326794896558 ),
 .UNSPECIFIED. ) 
 CURVE ( )  GEOMETRIC_REPRESENTATION_ITEM ( )  RATIONAL_B_SPLINE_CURVE ( ( 1.000000000000000000, 0.8047378541243649375, 0.8047378541243649375, 1.000000000000000000 ) ) 
 REPRESENTATION_ITEM ( '' )  );
#5480 = EDGE_CURVE ( 'NONE', #28586, #19058, #43753, .T. ) ;
#5481 = EDGE_CURVE ( 'NONE', #10540, #15922, #15557, .T. ) ;
#5482 = CARTESIAN_POINT ( 'NONE',  ( -0.3370904143228978245, 0.2449105217885259589, 10.00000000000000000 ) ) ;
#5483 = CARTESIAN_POINT ( 'NONE',  ( 9.221081804193270059, 13.81382350053991104, 3.266473740018926541 ) ) ;
#5484 = FACE_OUTER_BOUND ( 'NONE', #40392, .T. ) ;
#5485 = EDGE_CURVE ( 'NONE', #25915, #19067, #8623, .T. ) ;
#5486 = DIRECTION ( 'NONE',  ( -0.000000000000000000, -1.000000000000000000, -0.000000000000000000 ) ) ;
#5487 =( BOUNDED_CURVE ( )  B_SPLINE_CURVE ( 3, ( #19024, #26989, #15198, #46450 ),
 .UNSPECIFIED., .F., .F. ) 
 B_SPLINE_CURVE_WITH_KNOTS ( ( 4, 4 ),
 ( 3.141592653589793116, 4.712388980384689674 ),
 .UNSPECIFIED. ) 
 CURVE ( )  GEOMETRIC_REPRESENTATION_ITEM ( )  RATIONAL_B_SPLINE_CURVE ( ( 1.000000000000000000, 0.8047378541243649375, 0.8047378541243649375, 1.000000000000000000 ) ) 
 REPRESENTATION_ITEM ( '' )  );
#5488 = EDGE_CURVE ( 'NONE', #12229, #25250, #9088, .T. ) ;
#5489 = ORIENTED_EDGE ( 'NONE', *, *, #50415, .T. ) ;
#5490 = ORIENTED_EDGE ( 'NONE', *, *, #45364, .T. ) ;
#5491 = CARTESIAN_POINT ( 'NONE',  ( -5.083187235775261215, -8.611690166631138510, 9.646707543097347681 ) ) ;
#5492 = VECTOR ( 'NONE', #44100, 1000.000000000000000 ) ;
#5493 = CARTESIAN_POINT ( 'NONE',  ( 32.43949840348898306, 7.871562655726499713, -9.367992836599954742 ) ) ;
#5494 = ORIENTED_EDGE ( 'NONE', *, *, #9251, .F. ) ;
#5495 = ORIENTED_EDGE ( 'NONE', *, *, #21814, .F. ) ;
#5496 = CARTESIAN_POINT ( 'NONE',  ( 0.000000000000000000, 17.00000000000000000, 0.000000000000000000 ) ) ;
#5497 = FACE_OUTER_BOUND ( 'NONE', #47328, .T. ) ;
#5498 = CARTESIAN_POINT ( 'NONE',  ( -168.4459734468149747, 1.025126265847089213, 159.0682875569279418 ) ) ;
#5499 = CARTESIAN_POINT ( 'NONE',  ( 33.30402655318503946, 1.750000000000009992, 160.8182875569279702 ) ) ;
#5500 = ORIENTED_EDGE ( 'NONE', *, *, #25818, .F. ) ;
#5501 = ORIENTED_EDGE ( 'NONE', *, *, #36731, .F. ) ;
#5502 = ORIENTED_EDGE ( 'NONE', *, *, #31003, .F. ) ;
#5503 =( BOUNDED_CURVE ( )  B_SPLINE_CURVE ( 3, ( #29115, #37087, #41154, #14199 ),
 .UNSPECIFIED., .F., .F. ) 
 B_SPLINE_CURVE_WITH_KNOTS ( ( 4, 4 ),
 ( 0.000000000000000000, 1.570796326794896558 ),
 .UNSPECIFIED. ) 
 CURVE ( )  GEOMETRIC_REPRESENTATION_ITEM ( )  RATIONAL_B_SPLINE_CURVE ( ( 1.000000000000000000, 0.8047378541243649375, 0.8047378541243649375, 1.000000000000000000 ) ) 
 REPRESENTATION_ITEM ( '' )  );
#5504 = EDGE_CURVE ( 'NONE', #960, #14675, #33665, .T. ) ;
#5505 = CARTESIAN_POINT ( 'NONE',  ( -14.49999999999999822, 12.98684210526315930, 19.37312575500900280 ) ) ;
#5506 = PLANE ( 'NONE',  #6884 ) ;
#5507 = EDGE_CURVE ( 'NONE', #2601, #43558, #3750, .T. ) ;
#5508 = VECTOR ( 'NONE', #28679, 1000.000000000000000 ) ;
#5509 = EDGE_CURVE ( 'NONE', #34922, #35337, #4514, .T. ) ;
#5510 = ORIENTED_EDGE ( 'NONE', *, *, #12538, .T. ) ;
#5511 = VERTEX_POINT ( 'NONE', #19901 ) ;
#5512 = CARTESIAN_POINT ( 'NONE',  ( 356.0000000000000000, 165.0000000000000000, -340.0000000000001137 ) ) ;
#5513 = CYLINDRICAL_SURFACE ( 'NONE', #28990, 1.750000000000015543 ) ;
#5514 = ORIENTED_EDGE ( 'NONE', *, *, #10198, .F. ) ;
#5515 = EDGE_LOOP ( 'NONE', ( #33670, #14415, #34675, #18540 ) ) ;
#5516 = CARTESIAN_POINT ( 'NONE',  ( 33.64889274059390090, -3.704246042440748621, 8.356839323120299312 ) ) ;
#5517 = CARTESIAN_POINT ( 'NONE',  ( 210.0000000000000568, 0.000000000000000000, -37.43171244307202272 ) ) ;
#5518 = ORIENTED_EDGE ( 'NONE', *, *, #49972, .T. ) ;
#5519 = CARTESIAN_POINT ( 'NONE',  ( 152.2789002873379900, -1.750000000000010214, 121.8434138227750623 ) ) ;
#5520 = DIRECTION ( 'NONE',  ( 0.000000000000000000, 1.000000000000000000, 6.123233995736766036E-17 ) ) ;
#5521 = CARTESIAN_POINT ( 'NONE',  ( -86.69597344681494633, -1.750000000000009992, -159.1817124430720298 ) ) ;
#5522 = DIRECTION ( 'NONE',  ( 1.000000000000000000, 0.000000000000000000, 0.000000000000000000 ) ) ;
#5523 = CARTESIAN_POINT ( 'NONE',  ( -206.6959734468149463, 0.000000000000000000, 165.0000000000000000 ) ) ;
#5524 = VERTEX_POINT ( 'NONE', #11704 ) ;
#5525 = EDGE_CURVE ( 'NONE', #33474, #21965, #27625, .T. ) ;
#5526 = CARTESIAN_POINT ( 'NONE',  ( -16.69947034530963847, 2.312583065866374632, 2.590526750877053086 ) ) ;
#5527 = CARTESIAN_POINT ( 'NONE',  ( 2.052581215100350853, -0.2042358160480859663, 9.886433018048069954 ) ) ;
#5528 = DIRECTION ( 'NONE',  ( 0.000000000000000000, -1.224646799147352961E-16, 1.000000000000000000 ) ) ;
#5529 = DIRECTION ( 'NONE',  ( -0.000000000000000000, -0.000000000000000000, -1.000000000000000000 ) ) ;
#5530 = DIRECTION ( 'NONE',  ( 6.938893903907223447E-16, 0.000000000000000000, 1.000000000000000000 ) ) ;
#5531 = B_SPLINE_CURVE_WITH_KNOTS ( 'NONE', 3,
 ( #24050, #20184, #9140, #686 ),
 .UNSPECIFIED., .F., .F.,
 ( 4, 4 ),
 ( 0.0006669682284780770491, 0.0007799402130932136645 ),
 .UNSPECIFIED. ) ;
#5532 = MANIFOLD_SOLID_BREP ( 'Cut-Extrude1', #3153 ) ;
#5533 = EDGE_CURVE ( 'NONE', #43883, #43789, #47322, .T. ) ;
#5534 = DIRECTION ( 'NONE',  ( 3.172065745548403743E-16, 1.000000000000000000, 0.000000000000000000 ) ) ;
#5535 = CYLINDRICAL_SURFACE ( 'NONE', #1595, 1.750000000000015543 ) ;
#5536 = ORIENTED_EDGE ( 'NONE', *, *, #35030, .T. ) ;
#5537 = CARTESIAN_POINT ( 'NONE',  ( 25.40454589245968364, 27.58367357691700406, -8.192531242611265085 ) ) ;
#5538 = EDGE_CURVE ( 'NONE', #16170, #28550, #19862, .T. ) ;
#5539 = ADVANCED_FACE ( 'NONE', ( #20156 ), #49336, .T. ) ;
#5540 = AXIS2_PLACEMENT_3D ( 'NONE', #24472, #5212, #47523 ) ;
#5541 = LINE ( 'NONE', #13488, #6562 ) ;
#5542 = FACE_OUTER_BOUND ( 'NONE', #18492, .T. ) ;
#5543 = CARTESIAN_POINT ( 'NONE',  ( 36.08557433729230723, -35.58569447144768105, 7.455576670931136185 ) ) ;
#5544 = CARTESIAN_POINT ( 'NONE',  ( -44.94597344681493922, 2.143131898507880377E-16, -37.43171244307200141 ) ) ;
#5545 = EDGE_CURVE ( 'NONE', #14442, #45963, #40681, .T. ) ;
#5546 = ORIENTED_EDGE ( 'NONE', *, *, #32398, .T. ) ;
#5547 = CARTESIAN_POINT ( 'NONE',  ( 130.0000000000005684, 17.00000000000000000, -30.00000000000000000 ) ) ;
#5548 = EDGE_LOOP ( 'NONE', ( #25671, #32865, #14516, #34864, #2466 ) ) ;
#5549 = CARTESIAN_POINT ( 'NONE',  ( -49.89397392339119364, 8.245536726717011433, 7.906207997025717304 ) ) ;
#5550 = EDGE_CURVE ( 'NONE', #29259, #20258, #29373, .T. ) ;
#5551 = CARTESIAN_POINT ( 'NONE',  ( -168.4459734468149747, -1.025126265847089657, -80.93171244307201562 ) ) ;
#5552 = EDGE_CURVE ( 'NONE', #40604, #15344, #41165, .T. ) ;
#5553 = VERTEX_POINT ( 'NONE', #20920 ) ;
#5554 = CARTESIAN_POINT ( 'NONE',  ( -164.9459734468149463, 2.143131898507880377E-16, -160.9317124430720014 ) ) ;
#5555 = FACE_OUTER_BOUND ( 'NONE', #35797, .T. ) ;
#5556 = VERTEX_POINT ( 'NONE', #32723 ) ;
#5557 = ORIENTED_EDGE ( 'NONE', *, *, #34410, .T. ) ;
#5558 = VECTOR ( 'NONE', #42177, 1000.000000000000000 ) ;
#5559 = EDGE_CURVE ( 'NONE', #15591, #13831, #33489, .T. ) ;
#5560 = CYLINDRICAL_SURFACE ( 'NONE', #36501, 1.750000000000010214 ) ;
#5561 = CARTESIAN_POINT ( 'NONE',  ( 35.51958307830769002, -12.13749199045042282, -6.568693074176326085 ) ) ;
#5562 = DIRECTION ( 'NONE',  ( 0.000000000000000000, -0.2223603367690656640, 0.9749645535258950613 ) ) ;
#5563 = ORIENTED_EDGE ( 'NONE', *, *, #43099, .T. ) ;
#5564 = CARTESIAN_POINT ( 'NONE',  ( 185.0000000000000284, -174.9999999999999716, -99.00000000000014211 ) ) ;
#5565 = DIRECTION ( 'NONE',  ( -0.000000000000000000, -0.000000000000000000, -1.000000000000000000 ) ) ;
#5566 = ORIENTED_EDGE ( 'NONE', *, *, #5552, .F. ) ;
#5567 = ORIENTED_EDGE ( 'NONE', *, *, #23054, .T. ) ;
#5568 = EDGE_LOOP ( 'NONE', ( #49170, #12060, #17176 ) ) ;
#5569 = DIRECTION ( 'NONE',  ( 0.000000000000000000, 1.000000000000000000, 0.000000000000000000 ) ) ;
#5570 = CARTESIAN_POINT ( 'NONE',  ( 192.2789002873380184, 1.750000000000010436, -80.20683870891910772 ) ) ;
#5571 = VERTEX_POINT ( 'NONE', #9121 ) ;
#5572 = CARTESIAN_POINT ( 'NONE',  ( 34.32915281903212446, 1.750000000000010214, -78.15658617722490931 ) ) ;
#5573 = CARTESIAN_POINT ( 'NONE',  ( -0.3334286742303091411, -1.332255019526853435, 9.946805383069623474 ) ) ;
#5574 = PLANE ( 'NONE',  #1424 ) ;
#5575 = CARTESIAN_POINT ( 'NONE',  ( 34.99999999999997868, 17.00000000000000000, -114.9999999999999858 ) ) ;
#5576 = VECTOR ( 'NONE', #2369, 1000.000000000000000 ) ;
#5577 = CARTESIAN_POINT ( 'NONE',  ( -205.6708471809678827, 1.750000000000009548, 41.84341382277508359 ) ) ;
#5578 = CARTESIAN_POINT ( 'NONE',  ( -47.72109971266203132, -1.750000000000009548, 161.8434138227750907 ) ) ;
#5579 = CARTESIAN_POINT ( 'NONE',  ( -88.44597344681497475, 0.000000000000000000, -117.4317124430720156 ) ) ;
#5580 = CARTESIAN_POINT ( 'NONE',  ( 1.011271242968683648, 0.7347315653655930312, 9.972675548442463622 ) ) ;
#5581 = CARTESIAN_POINT ( 'NONE',  ( 16.73672383626881199, 2.341008440548111302, -9.008049429158100807 ) ) ;
#5582 = EDGE_CURVE ( 'NONE', #20412, #14675, #30074, .T. ) ;
#5583 = CARTESIAN_POINT ( 'NONE',  ( -114.9999999999981526, 17.00000000000000000, 65.00000000000000000 ) ) ;
#5584 = DIRECTION ( 'NONE',  ( 1.000000000000000000, 0.000000000000000000, 0.000000000000000000 ) ) ;
#5585 = VERTEX_POINT ( 'NONE', #9368 ) ;
#5586 = FACE_OUTER_BOUND ( 'NONE', #11858, .T. ) ;
#5587 = DIRECTION ( 'NONE',  ( 1.000000000000000000, 0.000000000000000000, 0.000000000000000000 ) ) ;
#5588 = FACE_OUTER_BOUND ( 'NONE', #2162, .T. ) ;
#5589 = CARTESIAN_POINT ( 'NONE',  ( 155.0540265531850537, 2.143131898507880377E-16, -80.93171244307201562 ) ) ;
#5590 = VERTEX_POINT ( 'NONE', #17317 ) ;
#5591 = CARTESIAN_POINT ( 'NONE',  ( 33.30402655318503946, 1.750000000000010658, -79.18171244307201562 ) ) ;
#5592 = ADVANCED_FACE ( 'NONE', ( #13466 ), #37099, .T. ) ;
#5593 = ADVANCED_FACE ( 'NONE', ( #36603 ), #9623, .T. ) ;
#5594 = CARTESIAN_POINT ( 'NONE',  ( -1.468446590252919348, -0.3226319952343834063, 9.953784399990620813 ) ) ;
#5595 = ORIENTED_EDGE ( 'NONE', *, *, #15505, .T. ) ;
#5596 = CARTESIAN_POINT ( 'NONE',  ( -22.75063655912460447, -24.61040335498469389, -8.466730184410787174 ) ) ;
#5597 = CYLINDRICAL_SURFACE ( 'NONE', #11020, 1.749999999999973799 ) ;
#5598 = DIRECTION ( 'NONE',  ( 0.000000000000000000, 0.000000000000000000, 1.000000000000000000 ) ) ;
#5599 = EDGE_CURVE ( 'NONE', #31636, #25458, #33247, .T. ) ;
#5600 = ORIENTED_EDGE ( 'NONE', *, *, #7631, .T. ) ;
#5601 = SURFACE_STYLE_FILL_AREA ( #25120 ) ;
#5602 = ORIENTED_EDGE ( 'NONE', *, *, #22353, .F. ) ;
#5603 = ORIENTED_EDGE ( 'NONE', *, *, #31809, .F. ) ;
#5604 = ADVANCED_FACE ( 'NONE', ( #44989 ), #49076, .T. ) ;
#5605 = DIRECTION ( 'NONE',  ( -0.000000000000000000, -1.000000000000000000, -0.000000000000000000 ) ) ;
#5606 = EDGE_CURVE ( 'NONE', #32346, #49488, #6014, .T. ) ;
#5607 = AXIS2_PLACEMENT_3D ( 'NONE', #5782, #45751, #6539 ) ;
#5608 = ORIENTED_EDGE ( 'NONE', *, *, #18881, .F. ) ;
#5609 = CARTESIAN_POINT ( 'NONE',  ( 135.0000000000019043, 17.00000000000000000, 90.00000000000000000 ) ) ;
#5610 = MANIFOLD_SOLID_BREP ( 'Cut-Extrude1[4]', #1534 ) ;
#5611 = ORIENTED_EDGE ( 'NONE', *, *, #25632, .F. ) ;
#5612 = DIRECTION ( 'NONE',  ( -1.000000000000000000, 0.000000000000000000, 0.000000000000000000 ) ) ;
#5613 = DIRECTION ( 'NONE',  ( 0.000000000000000000, -2.265761274745217480E-16, 1.000000000000000000 ) ) ;
#5614 = EDGE_CURVE ( 'NONE', #2521, #44090, #20663, .T. ) ;
#5615 = DIRECTION ( 'NONE',  ( -1.000000000000000000, 0.000000000000000000, 0.000000000000000000 ) ) ;
#5616 = DIRECTION ( 'NONE',  ( 1.000000000000000000, 0.000000000000000000, -0.000000000000000000 ) ) ;
#5617 = VECTOR ( 'NONE', #11838, 1000.000000000000000 ) ;
#5618 = EDGE_LOOP ( 'NONE', ( #27292, #2178, #12293, #31627 ) ) ;
#5619 = FACE_OUTER_BOUND ( 'NONE', #10615, .T. ) ;
#5620 = ORIENTED_EDGE ( 'NONE', *, *, #45836, .F. ) ;
#5621 = DIRECTION ( 'NONE',  ( 0.7233555441435720601, 0.6904757466825006684, -0.000000000000000000 ) ) ;
#5622 = PLANE ( 'NONE',  #46600 ) ;
#5623 = EDGE_LOOP ( 'NONE', ( #19375, #43841, #13617, #30615 ) ) ;
#5624 = EDGE_LOOP ( 'NONE', ( #47004, #28637, #40172 ) ) ;
#5625 = ORIENTED_EDGE ( 'NONE', *, *, #24370, .T. ) ;
#5626 = LINE ( 'NONE', #4864, #13876 ) ;
#5627 = CARTESIAN_POINT ( 'NONE',  ( -48.44597344681495343, 0.000000000000000000, 39.06828755692798438 ) ) ;
#5628 = B_SPLINE_SURFACE_WITH_KNOTS ( 'NONE', 3, 3, ( 
 ( #30951, #7850, #31196, #50632 ),
 ( #39654, #43483, #400, #7327 ),
 ( #46784, #8354, #19378, #23495 ),
 ( #19630, #42968, #42461, #47302 ) ),
 .UNSPECIFIED., .F., .F., .F.,
 ( 4, 4 ),
 ( 4, 4 ),
 ( 0.000000000000000000, 1.000000000000000000 ),
 ( 0.000000000000000000, 1.000000000000000000 ),
 .UNSPECIFIED. ) ;
#5629 = VERTEX_POINT ( 'NONE', #2672 ) ;
#5630 = DIRECTION ( 'NONE',  ( -0.000000000000000000, -0.000000000000000000, -1.000000000000000000 ) ) ;
#5631 = CARTESIAN_POINT ( 'NONE',  ( -84.94597344681493212, -1.025126265847089657, 79.06828755692797017 ) ) ;
#5632 = CARTESIAN_POINT ( 'NONE',  ( -207.7210997126620384, -1.750000000000009548, -158.1565861772249377 ) ) ;
#5633 = ORIENTED_EDGE ( 'NONE', *, *, #24333, .T. ) ;
#5634 = LINE ( 'NONE', #45369, #34347 ) ;
#5635 = DIRECTION ( 'NONE',  ( -0.000000000000000000, -1.000000000000000000, -0.000000000000000000 ) ) ;
#5636 = ADVANCED_FACE ( 'NONE', ( #38098 ), #6780, .F. ) ;
#5637 =( BOUNDED_CURVE ( )  B_SPLINE_CURVE ( 3, ( #10303, #29296, #16991, #48986 ),
 .UNSPECIFIED., .F., .F. ) 
 B_SPLINE_CURVE_WITH_KNOTS ( ( 4, 4 ),
 ( 3.141592653589793116, 4.712388980384689674 ),
 .UNSPECIFIED. ) 
 CURVE ( )  GEOMETRIC_REPRESENTATION_ITEM ( )  RATIONAL_B_SPLINE_CURVE ( ( 1.000000000000000000, 0.8047378541243649375, 0.8047378541243649375, 1.000000000000000000 ) ) 
 REPRESENTATION_ITEM ( '' )  );
#5638 = CARTESIAN_POINT ( 'NONE',  ( -0.5107275442771143092, -1.175643901748072873, 9.976582533991681601 ) ) ;
#5639 = VERTEX_POINT ( 'NONE', #33743 ) ;
#5640 = EDGE_CURVE ( 'NONE', #49297, #5007, #37852, .T. ) ;
#5641 = EDGE_LOOP ( 'NONE', ( #47808, #1671, #8547, #43786 ) ) ;
#5642 = SHAPE_DEFINITION_REPRESENTATION ( #41711, #3157 ) ;
#5643 = VECTOR ( 'NONE', #7613, 1000.000000000000000 ) ;
#5644 = DIRECTION ( 'NONE',  ( 0.000000000000000000, 0.000000000000000000, -1.000000000000000000 ) ) ;
#5645 = CARTESIAN_POINT ( 'NONE',  ( -239.0000000000000853, -153.6999999999999602, 250.3600000000000136 ) ) ;
#5646 = VECTOR ( 'NONE', #746, 1000.000000000000000 ) ;
#5647 = CARTESIAN_POINT ( 'NONE',  ( -27.33593271309441519, 41.94268121623345991, -9.367992836599954742 ) ) ;
#5648 = CARTESIAN_POINT ( 'NONE',  ( 342.0000000000000568, 181.0000000000000568, 355.9999999999998295 ) ) ;
#5649 = ORIENTED_EDGE ( 'NONE', *, *, #41016, .T. ) ;
#5650 = AXIS2_PLACEMENT_3D ( 'NONE', #24908, #17209, #39812 ) ;
#5651 = CIRCLE ( 'NONE', #37653, 0.4999999999999997224 ) ;
#5652 = FACE_OUTER_BOUND ( 'NONE', #23410, .T. ) ;
#5653 = DIRECTION ( 'NONE',  ( 0.5038710255240859137, 0.000000000000000000, -0.8637789008984335659 ) ) ;
#5654 = DIRECTION ( 'NONE',  ( -1.000000000000000000, 0.000000000000000000, 0.000000000000000000 ) ) ;
#5655 = DIRECTION ( 'NONE',  ( -8.673617379884028076E-17, 1.000000000000000000, 0.000000000000000000 ) ) ;
#5656 = VECTOR ( 'NONE', #47947, 1000.000000000000000 ) ;
#5657 = CARTESIAN_POINT ( 'NONE',  ( 210.0000000000000568, 0.000000000000000000, -119.1817124430720440 ) ) ;
#5658 = VECTOR ( 'NONE', #45006, 1000.000000000000114 ) ;
#5659 = ORIENTED_EDGE ( 'NONE', *, *, #5854, .T. ) ;
#5660 = CARTESIAN_POINT ( 'NONE',  ( -0.09523839817533703844, -1.466467394240187350, 9.958264684458541183 ) ) ;
#5661 = ORIENTED_EDGE ( 'NONE', *, *, #2704, .T. ) ;
#5662 = CARTESIAN_POINT ( 'NONE',  ( -14.49999999999999822, -46.01315789473684248, -5.916985404131818171 ) ) ;
#5663 =( REPRESENTATION_RELATIONSHIP ('NONE','NONE', #45699, #3157 ) REPRESENTATION_RELATIONSHIP_WITH_TRANSFORMATION ( #49209 )SHAPE_REPRESENTATION_RELATIONSHIP( ) );
#5664 = EDGE_LOOP ( 'NONE', ( #283, #37998, #29739, #28090, #37122, #49497 ) ) ;
#5665 = LINE ( 'NONE', #36752, #3293 ) ;
#5666 = CARTESIAN_POINT ( 'NONE',  ( -207.7210997126620384, -1.750000000000009548, -160.2068387089191219 ) ) ;
#5667 = CARTESIAN_POINT ( 'NONE',  ( -119.9999999999987921, 17.00000000000000000, 5.000000000000004441 ) ) ;
#5668 = ORIENTED_EDGE ( 'NONE', *, *, #31852, .F. ) ;
#5669 = LINE ( 'NONE', #16479, #25336 ) ;
#5670 = ORIENTED_EDGE ( 'NONE', *, *, #27288, .T. ) ;
#5671 = CARTESIAN_POINT ( 'NONE',  ( 30.00000000000092726, 17.00000000000000000, 0.000000000000000000 ) ) ;
#5672 = CARTESIAN_POINT ( 'NONE',  ( 2.769912820522884456, -9.621098677754085671, 6.185594734181534271 ) ) ;
#5673 = DIRECTION ( 'NONE',  ( -0.000000000000000000, -0.000000000000000000, 1.000000000000000000 ) ) ;
#5674 = DIRECTION ( 'NONE',  ( 7.793956916774525800E-48, 0.000000000000000000, 1.000000000000000000 ) ) ;
#5675 = EDGE_CURVE ( 'NONE', #37518, #33796, #18310, .T. ) ;
#5676 = CARTESIAN_POINT ( 'NONE',  ( 46.10908423965007330, 19.89422939639137766, 1.847720168420772691 ) ) ;
#5677 = ORIENTED_EDGE ( 'NONE', *, *, #49840, .F. ) ;
#5678 = ORIENTED_EDGE ( 'NONE', *, *, #34132, .T. ) ;
#5679 = LINE ( 'NONE', #6690, #27598 ) ;
#5680 = AXIS2_PLACEMENT_3D ( 'NONE', #28889, #44507, #42883 ) ;
#5681 = AXIS2_PLACEMENT_3D ( 'NONE', #34207, #37561, #30098 ) ;
#5682 = ORIENTED_EDGE ( 'NONE', *, *, #8710, .F. ) ;
#5683 = CARTESIAN_POINT ( 'NONE',  ( -126.6959734468149321, -1.749999999999997335, -79.18171244307201562 ) ) ;
#5684 = CARTESIAN_POINT ( 'NONE',  ( 32.27890028733795447, 1.750000000000009326, -158.1565861772249377 ) ) ;
#5685 = EDGE_LOOP ( 'NONE', ( #1427, #28695, #32580, #5124, #31405, #18798 ) ) ;
#5686 = DIRECTION ( 'NONE',  ( -1.000000000000000000, -0.000000000000000000, -0.000000000000000000 ) ) ;
#5687 = AXIS2_PLACEMENT_3D ( 'NONE', #12505, #39729, #32029 ) ;
#5688 = VECTOR ( 'NONE', #36681, 1000.000000000000000 ) ;
#5689 = DIRECTION ( 'NONE',  ( 0.000000000000000000, 0.000000000000000000, 1.000000000000000000 ) ) ;
#5690 = ORIENTED_EDGE ( 'NONE', *, *, #45622, .F. ) ;
#5691 = CARTESIAN_POINT ( 'NONE',  ( 1.231029138816503110, 0.08486683738666057908, 9.969907237807635880 ) ) ;
#5692 = FACE_OUTER_BOUND ( 'NONE', #17024, .T. ) ;
#5693 = CARTESIAN_POINT ( 'NONE',  ( 0.000000000000000000, -180.9999999999999716, -344.0000000000001705 ) ) ;
#5694 = AXIS2_PLACEMENT_3D ( 'NONE', #42204, #6045, #30413 ) ;
#5695 = DIRECTION ( 'NONE',  ( 0.000000000000000000, 0.000000000000000000, 1.000000000000000000 ) ) ;
#5696 = ORIENTED_EDGE ( 'NONE', *, *, #25363, .F. ) ;
#5697 = EDGE_LOOP ( 'NONE', ( #6929, #6365, #37231, #15190 ) ) ;
#5698 = MANIFOLD_SOLID_BREP ( 'Boss-Extrude2', #36785 ) ;
#5699 = CARTESIAN_POINT ( 'NONE',  ( -85.67084718096784002, 1.750000000000010214, 81.84341382277507648 ) ) ;
#5700 = CARTESIAN_POINT ( 'NONE',  ( -4.135284104686786393E-15, 0.4183134307191331280, 9.992713367193012175 ) ) ;
#5701 = PLANE ( 'NONE',  #34925 ) ;
#5702 = DIRECTION ( 'NONE',  ( 4.996003610813203446E-16, 1.000000000000000000, 0.000000000000000000 ) ) ;
#5703 = CARTESIAN_POINT ( 'NONE',  ( 2.538055338523177440, 50.00000000000000711, -9.367992836599954742 ) ) ;
#5704 = ORIENTED_EDGE ( 'NONE', *, *, #13082, .T. ) ;
#5705 = CARTESIAN_POINT ( 'NONE',  ( 34.99999999999997868, 17.00000000000000000, -114.9999999999999858 ) ) ;
#5706 = VERTEX_POINT ( 'NONE', #14212 ) ;
#5707 = CARTESIAN_POINT ( 'NONE',  ( -5.000000000000000000, 184.8000000000000114, 359.7999999999997840 ) ) ;
#5708 = CARTESIAN_POINT ( 'NONE',  ( -164.9999999999981526, 16.00000000000000000, 65.00000000000000000 ) ) ;
#5709 = CARTESIAN_POINT ( 'NONE',  ( 168.9999999999999716, -180.9999999999999716, -340.0000000000001137 ) ) ;
#5710 = CARTESIAN_POINT ( 'NONE',  ( -1.377636575563021992, 0.6021164824561227036, 9.953784399990620813 ) ) ;
#5711 = CARTESIAN_POINT ( 'NONE',  ( 210.0000000000000568, 0.000000000000000000, 120.8182875569279702 ) ) ;
#5712 = DIRECTION ( 'NONE',  ( -1.000000000000000000, -0.000000000000000000, -0.000000000000000000 ) ) ;
#5713 = ORIENTED_EDGE ( 'NONE', *, *, #47402, .T. ) ;
#5714 = PLANE ( 'NONE',  #2595 ) ;
#5715 = CARTESIAN_POINT ( 'NONE',  ( -207.2473046169136808, -153.9383703589661252, 472.5992458228021746 ) ) ;
#5716 = DIRECTION ( 'NONE',  ( 0.000000000000000000, 0.000000000000000000, -1.000000000000000000 ) ) ;
#5717 = VECTOR ( 'NONE', #37692, 1000.000000000000000 ) ;
#5718 = AXIS2_PLACEMENT_3D ( 'NONE', #46898, #5349, #28463 ) ;
#5719 = CIRCLE ( 'NONE', #34418, 2.000000000000001776 ) ;
#5720 = CARTESIAN_POINT ( 'NONE',  ( 350.0000000000000000, -174.9999999999999716, -350.0000000000002274 ) ) ;
#5721 = EDGE_LOOP ( 'NONE', ( #18465, #39616, #33856, #13679 ) ) ;
#5722 =( BOUNDED_CURVE ( )  B_SPLINE_CURVE ( 3, ( #27703, #46902, #7704, #19746 ),
 .UNSPECIFIED., .F., .F. ) 
 B_SPLINE_CURVE_WITH_KNOTS ( ( 4, 4 ),
 ( 1.570796326794896558, 3.141592653589793116 ),
 .UNSPECIFIED. ) 
 CURVE ( )  GEOMETRIC_REPRESENTATION_ITEM ( )  RATIONAL_B_SPLINE_CURVE ( ( 1.000000000000000000, 0.8047378541243649375, 0.8047378541243649375, 1.000000000000000000 ) ) 
 REPRESENTATION_ITEM ( '' )  );
#5723 = DIRECTION ( 'NONE',  ( 0.000000000000000000, 0.000000000000000000, -1.000000000000000000 ) ) ;
#5724 = ORIENTED_EDGE ( 'NONE', *, *, #28511, .T. ) ;
#5725 = VECTOR ( 'NONE', #36971, 1000.000000000000000 ) ;
#5726 = LINE ( 'NONE', #44455, #7380 ) ;
#5727 = CARTESIAN_POINT ( 'NONE',  ( 115.0540265531850395, 2.143131898507847836E-16, 122.5682875569279560 ) ) ;
#5728 = CARTESIAN_POINT ( 'NONE',  ( 15.80799809827372648, -29.65358618225706522, -8.016098858316205167 ) ) ;
#5729 = VERTEX_POINT ( 'NONE', #3165 ) ;
#5730 = AXIS2_PLACEMENT_3D ( 'NONE', #36247, #24940, #9282 ) ;
#5731 = CARTESIAN_POINT ( 'NONE',  ( 23.82716369509147825, 44.49195112876006419, 8.356839323120299312 ) ) ;
#5732 = CARTESIAN_POINT ( 'NONE',  ( 370.7621192902014968, -66.40178110878291307, -93.79675437945473959 ) ) ;
#5733 = DIRECTION ( 'NONE',  ( -1.000000000000000000, -0.000000000000000000, -0.000000000000000000 ) ) ;
#5734 = CARTESIAN_POINT ( 'NONE',  ( -8.277096487746778308, 45.55573069994827051, 7.455576670931136185 ) ) ;
#5735 = ADVANCED_FACE ( 'NONE', ( #45497 ), #10385, .T. ) ;
#5736 = EDGE_LOOP ( 'NONE', ( #48782, #6809, #5608, #21655, #28005, #8658 ) ) ;
#5737 = ORIENTED_EDGE ( 'NONE', *, *, #39075, .F. ) ;
#5738 = CARTESIAN_POINT ( 'NONE',  ( -2.538055338523173443, -50.00000000000000711, -9.367992836599951190 ) ) ;
#5739 = ADVANCED_FACE ( 'NONE', ( #43387 ), #320, .T. ) ;
#5740 = PLANE ( 'NONE',  #25497 ) ;
#5741 = ADVANCED_FACE ( 'NONE', ( #47211 ), #8014, .F. ) ;
#5742 = ORIENTED_EDGE ( 'NONE', *, *, #2036, .T. ) ;
#5743 = VERTEX_POINT ( 'NONE', #8774 ) ;
#5744 = PLANE ( 'NONE',  #19042 ) ;
#5745 = DIRECTION ( 'NONE',  ( -0.000000000000000000, -0.000000000000000000, -1.000000000000000000 ) ) ;
#5746 = CARTESIAN_POINT ( 'NONE',  ( -50.00000000000000000, -50.00000000000000000, 800.0000000000000000 ) ) ;
#5747 = VERTEX_POINT ( 'NONE', #1065 ) ;
#5748 = ORIENTED_EDGE ( 'NONE', *, *, #35417, .F. ) ;
#5749 = ORIENTED_EDGE ( 'NONE', *, *, #16083, .F. ) ;
#5750 = EDGE_CURVE ( 'NONE', #37243, #46256, #23903, .T. ) ;
#5751 = VECTOR ( 'NONE', #15847, 1000.000000000000114 ) ;
#5752 = PLANE ( 'NONE',  #39008 ) ;
#5753 = VECTOR ( 'NONE', #29588, 1000.000000000000000 ) ;
#5754 = EDGE_CURVE ( 'NONE', #19349, #21703, #39825, .T. ) ;
#5755 = CARTESIAN_POINT ( 'NONE',  ( 4.999999999999999112, -175.0000000000000284, 350.0000000000002274 ) ) ;
#5756 = AXIS2_PLACEMENT_3D ( 'NONE', #23139, #20060, #27260 ) ;
#5757 = ORIENTED_EDGE ( 'NONE', *, *, #34999, .T. ) ;
#5758 = ORIENTED_EDGE ( 'NONE', *, *, #26959, .T. ) ;
#5759 = AXIS2_PLACEMENT_3D ( 'NONE', #46305, #19648, #27351 ) ;
#5760 = CARTESIAN_POINT ( 'NONE',  ( 35.00000000000061107, 17.00000000000000000, -30.00000000000000000 ) ) ;
#5761 = AXIS2_PLACEMENT_3D ( 'NONE', #39042, #4134, #8494 ) ;
#5762 = CARTESIAN_POINT ( 'NONE',  ( -0.1287570809895658697, 0.3962735484563123523, 10.00000000000000000 ) ) ;
#5763 = VERTEX_POINT ( 'NONE', #43638 ) ;
#5764 = ADVANCED_FACE ( 'NONE', ( #31873 ), #20303, .T. ) ;
#5765 = EDGE_CURVE ( 'NONE', #50249, #43903, #15704, .T. ) ;
#5766 = ORIENTED_EDGE ( 'NONE', *, *, #17761, .T. ) ;
#5767 = CARTESIAN_POINT ( 'NONE',  ( -2.277966102372183776, 9.750758063795943897, 3.092157797347716119 ) ) ;
#5768 = DIRECTION ( 'NONE',  ( -1.000000000000000000, 0.000000000000000000, 0.000000000000000000 ) ) ;
#5769 = VERTEX_POINT ( 'NONE', #31100 ) ;
#5770 = CARTESIAN_POINT ( 'NONE',  ( 153.3040265531850537, 1.750000000000009992, 160.8182875569279702 ) ) ;
#5771 = EDGE_CURVE ( 'NONE', #16293, #6202, #9386, .T. ) ;
#5772 = LINE ( 'NONE', #20665, #4123 ) ;
#5773 = DIRECTION ( 'NONE',  ( 0.000000000000000000, -1.000000000000000000, 0.000000000000000000 ) ) ;
#5774 = CARTESIAN_POINT ( 'NONE',  ( 167.4999999999999716, -102.8976013127941656, -7.208237214241163926 ) ) ;
#5775 = EDGE_CURVE ( 'NONE', #24618, #32124, #12595, .T. ) ;
#5776 = LINE ( 'NONE', #37106, #36448 ) ;
#5777 = VERTEX_POINT ( 'NONE', #28264 ) ;
#5778 = EDGE_CURVE ( 'NONE', #13610, #17677, #30548, .T. ) ;
#5779 = CYLINDRICAL_SURFACE ( 'NONE', #43067, 1.750000000000001554 ) ;
#5780 = ADVANCED_FACE ( 'NONE', ( #20052 ), #19794, .T. ) ;
#5781 = DIRECTION ( 'NONE',  ( 0.000000000000000000, 1.000000000000000000, 0.000000000000000000 ) ) ;
#5782 = CARTESIAN_POINT ( 'NONE',  ( 210.0000000000000568, 0.000000000000000000, 40.81828755692798438 ) ) ;
#5783 = CARTESIAN_POINT ( 'NONE',  ( -6.695973446814940111, -1.750000000000023315, 0.8182875569279768335 ) ) ;
#5784 =( BOUNDED_CURVE ( )  B_SPLINE_CURVE ( 3, ( #35862, #16337, #32005, #47598 ),
 .UNSPECIFIED., .F., .F. ) 
 B_SPLINE_CURVE_WITH_KNOTS ( ( 4, 4 ),
 ( 0.000000000000000000, 1.570796326794896558 ),
 .UNSPECIFIED. ) 
 CURVE ( )  GEOMETRIC_REPRESENTATION_ITEM ( )  RATIONAL_B_SPLINE_CURVE ( ( 1.000000000000000000, 0.8047378541243649375, 0.8047378541243649375, 1.000000000000000000 ) ) 
 REPRESENTATION_ITEM ( '' )  );
#5785 = CARTESIAN_POINT ( 'NONE',  ( -1.437255894074058515, 3.713052624461494755, 6.606856988583542645E-16 ) ) ;
#5786 = CARTESIAN_POINT ( 'NONE',  ( 193.3040265531851105, -1.750000000000010658, -119.1817124430720440 ) ) ;
#5787 = MANIFOLD_SOLID_BREP ( 'Boss-Extrude2', #44141 ) ;
#5788 = CARTESIAN_POINT ( 'NONE',  ( 4.763548243873389154, -16.57409059453848599, 8.727788335465566760 ) ) ;
#5789 = DIRECTION ( 'NONE',  ( 0.000000000000000000, 0.000000000000000000, 1.000000000000000000 ) ) ;
#5790 =( BOUNDED_CURVE ( )  B_SPLINE_CURVE ( 3, ( #31643, #836, #31383, #587 ),
 .UNSPECIFIED., .F., .F. ) 
 B_SPLINE_CURVE_WITH_KNOTS ( ( 4, 4 ),
 ( 3.141592653589793116, 4.712388980384689674 ),
 .UNSPECIFIED. ) 
 CURVE ( )  GEOMETRIC_REPRESENTATION_ITEM ( )  RATIONAL_B_SPLINE_CURVE ( ( 1.000000000000000000, 0.8047378541243649375, 0.8047378541243649375, 1.000000000000000000 ) ) 
 REPRESENTATION_ITEM ( '' )  );
#5791 = EDGE_CURVE ( 'NONE', #3803, #33627, #9506, .T. ) ;
#5792 = CARTESIAN_POINT ( 'NONE',  ( 164.9999999999999716, 16.00000000000000000, 115.0000000000000142 ) ) ;
#5793 = VECTOR ( 'NONE', #49364, 1000.000000000000000 ) ;
#5794 = ORIENTED_EDGE ( 'NONE', *, *, #34974, .T. ) ;
#5795 = CARTESIAN_POINT ( 'NONE',  ( -24.39427009666018265, -44.07992421011638129, 8.807470649214879543 ) ) ;
#5796 = EDGE_CURVE ( 'NONE', #39156, #5803, #31203, .T. ) ;
#5797 = EDGE_CURVE ( 'NONE', #10318, #22771, #25418, .T. ) ;
#5798 = CARTESIAN_POINT ( 'NONE',  ( -568.8466156985925863, 47.50000000000000000, -173.6910835022032700 ) ) ;
#5799 = CARTESIAN_POINT ( 'NONE',  ( -18.38319608353667434, 32.68498281710182596, -8.192531242611268638 ) ) ;
#5800 = CARTESIAN_POINT ( 'NONE',  ( 75.05402655318509630, 2.143131898507880377E-16, -80.93171244307204404 ) ) ;
#5801 = CARTESIAN_POINT ( 'NONE',  ( 344.0000000000000000, 183.0000000000000284, 357.9999999999998863 ) ) ;
#5802 = B_SPLINE_CURVE_WITH_KNOTS ( 'NONE', 3,
 ( #3353, #14404, #10547, #49510 ),
 .UNSPECIFIED., .F., .F.,
 ( 4, 4 ),
 ( 2.954445946614352819E-17, 0.0004072981213157676555 ),
 .UNSPECIFIED. ) ;
#5803 = VERTEX_POINT ( 'NONE', #41319 ) ;
#5804 = CARTESIAN_POINT ( 'NONE',  ( -207.7210997126620384, -1.750000000000009548, 1.843413822775065825 ) ) ;
#5805 = ORIENTED_EDGE ( 'NONE', *, *, #47503, .T. ) ;
#5806 = DIRECTION ( 'NONE',  ( 0.000000000000000000, -2.265761274745217480E-16, 1.000000000000000000 ) ) ;
#5807 = EDGE_CURVE ( 'NONE', #15843, #17906, #45660, .T. ) ;
#5808 = LINE ( 'NONE', #22463, #34488 ) ;
#5809 = VERTEX_POINT ( 'NONE', #29015 ) ;
#5810 = DIRECTION ( 'NONE',  ( -1.000000000000000000, -0.000000000000000000, -0.000000000000000000 ) ) ;
#5811 = CARTESIAN_POINT ( 'NONE',  ( -239.0000000000000853, -165.6999999999999602, 250.3600000000000136 ) ) ;
#5812 = ORIENTED_EDGE ( 'NONE', *, *, #21954, .T. ) ;
#5813 = ORIENTED_EDGE ( 'NONE', *, *, #3987, .T. ) ;
#5814 = EDGE_CURVE ( 'NONE', #3446, #692, #48217, .T. ) ;
#5815 = LINE ( 'NONE', #14261, #14347 ) ;
#5816 = LINE ( 'NONE', #37147, #10321 ) ;
#5817 = CARTESIAN_POINT ( 'NONE',  ( 7.359817328027030925, 15.16751262232805431, 2.590526750877053086 ) ) ;
#5818 = ORIENTED_EDGE ( 'NONE', *, *, #7121, .F. ) ;
#5819 = CARTESIAN_POINT ( 'NONE',  ( -86.69597344681496054, 0.000000000000000000, 165.0000000000000000 ) ) ;
#5820 = CARTESIAN_POINT ( 'NONE',  ( -64.99999999999783995, 17.00000000000000000, 95.00000000000000000 ) ) ;
#5821 = CARTESIAN_POINT ( 'NONE',  ( -86.69597344681494633, -1.750000000000010658, -79.18171244307201562 ) ) ;
#5822 = ORIENTED_EDGE ( 'NONE', *, *, #29641, .F. ) ;
#5823 = EDGE_CURVE ( 'NONE', #47489, #24452, #41065, .T. ) ;
#5824 = VERTEX_POINT ( 'NONE', #13102 ) ;
#5825 = ORIENTED_EDGE ( 'NONE', *, *, #25519, .T. ) ;
#5826 = FACE_OUTER_BOUND ( 'NONE', #30998, .T. ) ;
#5827 = CARTESIAN_POINT ( 'NONE',  ( 191.5540265531851105, 0.000000000000000000, -80.93171244307201562 ) ) ;
#5828 = ORIENTED_EDGE ( 'NONE', *, *, #45645, .T. ) ;
#5829 = AXIS2_PLACEMENT_3D ( 'NONE', #17507, #36020, #17258 ) ;
#5830 = DIRECTION ( 'NONE',  ( 0.000000000000000000, 1.000000000000000000, 0.000000000000000000 ) ) ;
#5831 = CARTESIAN_POINT ( 'NONE',  ( -6.695973446814940111, 1.750000000000024203, -119.1817124430720440 ) ) ;
#5832 = ADVANCED_FACE ( 'NONE', ( #5403 ), #9757, .F. ) ;
#5833 = CARTESIAN_POINT ( 'NONE',  ( 210.0000000000000568, 0.000000000000000000, 0.8182875569279768335 ) ) ;
#5834 = CARTESIAN_POINT ( 'NONE',  ( 73.30402655318508209, 1.750000000000010214, 40.81828755692798438 ) ) ;
#5835 = EDGE_CURVE ( 'NONE', #48110, #16730, #32858, .T. ) ;
#5836 = CARTESIAN_POINT ( 'NONE',  ( 164.9999999999999716, 17.00000000000000000, 34.99999999999999289 ) ) ;
#5837 = DIRECTION ( 'NONE',  ( -1.000000000000000000, -0.000000000000000000, -0.000000000000000000 ) ) ;
#5838 = EDGE_CURVE ( 'NONE', #19943, #41219, #1570, .T. ) ;
#5839 = VECTOR ( 'NONE', #49149, 1000.000000000000000 ) ;
#5840 = CARTESIAN_POINT ( 'NONE',  ( -7.372990760266265653, 0.000000000000000000, 0.000000000000000000 ) ) ;
#5841 = ADVANCED_FACE ( 'NONE', ( #17463 ), #29266, .T. ) ;
#5842 = PLANE ( 'NONE',  #26439 ) ;
#5843 = VECTOR ( 'NONE', #30463, 1000.000000000000000 ) ;
#5844 = CARTESIAN_POINT ( 'NONE',  ( -8.277096487746778308, 50.00000000000000000, 7.455576670931136185 ) ) ;
#5845 = EDGE_CURVE ( 'NONE', #21498, #50507, #9077, .T. ) ;
#5846 = CARTESIAN_POINT ( 'NONE',  ( -208.4459734468149463, 0.000000000000000000, 122.5682875569279702 ) ) ;
#5847 = LINE ( 'NONE', #21488, #42915 ) ;
#5848 = EDGE_LOOP ( 'NONE', ( #16107, #30418, #1318, #15537 ) ) ;
#5849 = CARTESIAN_POINT ( 'NONE',  ( -128.4459734468149179, 0.000000000000000000, -37.43171244307205825 ) ) ;
#5850 = CARTESIAN_POINT ( 'NONE',  ( -0.1287570809895632329, 0.3962735484563137400, 10.00000000000000000 ) ) ;
#5851 = CARTESIAN_POINT ( 'NONE',  ( 210.0000000000000568, 0.000000000000000000, -159.1817124430720298 ) ) ;
#5852 = ORIENTED_EDGE ( 'NONE', *, *, #3020, .T. ) ;
#5853 = FACE_OUTER_BOUND ( 'NONE', #32483, .T. ) ;
#5854 = EDGE_CURVE ( 'NONE', #46920, #12938, #27938, .T. ) ;
#5855 = CARTESIAN_POINT ( 'NONE',  ( -2.210477865340801706, -37.43479381012853224, -9.422646554964178023 ) ) ;
#5856 = ORIENTED_EDGE ( 'NONE', *, *, #49764, .T. ) ;
#5857 = PLANE ( 'NONE',  #23829 ) ;
#5858 = CARTESIAN_POINT ( 'NONE',  ( -48.44597344681495343, 0.000000000000000000, 119.0682875569279702 ) ) ;
#5859 = CARTESIAN_POINT ( 'NONE',  ( 192.2789002873380184, 1.750000000000009548, 121.8434138227750623 ) ) ;
#5860 = AXIS2_PLACEMENT_3D ( 'NONE', #33793, #2227, #37648 ) ;
#5861 = ORIENTED_EDGE ( 'NONE', *, *, #25959, .F. ) ;
#5862 = CARTESIAN_POINT ( 'NONE',  ( 10.00000000000000000, -250.0000000000000000, 225.0000000000000000 ) ) ;
#5863 = ORIENTED_EDGE ( 'NONE', *, *, #16654, .T. ) ;
#5864 = ORIENTED_EDGE ( 'NONE', *, *, #24684, .T. ) ;
#5865 = FACE_OUTER_BOUND ( 'NONE', #49027, .T. ) ;
#5866 = ORIENTED_EDGE ( 'NONE', *, *, #26236, .T. ) ;
#5867 = DIRECTION ( 'NONE',  ( -1.000000000000000000, -0.000000000000000000, -0.000000000000000000 ) ) ;
#5868 = CARTESIAN_POINT ( 'NONE',  ( -13.92102703536724384, -30.85732372859812500, 8.356839323120299312 ) ) ;
#5869 = VERTEX_POINT ( 'NONE', #33384 ) ;
#5870 = CARTESIAN_POINT ( 'NONE',  ( 357.9999999999999432, -178.0000000000000000, 352.9999999999998295 ) ) ;
#5871 = DIRECTION ( 'NONE',  ( -2.220446049250312588E-16, -0.7071067811865475727, 0.7071067811865474617 ) ) ;
#5872 = FACE_OUTER_BOUND ( 'NONE', #3456, .T. ) ;
#5873 = AXIS2_PLACEMENT_3D ( 'NONE', #44458, #28577, #9338 ) ;
#5874 = CARTESIAN_POINT ( 'NONE',  ( 339.9999999999999432, 167.0000000000000000, -344.0000000000001705 ) ) ;
#5875 = ORIENTED_EDGE ( 'NONE', *, *, #33151, .F. ) ;
#5876 = DIRECTION ( 'NONE',  ( 0.000000000000000000, -1.822804496942679766E-16, -1.000000000000000000 ) ) ;
#5877 = ORIENTED_EDGE ( 'NONE', *, *, #39352, .F. ) ;
#5878 = CARTESIAN_POINT ( 'NONE',  ( -8.445973446814962315, -1.025126265847097207, 2.568287556927999926 ) ) ;
#5879 = LINE ( 'NONE', #45353, #50698 ) ;
#5880 = ORIENTED_EDGE ( 'NONE', *, *, #18054, .T. ) ;
#5881 = ORIENTED_EDGE ( 'NONE', *, *, #29143, .F. ) ;
#5882 = ORIENTED_EDGE ( 'NONE', *, *, #30777, .T. ) ;
#5883 = CARTESIAN_POINT ( 'NONE',  ( -1.193089574352124149, -0.2545860991493743564, 9.963925895596188909 ) ) ;
#5884 = CARTESIAN_POINT ( 'NONE',  ( -47.72109971266203132, 1.750000000000009548, 39.79316129108089228 ) ) ;
#5885 = EDGE_LOOP ( 'NONE', ( #39929, #19884, #19687, #34576 ) ) ;
#5886 = CARTESIAN_POINT ( 'NONE',  ( 0.7606162131530698201, -1.296876929034913140, 9.953784399990620813 ) ) ;
#5887 = CARTESIAN_POINT ( 'NONE',  ( -2.462075149652696027, 16.57295996686994499, 9.403735324607438884 ) ) ;
#5888 = CARTESIAN_POINT ( 'NONE',  ( -165.0000000000000284, 15.00000000000000000, 115.0000000000000142 ) ) ;
#5889 = EDGE_CURVE ( 'NONE', #37542, #31812, #21309, .T. ) ;
#5890 = CARTESIAN_POINT ( 'NONE',  ( -4.945973446814916130, 1.025126265847097651, 82.56828755692798438 ) ) ;
#5891 = EDGE_CURVE ( 'NONE', #4629, #3971, #17901, .T. ) ;
#5892 = EDGE_LOOP ( 'NONE', ( #32196, #5502, #38784, #26023 ) ) ;
#5893 = DIRECTION ( 'NONE',  ( 1.000000000000000000, 0.000000000000000000, 2.958228394578794270E-31 ) ) ;
#5894 = CARTESIAN_POINT ( 'NONE',  ( -65.00000000000002842, 17.00000000000000000, -90.00000000000000000 ) ) ;
#5895 = EDGE_CURVE ( 'NONE', #21583, #13512, #28423, .T. ) ;
#5896 = DIRECTION ( 'NONE',  ( 0.000000000000000000, -0.000000000000000000, -1.000000000000000000 ) ) ;
#5897 = VERTEX_POINT ( 'NONE', #16966 ) ;
#5898 = ADVANCED_FACE ( 'NONE', ( #44142 ), #37251, .F. ) ;
#5899 = EDGE_CURVE ( 'NONE', #43723, #48553, #7445, .T. ) ;
#5900 = DIRECTION ( 'NONE',  ( 0.000000000000000000, 5.664403186863042467E-17, 1.000000000000000000 ) ) ;
#5901 = CARTESIAN_POINT ( 'NONE',  ( -1.011271242968677875, -0.7347315653656004697, -10.00000000000000000 ) ) ;
#5902 = CIRCLE ( 'NONE', #21462, 50.00000000000000000 ) ;
#5903 = CARTESIAN_POINT ( 'NONE',  ( -26.18032376592659105, 21.95228666728381128, 7.455576670931136185 ) ) ;
#5904 = VERTEX_POINT ( 'NONE', #38503 ) ;
#5905 = DIRECTION ( 'NONE',  ( 1.000000000000000000, 0.000000000000000000, 0.000000000000000000 ) ) ;
#5906 = EDGE_CURVE ( 'NONE', #4790, #28808, #40554, .T. ) ;
#5907 = DIRECTION ( 'NONE',  ( -1.000000000000000000, 0.000000000000000000, 1.860490536778032451E-50 ) ) ;
#5908 = DIRECTION ( 'NONE',  ( -0.000000000000000000, 0.9749645535258953943, 0.2223603367690637489 ) ) ;
#5909 = CARTESIAN_POINT ( 'NONE',  ( 191.5540265531851105, 0.000000000000000000, -40.93171244307202983 ) ) ;
#5910 = VERTEX_POINT ( 'NONE', #33884 ) ;
#5911 = CARTESIAN_POINT ( 'NONE',  ( -166.6959734468149463, 1.750000000000009992, 0.8182875569279768335 ) ) ;
#5912 = ORIENTED_EDGE ( 'NONE', *, *, #26645, .T. ) ;
#5913 = CARTESIAN_POINT ( 'NONE',  ( -7.576114424932982594, 50.00000000000000711, 7.906207997025717304 ) ) ;
#5914 = ORIENTED_EDGE ( 'NONE', *, *, #13078, .F. ) ;
#5915 = DIRECTION ( 'NONE',  ( -1.000000000000000000, -0.000000000000000000, 4.625929269271584521E-16 ) ) ;
#5916 = CARTESIAN_POINT ( 'NONE',  ( 360.0000000000002274, 166.6568542494923406, 341.6568542494921417 ) ) ;
#5917 = AXIS2_PLACEMENT_3D ( 'NONE', #32974, #48558, #29109 ) ;
#5918 = EDGE_LOOP ( 'NONE', ( #14911, #33689, #33782, #18625 ) ) ;
#5919 =( BOUNDED_CURVE ( )  B_SPLINE_CURVE ( 3, ( #12475, #19926, #4537, #16088 ),
 .UNSPECIFIED., .F., .F. ) 
 B_SPLINE_CURVE_WITH_KNOTS ( ( 4, 4 ),
 ( 1.570796326794896558, 3.141592653589793116 ),
 .UNSPECIFIED. ) 
 CURVE ( )  GEOMETRIC_REPRESENTATION_ITEM ( )  RATIONAL_B_SPLINE_CURVE ( ( 1.000000000000000000, 0.8047378541243649375, 0.8047378541243649375, 1.000000000000000000 ) ) 
 REPRESENTATION_ITEM ( '' )  );
#5920 = CARTESIAN_POINT ( 'NONE',  ( 35.05402655318504657, 2.143131898507880377E-16, 39.06828755692798438 ) ) ;
#5921 = EDGE_LOOP ( 'NONE', ( #46869, #44703, #35440, #46941 ) ) ;
#5922 = DIRECTION ( 'NONE',  ( 1.000000000000000000, 0.000000000000000000, 0.000000000000000000 ) ) ;
#5923 = CYLINDRICAL_SURFACE ( 'NONE', #18290, 1.750000000000008438 ) ;
#5924 = VECTOR ( 'NONE', #38415, 1000.000000000000000 ) ;
#5925 = CARTESIAN_POINT ( 'NONE',  ( 115.0540265531850395, 2.143131898507847836E-16, 42.56828755692795596 ) ) ;
#5926 = DIRECTION ( 'NONE',  ( -0.000000000000000000, -1.000000000000000000, -0.000000000000000000 ) ) ;
#5927 = CIRCLE ( 'NONE', #12481, 40.00000000000000000 ) ;
#5928 = CARTESIAN_POINT ( 'NONE',  ( 113.3040265531850537, 0.000000000000000000, 165.0000000000000000 ) ) ;
#5929 = ORIENTED_EDGE ( 'NONE', *, *, #40910, .F. ) ;
#5930 = ORIENTED_EDGE ( 'NONE', *, *, #28345, .T. ) ;
#5931 = CARTESIAN_POINT ( 'NONE',  ( 0.3862712429686810944, 1.188820645368943607, 10.00000000000000000 ) ) ;
#5933 = EDGE_CURVE ( 'NONE', #11195, #4845, #41817, .T. ) ;
#5932 = VECTOR ( 'NONE', #41070, 1000.000000000000000 ) ;
#5934 = ORIENTED_EDGE ( 'NONE', *, *, #8795, .T. ) ;
#5935 = CIRCLE ( 'NONE', #1009, 2.000000000000001776 ) ;
#5936 = CARTESIAN_POINT ( 'NONE',  ( 10.50000000000000178, -46.12433806312137108, 6.404467680894761372 ) ) ;
#5937 = DIRECTION ( 'NONE',  ( 0.000000000000000000, -2.969158215481698263E-48, 1.000000000000000000 ) ) ;
#5938 = EDGE_LOOP ( 'NONE', ( #47149, #38697, #19708, #8780 ) ) ;
#5939 = B_SPLINE_CURVE_WITH_KNOTS ( 'NONE', 3,
 ( #50163, #18407, #25869, #2257 ),
 .UNSPECIFIED., .F., .F.,
 ( 4, 4 ),
 ( 0.000000000000000000, 0.002368422649471296423 ),
 .UNSPECIFIED. ) ;
#5940 = CARTESIAN_POINT ( 'NONE',  ( 10.25676241992214344, 8.638513918217336496, -18.89424093979656760 ) ) ;
#5941 =( BOUNDED_CURVE ( )  B_SPLINE_CURVE ( 3, ( #663, #32719, #44743, #36845 ),
 .UNSPECIFIED., .F., .F. ) 
 B_SPLINE_CURVE_WITH_KNOTS ( ( 4, 4 ),
 ( 3.141592653589793116, 4.712388980384689674 ),
 .UNSPECIFIED. ) 
 CURVE ( )  GEOMETRIC_REPRESENTATION_ITEM ( )  RATIONAL_B_SPLINE_CURVE ( ( 1.000000000000000000, 0.8047378541243649375, 0.8047378541243649375, 1.000000000000000000 ) ) 
 REPRESENTATION_ITEM ( '' )  );
#5942 = DIRECTION ( 'NONE',  ( 0.000000000000000000, 0.000000000000000000, 1.000000000000000000 ) ) ;
#5943 = ORIENTED_EDGE ( 'NONE', *, *, #592, .F. ) ;
#5944 = CARTESIAN_POINT ( 'NONE',  ( 194.3291528190321742, 1.750000000000010214, -78.15658617722490931 ) ) ;
#5945 = CARTESIAN_POINT ( 'NONE',  ( -126.6959734468149321, 1.749999999999997113, -39.18171244307202983 ) ) ;
#5946 = LINE ( 'NONE', #13389, #42147 ) ;
#5947 = CARTESIAN_POINT ( 'NONE',  ( 115.0540265531850395, 2.143131898507847836E-16, 39.06828755692798438 ) ) ;
#5948 = ORIENTED_EDGE ( 'NONE', *, *, #6745, .T. ) ;
#5949 = ORIENTED_EDGE ( 'NONE', *, *, #2208, .F. ) ;
#5950 = MANIFOLD_SOLID_BREP ( 'Mirror1', #35140 ) ;
#5951 = CARTESIAN_POINT ( 'NONE',  ( -397.9839762253770346, 0.000000000000000000, 197.0020682315616796 ) ) ;
#5952 = DIRECTION ( 'NONE',  ( 1.000000000000000000, 0.000000000000000000, -0.000000000000000000 ) ) ;
#5953 = CARTESIAN_POINT ( 'NONE',  ( 35.00000000000028422, 17.00000000000000000, -84.99999999999998579 ) ) ;
#5954 = DIRECTION ( 'NONE',  ( 0.000000000000000000, 0.000000000000000000, 1.000000000000000000 ) ) ;
#5955 = AXIS2_PLACEMENT_3D ( 'NONE', #12138, #21083, #14132 ) ;
#5956 = DIRECTION ( 'NONE',  ( -1.000000000000000000, -0.000000000000000000, -0.000000000000000000 ) ) ;
#5957 = ORIENTED_EDGE ( 'NONE', *, *, #37256, .T. ) ;
#5958 = DIRECTION ( 'NONE',  ( 0.000000000000000000, 0.000000000000000000, -1.000000000000000000 ) ) ;
#5959 = VERTEX_POINT ( 'NONE', #18462 ) ;
#5960 =( LENGTH_UNIT ( ) NAMED_UNIT ( * ) SI_UNIT ( .MILLI., .METRE. ) );
#5961 = EDGE_CURVE ( 'NONE', #18600, #42641, #7446, .T. ) ;
#5962 = DIRECTION ( 'NONE',  ( 0.000000000000000000, 0.000000000000000000, 1.000000000000000000 ) ) ;
#5963 = DIRECTION ( 'NONE',  ( -0.000000000000000000, -1.000000000000000000, -0.000000000000000000 ) ) ;
#5964 = CYLINDRICAL_SURFACE ( 'NONE', #46278, 1.750000000000008438 ) ;
#5965 = PLANE ( 'NONE',  #33978 ) ;
#5966 = VECTOR ( 'NONE', #15694, 1000.000000000000000 ) ;
#5967 = DIRECTION ( 'NONE',  ( 1.000000000000000000, 0.000000000000000000, 0.000000000000000000 ) ) ;
#5968 = ORIENTED_EDGE ( 'NONE', *, *, #49942, .F. ) ;
#5969 = ADVANCED_FACE ( 'NONE', ( #6662 ), #2810, .F. ) ;
#5970 = CARTESIAN_POINT ( 'NONE',  ( 193.3040265531851105, -1.750000000000010214, -39.18171244307202983 ) ) ;
#5971 = AXIS2_PLACEMENT_3D ( 'NONE', #41236, #13024, #20732 ) ;
#5972 = CARTESIAN_POINT ( 'NONE',  ( 168.9999999999999716, 6.000000000000060396, -340.0000000000001137 ) ) ;
#5973 = CARTESIAN_POINT ( 'NONE',  ( -164.4973046169135955, -61.66198943095990614, -93.79675437945473959 ) ) ;
#5974 = B_SPLINE_CURVE_WITH_KNOTS ( 'NONE', 3,
 ( #25220, #18009, #14155, #5710 ),
 .UNSPECIFIED., .F., .F.,
 ( 4, 4 ),
 ( 0.0002936521407493293328, 0.0006663369986113973614 ),
 .UNSPECIFIED. ) ;
#5975 = AXIS2_PLACEMENT_3D ( 'NONE', #19675, #31494, #50674 ) ;
#5976 = CARTESIAN_POINT ( 'NONE',  ( 16.76006782980217125, -2.050259795448531541, 9.178419661560148768 ) ) ;
#5977 = EDGE_LOOP ( 'NONE', ( #29681, #17204, #46672, #34831 ) ) ;
#5978 = VECTOR ( 'NONE', #21618, 1000.000000000000000 ) ;
#5979 = CARTESIAN_POINT ( 'NONE',  ( -27.31081730472607561, -41.96092862852123773, 3.199614146704519602 ) ) ;
#5980 = EDGE_LOOP ( 'NONE', ( #45782, #15733, #28671, #12013 ) ) ;
#5981 = DIRECTION ( 'NONE',  ( -1.000000000000000000, 0.000000000000000000, -7.793956916774525800E-48 ) ) ;
#5982 = CARTESIAN_POINT ( 'NONE',  ( 360.0000000000001137, 181.0000000000000284, 349.9999999999998295 ) ) ;
#5983 = CARTESIAN_POINT ( 'NONE',  ( 111.5540265531850679, 0.000000000000000000, 165.0000000000000000 ) ) ;
#5984 = VERTEX_POINT ( 'NONE', #14105 ) ;
#5985 = LINE ( 'NONE', #13924, #5753 ) ;
#5986 = CARTESIAN_POINT ( 'NONE',  ( 1.250000000000000222, 0.000000000000000000, -10.00000000000000000 ) ) ;
#5987 = CARTESIAN_POINT ( 'NONE',  ( 75.05402655318509630, 2.143131898507880377E-16, -77.43171244307198720 ) ) ;
#5988 = CARTESIAN_POINT ( 'NONE',  ( 357.9999999999999432, -165.0000000000001137, -106.0000000000001990 ) ) ;
#5989 = ORIENTED_EDGE ( 'NONE', *, *, #41771, .T. ) ;
#5990 = EDGE_LOOP ( 'NONE', ( #39418, #17995, #11209, #40774 ) ) ;
#5991 = DIRECTION ( 'NONE',  ( -1.000000000000000000, 0.000000000000000000, 0.000000000000000000 ) ) ;
#5992 = CARTESIAN_POINT ( 'NONE',  ( -124.9459734468149463, 2.143131898507847836E-16, -37.43171244307205825 ) ) ;
#5993 = EDGE_CURVE ( 'NONE', #16365, #3789, #26927, .T. ) ;
#5994 = ORIENTED_EDGE ( 'NONE', *, *, #31272, .F. ) ;
#5995 = ORIENTED_EDGE ( 'NONE', *, *, #18018, .T. ) ;
#5996 = CARTESIAN_POINT ( 'NONE',  ( 154.3291528190321458, 1.750000000000010214, -78.15658617722490931 ) ) ;
#5997 = CARTESIAN_POINT ( 'NONE',  ( -85.67084718096784002, 1.750000000000010214, -78.15658617722490931 ) ) ;
#5998 = CARTESIAN_POINT ( 'NONE',  ( -206.6959734468149463, 1.750000000000010658, 80.81828755692798438 ) ) ;
#5999 = CARTESIAN_POINT ( 'NONE',  ( -84.94597344681493212, -1.025126265847089213, 42.56828755692799149 ) ) ;
#6000 = EDGE_LOOP ( 'NONE', ( #35629, #27430, #11990, #50346 ) ) ;
#6001 = VECTOR ( 'NONE', #46006, 1000.000000000000000 ) ;
#6002 = ORIENTED_EDGE ( 'NONE', *, *, #22415, .T. ) ;
#6003 = VECTOR ( 'NONE', #31881, 1000.000000000000000 ) ;
#6004 = CARTESIAN_POINT ( 'NONE',  ( 48.98697415750967821, 11.03699497439252220, -8.016098858316205167 ) ) ;
#6005 = CARTESIAN_POINT ( 'NONE',  ( 350.0000000000000000, -175.0000000000000000, 349.9999999999998295 ) ) ;
#6006 = AXIS2_PLACEMENT_3D ( 'NONE', #6408, #26919, #22309 ) ;
#6007 = VERTEX_POINT ( 'NONE', #42323 ) ;
#6008 = ORIENTED_EDGE ( 'NONE', *, *, #47342, .T. ) ;
#6009 = DIRECTION ( 'NONE',  ( 0.000000000000000000, 0.000000000000000000, 1.000000000000000000 ) ) ;
#6010 = CARTESIAN_POINT ( 'NONE',  ( -207.7210997126620384, 1.750000000000009326, -158.1565861772249377 ) ) ;
#6011 = VERTEX_POINT ( 'NONE', #7182 ) ;
#6012 = ORIENTED_EDGE ( 'NONE', *, *, #8932, .T. ) ;
#6013 = CARTESIAN_POINT ( 'NONE',  ( -126.6959734468149321, 1.749999999999997113, 40.81828755692798438 ) ) ;
#6014 = LINE ( 'NONE', #24519, #32174 ) ;
#6015 = VERTEX_POINT ( 'NONE', #22823 ) ;
#6016 = DIRECTION ( 'NONE',  ( 1.000000000000000000, 0.000000000000000000, -0.000000000000000000 ) ) ;
#6017 = CARTESIAN_POINT ( 'NONE',  ( 193.3040265531851105, 0.000000000000000000, 165.0000000000000000 ) ) ;
#6018 = DIRECTION ( 'NONE',  ( -0.000000000000000000, -1.000000000000000000, -0.000000000000000000 ) ) ;
#6019 = DIRECTION ( 'NONE',  ( 0.000000000000000000, -3.186989995019654210E-49, -1.000000000000000000 ) ) ;
#6020 = VECTOR ( 'NONE', #23765, 1000.000000000000000 ) ;
#6021 =( BOUNDED_CURVE ( )  B_SPLINE_CURVE ( 3, ( #14558, #22513, #2754, #21763 ),
 .UNSPECIFIED., .F., .F. ) 
 B_SPLINE_CURVE_WITH_KNOTS ( ( 4, 4 ),
 ( 3.141592653589793116, 4.712388980384689674 ),
 .UNSPECIFIED. ) 
 CURVE ( )  GEOMETRIC_REPRESENTATION_ITEM ( )  RATIONAL_B_SPLINE_CURVE ( ( 1.000000000000000000, 0.8047378541243649375, 0.8047378541243649375, 1.000000000000000000 ) ) 
 REPRESENTATION_ITEM ( '' )  );
#6022 = CARTESIAN_POINT ( 'NONE',  ( -6.408332700304190332, -7.676800896350769676, 0.000000000000000000 ) ) ;
#6023 = ORIENTED_EDGE ( 'NONE', *, *, #39006, .T. ) ;
#6024 = EDGE_CURVE ( 'NONE', #43206, #27540, #39416, .T. ) ;
#6025 = CARTESIAN_POINT ( 'NONE',  ( 232.4999999999999716, -169.9999999999999716, 4.999999999999616307 ) ) ;
#6026 = CARTESIAN_POINT ( 'NONE',  ( 0.3862712429686727678, 1.188820645368945605, 3.333333333333333481 ) ) ;
#6027 = LINE ( 'NONE', #48839, #21180 ) ;
#6028 = CARTESIAN_POINT ( 'NONE',  ( 183.0000000000000000, -93.49999999999998579, -350.0000000000001705 ) ) ;
#6029 = DIRECTION ( 'NONE',  ( -2.958228394578793832E-31, 0.000000000000000000, -1.000000000000000000 ) ) ;
#6030 = CARTESIAN_POINT ( 'NONE',  ( -37.27397286063865778, 4.111076158911805223, 7.697694107796192675 ) ) ;
#6031 = VECTOR ( 'NONE', #46909, 1000.000000000000000 ) ;
#6032 = DIRECTION ( 'NONE',  ( -1.000000000000000000, 0.000000000000000000, 0.000000000000000000 ) ) ;
#6033 = CIRCLE ( 'NONE', #11801, 1.750000000000009992 ) ;
#6034 = EDGE_CURVE ( 'NONE', #28309, #39980, #1894, .T. ) ;
#6035 = CARTESIAN_POINT ( 'NONE',  ( -1.424725715586989239, 0.8249487629949916467, 9.927568724237804787 ) ) ;
#6036 = EDGE_CURVE ( 'NONE', #10604, #36951, #45755, .T. ) ;
#6037 = DIRECTION ( 'NONE',  ( -0.9928768384869220975, 0.000000000000000000, -0.1191452206184307611 ) ) ;
#6038 = AXIS2_PLACEMENT_3D ( 'NONE', #17098, #36370, #21699 ) ;
#6039 = ADVANCED_FACE ( 'NONE', ( #45641 ), #15893, .F. ) ;
#6040 = EDGE_CURVE ( 'NONE', #26888, #1022, #38745, .T. ) ;
#6041 = VECTOR ( 'NONE', #45873, 1000.000000000000000 ) ;
#6042 = ORIENTED_EDGE ( 'NONE', *, *, #7705, .F. ) ;
#6043 = CARTESIAN_POINT ( 'NONE',  ( 33.30402655318503946, 1.750000000000010658, 120.8182875569279702 ) ) ;
#6044 = CARTESIAN_POINT ( 'NONE',  ( -30.12518629743573584, -14.70074613238887551, 1.847720168420772691 ) ) ;
#6045 = DIRECTION ( 'NONE',  ( -0.000000000000000000, -0.000000000000000000, -1.000000000000000000 ) ) ;
#6046 = CARTESIAN_POINT ( 'NONE',  ( 27.33593271309472073, -41.94268121623323964, -9.367992836599954742 ) ) ;
#6047 = CARTESIAN_POINT ( 'NONE',  ( 7.499999999999944045, -224.9999999999999716, -240.0000000000000000 ) ) ;
#6048 = ORIENTED_EDGE ( 'NONE', *, *, #22870, .F. ) ;
#6049 = CYLINDRICAL_SURFACE ( 'NONE', #46991, 2.000000000000001776 ) ;
#6050 = B_SPLINE_SURFACE_WITH_KNOTS ( 'NONE', 3, 3, ( 
 ( #5451, #21103, #44683, #45176 ),
 ( #33183, #21607, #21874, #9561 ),
 ( #25210, #9800, #25463, #40857 ),
 ( #5703, #21353, #37041, #48767 ) ),
 .UNSPECIFIED., .F., .F., .F.,
 ( 4, 4 ),
 ( 4, 4 ),
 ( 0.000000000000000000, 1.000000000000000000 ),
 ( 0.000000000000000000, 1.000000000000000000 ),
 .UNSPECIFIED. ) ;
#6051 = EDGE_CURVE ( 'NONE', #42585, #27971, #31045, .T. ) ;
#6053 = ORIENTED_EDGE ( 'NONE', *, *, #39805, .F. ) ;
#6052 = EDGE_CURVE ( 'NONE', #22572, #46647, #23849, .T. ) ;
#6054 = CARTESIAN_POINT ( 'NONE',  ( 164.9999999999999716, 17.00000000000000000, 65.00000000000000000 ) ) ;
#6055 = LINE ( 'NONE', #21702, #5793 ) ;
#6056 = UNCERTAINTY_MEASURE_WITH_UNIT (LENGTH_MEASURE( 1.000000000000000082E-05 ), #3542, 'distance_accuracy_value', 'NONE');
#6057 = EDGE_CURVE ( 'NONE', #13717, #40787, #8453, .T. ) ;
#6058 = EDGE_CURVE ( 'NONE', #4113, #26133, #12537, .T. ) ;
#6059 = VECTOR ( 'NONE', #20162, 1000.000000000000000 ) ;
#6060 = ORIENTED_EDGE ( 'NONE', *, *, #4498, .F. ) ;
#6061 = DIRECTION ( 'NONE',  ( -1.000000000000000000, -0.000000000000000000, -0.000000000000000000 ) ) ;
#6062 = ORIENTED_EDGE ( 'NONE', *, *, #12416, .T. ) ;
#6063 = ORIENTED_EDGE ( 'NONE', *, *, #14408, .F. ) ;
#6064 = VERTEX_POINT ( 'NONE', #12050 ) ;
#6065 = CARTESIAN_POINT ( 'NONE',  ( 169.0000000000000000, -174.9999999999999716, -111.0000000000001563 ) ) ;
#6066 = CARTESIAN_POINT ( 'NONE',  ( -124.9459734468149463, 2.143131898507847836E-16, -160.9317124430720014 ) ) ;
#6067 = FACE_OUTER_BOUND ( 'NONE', #28869, .T. ) ;
#6068 = EDGE_LOOP ( 'NONE', ( #16968, #18794, #14384, #46517, #24022, #25623 ) ) ;
#6069 = DIRECTION ( 'NONE',  ( -1.586032892321652236E-16, -1.000000000000000000, -2.288264760618012091E-48 ) ) ;
#6070 = DIRECTION ( 'NONE',  ( 0.000000000000000000, 1.000000000000000000, 0.000000000000000000 ) ) ;
#6071 = ORIENTED_EDGE ( 'NONE', *, *, #300, .T. ) ;
#6072 = ORIENTED_EDGE ( 'NONE', *, *, #47432, .F. ) ;
#6073 = CARTESIAN_POINT ( 'NONE',  ( 168.9999999999999716, -174.9999999999999716, -344.0000000000001137 ) ) ;
#6074 = VECTOR ( 'NONE', #18713, 1000.000000000000000 ) ;
#6075 = CARTESIAN_POINT ( 'NONE',  ( -0.3862712429686809279, -1.188820645368943163, -10.00000000000000000 ) ) ;
#6076 = DIRECTION ( 'NONE',  ( 1.000000000000000000, -0.000000000000000000, 0.000000000000000000 ) ) ;
#6077 = ORIENTED_EDGE ( 'NONE', *, *, #10976, .T. ) ;
#6078 = ADVANCED_FACE ( 'NONE', ( #16390 ), #22347, .T. ) ;
#6079 = VECTOR ( 'NONE', #25455, 1000.000000000000000 ) ;
#6080 = CARTESIAN_POINT ( 'NONE',  ( 113.3040265531850537, -1.749999999999997113, 40.81828755692798438 ) ) ;
#6081 = CARTESIAN_POINT ( 'NONE',  ( -36.32827987961121607, 9.445964435369075929, 3.209567239418972928 ) ) ;
#6082 =( BOUNDED_CURVE ( )  B_SPLINE_CURVE ( 3, ( #16615, #31527, #713, #4800 ),
 .UNSPECIFIED., .F., .F. ) 
 B_SPLINE_CURVE_WITH_KNOTS ( ( 4, 4 ),
 ( 1.570796326794896558, 3.141592653589793116 ),
 .UNSPECIFIED. ) 
 CURVE ( )  GEOMETRIC_REPRESENTATION_ITEM ( )  RATIONAL_B_SPLINE_CURVE ( ( 1.000000000000000000, 0.8047378541243649375, 0.8047378541243649375, 1.000000000000000000 ) ) 
 REPRESENTATION_ITEM ( '' )  );
#6083 = ADVANCED_FACE ( 'NONE', ( #27694 ), #34255, .T. ) ;
#6084 = CARTESIAN_POINT ( 'NONE',  ( 2.052560157877110658, -0.2040521727611157299, 9.891980816076525684 ) ) ;
#6085 = CARTESIAN_POINT ( 'NONE',  ( 0.8285222815141930486, 1.889008401827334094, 9.886433018048068178 ) ) ;
#6086 = EDGE_CURVE ( 'NONE', #4778, #37949, #47697, .T. ) ;
#6087 = CARTESIAN_POINT ( 'NONE',  ( -204.9459734468148895, -1.025126265847089657, -120.9317124430720440 ) ) ;
#6088 = DIRECTION ( 'NONE',  ( -0.000000000000000000, -1.000000000000000000, -0.000000000000000000 ) ) ;
#6089 = EDGE_CURVE ( 'NONE', #33102, #14175, #39251, .T. ) ;
#6090 = CARTESIAN_POINT ( 'NONE',  ( 44.25629667545849344, -43.33333333333335702, 790.0000000000000000 ) ) ;
#6091 =( BOUNDED_CURVE ( )  B_SPLINE_CURVE ( 3, ( #26181, #41825, #18712, #6669 ),
 .UNSPECIFIED., .F., .F. ) 
 B_SPLINE_CURVE_WITH_KNOTS ( ( 4, 4 ),
 ( 3.141592653589793116, 4.712388980384689674 ),
 .UNSPECIFIED. ) 
 CURVE ( )  GEOMETRIC_REPRESENTATION_ITEM ( )  RATIONAL_B_SPLINE_CURVE ( ( 1.000000000000000000, 0.8047378541243649375, 0.8047378541243649375, 1.000000000000000000 ) ) 
 REPRESENTATION_ITEM ( '' )  );
#6092 = LINE ( 'NONE', #28447, #34667 ) ;
#6093 = DIRECTION ( 'NONE',  ( -1.000000000000000000, -0.000000000000000000, -0.000000000000000000 ) ) ;
#6094 = EDGE_CURVE ( 'NONE', #28572, #33964, #35338, .T. ) ;
#6095 = CARTESIAN_POINT ( 'NONE',  ( 210.0000000000000568, 0.000000000000000000, -157.4317124430720298 ) ) ;
#6096 = VECTOR ( 'NONE', #16521, 1000.000000000000000 ) ;
#6097 = CARTESIAN_POINT ( 'NONE',  ( 0.000000000000000000, 0.000000000000000000, 0.000000000000000000 ) ) ;
#6098 = VECTOR ( 'NONE', #13478, 1000.000000000000000 ) ;
#6099 = EDGE_LOOP ( 'NONE', ( #43587, #31846, #9985, #46890, #4156, #9861 ) ) ;
#6100 = CARTESIAN_POINT ( 'NONE',  ( 181.0000000000003411, 165.0000000000000000, 359.9999999999997726 ) ) ;
#6101 = DIRECTION ( 'NONE',  ( 1.000000000000000000, 0.000000000000000000, 0.000000000000000000 ) ) ;
#6102 = ORIENTED_EDGE ( 'NONE', *, *, #5184, .T. ) ;
#6103 = CARTESIAN_POINT ( 'NONE',  ( 155.0540265531850537, 2.143131898507880377E-16, -40.93171244307202983 ) ) ;
#6104 = DIRECTION ( 'NONE',  ( 0.000000000000000000, 0.000000000000000000, 1.000000000000000000 ) ) ;
#6105 = AXIS2_PLACEMENT_3D ( 'NONE', #16237, #24449, #36257 ) ;
#6106 = EDGE_CURVE ( 'NONE', #17197, #14015, #20743, .T. ) ;
#6107 = ORIENTED_EDGE ( 'NONE', *, *, #222, .F. ) ;
#6108 = CARTESIAN_POINT ( 'NONE',  ( -5.670847180967843570, -1.750000000000022427, -158.1565861772249093 ) ) ;
#6109 = CYLINDRICAL_SURFACE ( 'NONE', #906, 1.749999999999987566 ) ;
#6110 = CARTESIAN_POINT ( 'NONE',  ( -206.6959734468149463, 1.750000000000009992, -159.1817124430720298 ) ) ;
#6111 = CARTESIAN_POINT ( 'NONE',  ( 191.5540265531851105, 0.000000000000000000, 122.5682875569279702 ) ) ;
#6112 = ORIENTED_EDGE ( 'NONE', *, *, #7061, .F. ) ;
#6113 = CARTESIAN_POINT ( 'NONE',  ( 168.9999999999999716, -272.5000000000000000, -114.9999999999999147 ) ) ;
#6115 = ORIENTED_EDGE ( 'NONE', *, *, #7131, .F. ) ;
#6114 = EDGE_CURVE ( 'NONE', #31257, #49939, #4078, .T. ) ;
#6116 = ORIENTED_EDGE ( 'NONE', *, *, #4179, .F. ) ;
#6117 = VECTOR ( 'NONE', #24580, 1000.000000000000000 ) ;
#6118 = CARTESIAN_POINT ( 'NONE',  ( 356.0000000000001137, 165.0000000000000000, 339.9999999999998295 ) ) ;
#6119 = EDGE_CURVE ( 'NONE', #43660, #17110, #32311, .T. ) ;
#6120 = EDGE_CURVE ( 'NONE', #32197, #20771, #1264, .T. ) ;
#6121 = ORIENTED_EDGE ( 'NONE', *, *, #25589, .F. ) ;
#6122 = DIRECTION ( 'NONE',  ( 1.000000000000000000, 0.000000000000000000, 0.000000000000000000 ) ) ;
#6123 = CARTESIAN_POINT ( 'NONE',  ( 75.05402655318509630, 2.143131898507880377E-16, -80.93171244307204404 ) ) ;
#6124 = ORIENTED_EDGE ( 'NONE', *, *, #44962, .F. ) ;
#6125 = CARTESIAN_POINT ( 'NONE',  ( 155.0540265531850537, 2.143131898507880377E-16, 79.06828755692797017 ) ) ;
#6126 = EDGE_CURVE ( 'NONE', #43660, #32627, #16908, .T. ) ;
#6127 = CYLINDRICAL_SURFACE ( 'NONE', #8544, 1.750000000000008438 ) ;
#6128 = EDGE_CURVE ( 'NONE', #33080, #35109, #33318, .T. ) ;
#6129 = CARTESIAN_POINT ( 'NONE',  ( 33.30402655318503946, 1.750000000000009992, 0.8182875569279768335 ) ) ;
#6130 = ORIENTED_EDGE ( 'NONE', *, *, #20040, .F. ) ;
#6131 = CARTESIAN_POINT ( 'NONE',  ( 210.0000000000000568, 2.143131898507880377E-16, 159.0682875569279702 ) ) ;
#6132 = CARTESIAN_POINT ( 'NONE',  ( 35.00000000000216716, 17.00000000000000000, 95.00000000000000000 ) ) ;
#6133 = CARTESIAN_POINT ( 'NONE',  ( -114.9999999999984652, 16.00000000000000000, 35.00000000000000000 ) ) ;
#6134 = VECTOR ( 'NONE', #42620, 1000.000000000000000 ) ;
#6135 = ORIENTED_EDGE ( 'NONE', *, *, #19751, .F. ) ;
#6136 = DIRECTION ( 'NONE',  ( -1.000000000000000000, -0.000000000000000000, -0.000000000000000000 ) ) ;
#6137 = DIRECTION ( 'NONE',  ( 0.000000000000000000, 0.000000000000000000, -1.000000000000000000 ) ) ;
#6138 = ORIENTED_EDGE ( 'NONE', *, *, #15141, .F. ) ;
#6139 = VECTOR ( 'NONE', #37000, 1000.000000000000000 ) ;
#6140 = EDGE_LOOP ( 'NONE', ( #49167, #19830, #37309, #22354 ) ) ;
#6141 = ORIENTED_EDGE ( 'NONE', *, *, #21807, .T. ) ;
#6142 = CARTESIAN_POINT ( 'NONE',  ( -4.945973446814903696, 2.143131898507912917E-16, -157.4317124430720014 ) ) ;
#6143 = CARTESIAN_POINT ( 'NONE',  ( 21.61731705588930907, 25.43568671410602278, -9.367992836599954742 ) ) ;
#6144 = VERTEX_POINT ( 'NONE', #32568 ) ;
#6145 = CARTESIAN_POINT ( 'NONE',  ( -208.4459734468149463, 0.000000000000000000, 165.0000000000000000 ) ) ;
#6146 = LINE ( 'NONE', #1549, #36115 ) ;
#6147 = CARTESIAN_POINT ( 'NONE',  ( 31.44259251615245887, 38.95901822126168668, -9.367992836599954742 ) ) ;
#6148 = CARTESIAN_POINT ( 'NONE',  ( 210.0000000000000568, 0.000000000000000000, -119.1817124430720440 ) ) ;
#6149 = EDGE_CURVE ( 'NONE', #35238, #7083, #48151, .T. ) ;
#6150 = ORIENTED_EDGE ( 'NONE', *, *, #28338, .T. ) ;
#6151 = VECTOR ( 'NONE', #41388, 1000.000000000000000 ) ;
#6152 = PLANE ( 'NONE',  #17129 ) ;
#6153 = LINE ( 'NONE', #13336, #13616 ) ;
#6154 = CARTESIAN_POINT ( 'NONE',  ( -28.96803024440907137, -18.11533787072017176, 7.455576670931136185 ) ) ;
#6155 = B_SPLINE_CURVE_WITH_KNOTS ( 'NONE', 3,
 ( #34668, #22087, #30055, #45909 ),
 .UNSPECIFIED., .F., .F.,
 ( 4, 4 ),
 ( 0.7998230999345287140, 0.9869080488566183140 ),
 .UNSPECIFIED. ) ;
#6156 = AXIS2_PLACEMENT_3D ( 'NONE', #20350, #36536, #24721 ) ;
#6157 = ORIENTED_EDGE ( 'NONE', *, *, #39006, .F. ) ;
#6158 = CONTEXT_DEPENDENT_SHAPE_REPRESENTATION ( #43345, #39310 ) ;
#6159 = CARTESIAN_POINT ( 'NONE',  ( 193.3040265531851105, -1.750000000000010214, -39.18171244307202983 ) ) ;
#6160 = CARTESIAN_POINT ( 'NONE',  ( 356.0000000000001137, 185.0000000000000284, 349.9999999999998295 ) ) ;
#6161 = LINE ( 'NONE', #21815, #21605 ) ;
#6162 = DIRECTION ( 'NONE',  ( -0.000000000000000000, -1.000000000000000000, -0.000000000000000000 ) ) ;
#6163 = ORIENTED_EDGE ( 'NONE', *, *, #39420, .F. ) ;
#6164 = CARTESIAN_POINT ( 'NONE',  ( 168.9999999999999716, -256.4999999999999432, -339.9999999999998863 ) ) ;
#6165 = ADVANCED_FACE ( 'NONE', ( #21246 ), #13036, .T. ) ;
#6166 = DIRECTION ( 'NONE',  ( -1.000000000000000000, 0.000000000000000000, -0.000000000000000000 ) ) ;
#6167 = CARTESIAN_POINT ( 'NONE',  ( -14.86945752723352498, -7.944783388878907004, 2.590526750877053086 ) ) ;
#6168 = CARTESIAN_POINT ( 'NONE',  ( -128.4459734468149179, 0.000000000000000000, 122.5682875569279418 ) ) ;
#6169 = DIRECTION ( 'NONE',  ( 0.000000000000000000, 1.000000000000000000, 7.004339610132985974E-48 ) ) ;
#6170 = ORIENTED_EDGE ( 'NONE', *, *, #1388, .T. ) ;
#6171 = AXIS2_PLACEMENT_3D ( 'NONE', #43471, #16791, #47542 ) ;
#6172 = CARTESIAN_POINT ( 'NONE',  ( -64.99999999999783995, 16.00000000000000000, 95.00000000000000000 ) ) ;
#6173 = VERTEX_POINT ( 'NONE', #45072 ) ;
#6174 = CARTESIAN_POINT ( 'NONE',  ( 164.9999999999999716, 17.00000000000000000, 95.00000000000000000 ) ) ;
#6175 = EDGE_CURVE ( 'NONE', #4762, #43380, #5347, .T. ) ;
#6176 = VECTOR ( 'NONE', #12500, 1000.000000000000000 ) ;
#6177 = ORIENTED_EDGE ( 'NONE', *, *, #14200, .T. ) ;
#6178 = LINE ( 'NONE', #21835, #1669 ) ;
#6179 = DIRECTION ( 'NONE',  ( 1.000000000000000000, 0.000000000000000000, 0.000000000000000000 ) ) ;
#6180 = AXIS2_PLACEMENT_3D ( 'NONE', #12584, #5394, #32874 ) ;
#6181 = FILL_AREA_STYLE_COLOUR ( '', #2741 ) ;
#6182 = ORIENTED_EDGE ( 'NONE', *, *, #1354, .F. ) ;
#6183 = COLOUR_RGB ( '',0.7921568627450980005, 0.8196078431372548767, 0.9333333333333333481 ) ;
#6184 = ADVANCED_FACE ( 'NONE', ( #2004 ), #17651, .F. ) ;
#6185 = CARTESIAN_POINT ( 'NONE',  ( 85.00000000000213163, 17.00000000000000000, 95.00000000000000000 ) ) ;
#6186 = EDGE_CURVE ( 'NONE', #33652, #36453, #18067, .T. ) ;
#6187 = ORIENTED_EDGE ( 'NONE', *, *, #28725, .T. ) ;
#6188 = CARTESIAN_POINT ( 'NONE',  ( 195.0540265531851105, 2.143131898507880377E-16, 162.5682875569279702 ) ) ;
#6189 = DIRECTION ( 'NONE',  ( -0.000000000000000000, -0.000000000000000000, -1.000000000000000000 ) ) ;
#6190 = AXIS2_PLACEMENT_3D ( 'NONE', #1242, #16884, #48377 ) ;
#6191 = DIRECTION ( 'NONE',  ( -1.586032892321652236E-16, -1.000000000000000000, -6.853681917100419162E-49 ) ) ;
#6192 = CARTESIAN_POINT ( 'NONE',  ( -126.6959734468149321, 1.749999999999997335, -119.1817124430720440 ) ) ;
#6193 = PLANE ( 'NONE',  #1972 ) ;
#6194 = ORIENTED_EDGE ( 'NONE', *, *, #31295, .F. ) ;
#6195 = EDGE_CURVE ( 'NONE', #42902, #25915, #24363, .T. ) ;
#6196 = PRODUCT_DEFINITION_FORMATION_WITH_SPECIFIED_SOURCE ( 'ANY', '', #26565, .NOT_KNOWN. ) ;
#6197 = ORIENTED_EDGE ( 'NONE', *, *, #16528, .F. ) ;
#6198 = CARTESIAN_POINT ( 'NONE',  ( 193.3040265531851105, 1.750000000000009992, 160.8182875569279702 ) ) ;
#6199 = VECTOR ( 'NONE', #33678, 1000.000000000000000 ) ;
#6200 = EDGE_CURVE ( 'NONE', #48473, #20980, #14617, .T. ) ;
#6201 = EDGE_CURVE ( 'NONE', #47750, #27906, #24853, .T. ) ;
#6202 = VERTEX_POINT ( 'NONE', #5589 ) ;
#6203 = CARTESIAN_POINT ( 'NONE',  ( 0.000000000000000000, 0.000000000000000000, 900.0000000000000000 ) ) ;
#6204 = DIRECTION ( 'NONE',  ( 0.000000000000000000, 0.000000000000000000, 1.000000000000000000 ) ) ;
#6205 = ORIENTED_EDGE ( 'NONE', *, *, #7305, .T. ) ;
#6206 = CARTESIAN_POINT ( 'NONE',  ( -69.99999999999783995, 16.00000000000000000, 115.0000000000000142 ) ) ;
#6207 = EDGE_CURVE ( 'NONE', #8852, #13504, #37183, .T. ) ;
#6208 = CARTESIAN_POINT ( 'NONE',  ( 72.27890028733797578, 1.750000000000009548, -160.2068387089191219 ) ) ;
#6209 = ORIENTED_EDGE ( 'NONE', *, *, #24456, .T. ) ;
#6210 = DIRECTION ( 'NONE',  ( 1.000000000000000000, 0.000000000000000000, -4.625929269271584521E-16 ) ) ;
#6211 = DIRECTION ( 'NONE',  ( 1.000000000000000000, 0.000000000000000000, 0.000000000000000000 ) ) ;
#6212 = FACE_OUTER_BOUND ( 'NONE', #36170, .T. ) ;
#6213 = CARTESIAN_POINT ( 'NONE',  ( 195.0540265531851105, 2.143131898507880377E-16, 119.0682875569279702 ) ) ;
#6214 = CARTESIAN_POINT ( 'NONE',  ( 113.3040265531850537, 0.000000000000000000, 165.0000000000000000 ) ) ;
#6215 = VECTOR ( 'NONE', #33902, 1000.000000000000000 ) ;
#6216 = ORIENTED_EDGE ( 'NONE', *, *, #14706, .F. ) ;
#6217 = VERTEX_POINT ( 'NONE', #24605 ) ;
#6218 = DIRECTION ( 'NONE',  ( -0.000000000000000000, -0.000000000000000000, -1.000000000000000000 ) ) ;
#6219 = AXIS2_PLACEMENT_3D ( 'NONE', #17809, #45225, #33731 ) ;
#6220 = CARTESIAN_POINT ( 'NONE',  ( -46.69597344681494633, -1.750000000000010214, 40.81828755692798438 ) ) ;
#6221 = CARTESIAN_POINT ( 'NONE',  ( 113.3040265531850537, 0.000000000000000000, 165.0000000000000000 ) ) ;
#6222 = VECTOR ( 'NONE', #26300, 1000.000000000000000 ) ;
#6223 = LINE ( 'NONE', #32931, #45232 ) ;
#6224 = ORIENTED_EDGE ( 'NONE', *, *, #40094, .T. ) ;
#6225 = LINE ( 'NONE', #9311, #42226 ) ;
#6226 = VERTEX_POINT ( 'NONE', #36939 ) ;
#6227 = DIRECTION ( 'NONE',  ( 0.000000000000000000, 0.000000000000000000, -1.000000000000000000 ) ) ;
#6228 = VECTOR ( 'NONE', #30490, 1000.000000000000000 ) ;
#6229 = LINE ( 'NONE', #44438, #23600 ) ;
#6230 = CARTESIAN_POINT ( 'NONE',  ( -13.92102703536724384, -30.85732372859812500, 8.356839323120299312 ) ) ;
#6231 = CARTESIAN_POINT ( 'NONE',  ( 210.0000000000000568, 0.000000000000000000, -39.18171244307202983 ) ) ;
#6232 = DIRECTION ( 'NONE',  ( 0.000000000000000000, 0.000000000000000000, -1.000000000000000000 ) ) ;
#6233 = VECTOR ( 'NONE', #13657, 1000.000000000000000 ) ;
#6234 = CARTESIAN_POINT ( 'NONE',  ( -84.94597344681494633, 2.143131898507880377E-16, -157.4317124430720582 ) ) ;
#6235 = ORIENTED_EDGE ( 'NONE', *, *, #45914, .F. ) ;
#6236 = DIRECTION ( 'NONE',  ( 1.000000000000000000, 0.000000000000000000, 0.000000000000000000 ) ) ;
#6237 = FACE_OUTER_BOUND ( 'NONE', #15261, .T. ) ;
#6238 = CARTESIAN_POINT ( 'NONE',  ( 168.9999999999999716, 165.0000000000000000, 339.9999999999997726 ) ) ;
#6239 = EDGE_CURVE ( 'NONE', #47737, #21998, #46713, .T. ) ;
#6240 = AXIS2_PLACEMENT_3D ( 'NONE', #44222, #29351, #5991 ) ;
#6241 =( BOUNDED_CURVE ( )  B_SPLINE_CURVE ( 3, ( #29321, #25218, #44933, #40865 ),
 .UNSPECIFIED., .F., .F. ) 
 B_SPLINE_CURVE_WITH_KNOTS ( ( 4, 4 ),
 ( 4.712388980384689674, 6.283185307179586232 ),
 .UNSPECIFIED. ) 
 CURVE ( )  GEOMETRIC_REPRESENTATION_ITEM ( )  RATIONAL_B_SPLINE_CURVE ( ( 1.000000000000000000, 0.8047378541243649375, 0.8047378541243649375, 1.000000000000000000 ) ) 
 REPRESENTATION_ITEM ( '' )  );
#6242 = CARTESIAN_POINT ( 'NONE',  ( -126.6959734468149321, -1.749999999999996891, 0.8182875569279768335 ) ) ;
#6243 = ORIENTED_EDGE ( 'NONE', *, *, #45572, .T. ) ;
#6244 = PLANE ( 'NONE',  #7341 ) ;
#6245 = VERTEX_POINT ( 'NONE', #30728 ) ;
#6246 = CARTESIAN_POINT ( 'NONE',  ( -164.9999999999978400, 16.00000000000000000, 95.00000000000000000 ) ) ;
#6247 =( BOUNDED_CURVE ( )  B_SPLINE_CURVE ( 3, ( #32417, #48013, #12898, #34624 ),
 .UNSPECIFIED., .F., .F. ) 
 B_SPLINE_CURVE_WITH_KNOTS ( ( 4, 4 ),
 ( 4.712388980384689674, 6.283185307179586232 ),
 .UNSPECIFIED. ) 
 CURVE ( )  GEOMETRIC_REPRESENTATION_ITEM ( )  RATIONAL_B_SPLINE_CURVE ( ( 1.000000000000000000, 0.8047378541243649375, 0.8047378541243649375, 1.000000000000000000 ) ) 
 REPRESENTATION_ITEM ( '' )  );
#6248 = DIRECTION ( 'NONE',  ( -3.172065784643302499E-16, -1.000000000000000000, 2.537652627714642000E-15 ) ) ;
#6249 = CARTESIAN_POINT ( 'NONE',  ( -19.99999999999940670, 17.00000000000000000, -54.99999999999999289 ) ) ;
#6250 = AXIS2_PLACEMENT_3D ( 'NONE', #50502, #27210, #16411 ) ;
#6251 = EDGE_CURVE ( 'NONE', #13654, #27632, #9950, .T. ) ;
#6252 = EDGE_CURVE ( 'NONE', #14684, #45429, #21210, .T. ) ;
#6253 = AXIS2_PLACEMENT_3D ( 'NONE', #13574, #44106, #24638 ) ;
#6254 = DIRECTION ( 'NONE',  ( 0.000000000000000000, 0.000000000000000000, -1.000000000000000000 ) ) ;
#6255 = ORIENTED_EDGE ( 'NONE', *, *, #30709, .T. ) ;
#6256 = CARTESIAN_POINT ( 'NONE',  ( -207.7210997126620384, -1.750000000000009548, 41.84341382277508359 ) ) ;
#6257 = DIRECTION ( 'NONE',  ( 1.000000000000000000, 0.000000000000000000, -0.000000000000000000 ) ) ;
#6258 = CARTESIAN_POINT ( 'NONE',  ( 33.64889274059390090, -3.704246042440748621, 8.356839323120299312 ) ) ;
#6259 =( BOUNDED_CURVE ( )  B_SPLINE_CURVE ( 3, ( #21479, #24587, #41233, #13022 ),
 .UNSPECIFIED., .F., .F. ) 
 B_SPLINE_CURVE_WITH_KNOTS ( ( 4, 4 ),
 ( 0.000000000000000000, 1.570796326794896780 ),
 .UNSPECIFIED. ) 
 CURVE ( )  GEOMETRIC_REPRESENTATION_ITEM ( )  RATIONAL_B_SPLINE_CURVE ( ( 1.000000000000000000, 0.8047378541243649375, 0.8047378541243649375, 1.000000000000000000 ) ) 
 REPRESENTATION_ITEM ( '' )  );
#6260 = ORIENTED_EDGE ( 'NONE', *, *, #48354, .T. ) ;
#6261 = ORIENTED_EDGE ( 'NONE', *, *, #5765, .T. ) ;
#6262 = CARTESIAN_POINT ( 'NONE',  ( 85.00000000000152056, 16.00000000000000000, 35.00000000000000000 ) ) ;
#6263 = CARTESIAN_POINT ( 'NONE',  ( -0.3862712429686977478, 1.188820645368937390, -3.333333333333333481 ) ) ;
#6264 = EDGE_CURVE ( 'NONE', #4976, #14400, #22504, .T. ) ;
#6265 = EDGE_CURVE ( 'NONE', #18739, #15426, #6354, .T. ) ;
#6266 = AXIS2_PLACEMENT_3D ( 'NONE', #36389, #28170, #43800 ) ;
#6267 = ORIENTED_EDGE ( 'NONE', *, *, #34937, .T. ) ;
#6268 = B_SPLINE_CURVE_WITH_KNOTS ( 'NONE', 3,
 ( #22816, #14609, #30030, #3309 ),
 .UNSPECIFIED., .F., .F.,
 ( 4, 4 ),
 ( 0.8097120833243680593, 0.9322955464061821740 ),
 .UNSPECIFIED. ) ;
#6269 = ORIENTED_EDGE ( 'NONE', *, *, #42816, .F. ) ;
#6270 = CYLINDRICAL_SURFACE ( 'NONE', #31514, 2.000000000000001776 ) ;
#6271 = CARTESIAN_POINT ( 'NONE',  ( 15.00000000000000000, -46.01315789473684248, 5.916985404131816395 ) ) ;
#6272 = CARTESIAN_POINT ( 'NONE',  ( -86.69597344681494633, -1.750000000000010214, 40.81828755692798438 ) ) ;
#6273=STYLED_ITEM('',(#50747),#21989);
#6274 = ORIENTED_EDGE ( 'NONE', *, *, #28678, .T. ) ;
#6275 = DIRECTION ( 'NONE',  ( -0.000000000000000000, 0.000000000000000000, -1.000000000000000000 ) ) ;
#6276 = EDGE_CURVE ( 'NONE', #24192, #31155, #35261, .T. ) ;
#6277 = VERTEX_POINT ( 'NONE', #41506 ) ;
#6278 = CIRCLE ( 'NONE', #19373, 0.4999999999999995559 ) ;
#6279 = DIRECTION ( 'NONE',  ( -0.000000000000000000, -0.000000000000000000, -1.000000000000000000 ) ) ;
#6280 = CARTESIAN_POINT ( 'NONE',  ( -164.9999999999994031, 17.00000000000000000, -30.00000000000000000 ) ) ;
#6281 = ORIENTED_EDGE ( 'NONE', *, *, #167, .T. ) ;
#6282 = ORIENTED_EDGE ( 'NONE', *, *, #41178, .T. ) ;
#6283 = LINE ( 'NONE', #17566, #20203 ) ;
#6284 = ORIENTED_EDGE ( 'NONE', *, *, #47110, .T. ) ;
#6285 = CARTESIAN_POINT ( 'NONE',  ( -10.06660411345808193, 8.486842105263161073, -18.70408263333243326 ) ) ;
#6286 = B_SPLINE_CURVE_WITH_KNOTS ( 'NONE', 3,
 ( #46170, #3356, #11063, #26723 ),
 .UNSPECIFIED., .F., .F.,
 ( 4, 4 ),
 ( 2.278501876322824808E-17, 0.0004301978946275286349 ),
 .UNSPECIFIED. ) ;
#6287 = ORIENTED_EDGE ( 'NONE', *, *, #9924, .F. ) ;
#6288 = LINE ( 'NONE', #41164, #8621 ) ;
#6289 = SURFACE_STYLE_USAGE ( .BOTH. , #34243 ) ;
#6290 = VERTEX_POINT ( 'NONE', #33820 ) ;
#6291 = PLANE ( 'NONE',  #43059 ) ;
#6292 = CARTESIAN_POINT ( 'NONE',  ( 0.000000000000000000, 17.00000000000000000, 0.000000000000000000 ) ) ;
#6293 = LINE ( 'NONE', #40927, #15373 ) ;
#6294 = DIRECTION ( 'NONE',  ( 0.000000000000000000, 0.000000000000000000, -1.000000000000000000 ) ) ;
#6295 = CARTESIAN_POINT ( 'NONE',  ( -568.8466156985925863, -62.49999999999998579, -173.6910835022032700 ) ) ;
#6296 = ORIENTED_EDGE ( 'NONE', *, *, #12159, .F. ) ;
#6297 = CARTESIAN_POINT ( 'NONE',  ( -207.7210997126620384, -1.750000000000010214, -80.20683870891910772 ) ) ;
#6298 = CARTESIAN_POINT ( 'NONE',  ( 153.3040265531850537, -1.750000000000009992, 160.8182875569279702 ) ) ;
#6299 = DIRECTION ( 'NONE',  ( -0.000000000000000000, -0.000000000000000000, 1.000000000000000000 ) ) ;
#6300 = DIRECTION ( 'NONE',  ( 1.000000000000000000, 0.000000000000000000, 0.000000000000000000 ) ) ;
#6301 = ADVANCED_BREP_SHAPE_REPRESENTATION ( '', ( #5532, #45486 ), #38984 ) ;
#6302 = ADVANCED_FACE ( 'NONE', ( #49412 ), #37674, .F. ) ;
#6303 = CARTESIAN_POINT ( 'NONE',  ( 193.3040265531851105, 0.000000000000000000, 165.0000000000000000 ) ) ;
#6304 = DIRECTION ( 'NONE',  ( -1.000000000000000000, -0.000000000000000000, -0.000000000000000000 ) ) ;
#6305 = LINE ( 'NONE', #21945, #23718 ) ;
#6306 = DIRECTION ( 'NONE',  ( -0.000000000000000000, 1.000000000000000000, 0.000000000000000000 ) ) ;
#6307 = PLANE ( 'NONE',  #47557 ) ;
#6308 = AXIS2_PLACEMENT_3D ( 'NONE', #19441, #11251, #26887 ) ;
#6309 = VERTEX_POINT ( 'NONE', #29704 ) ;
#6310 = CARTESIAN_POINT ( 'NONE',  ( 6.604186672497970534, -1.848482776016330043, 9.753789706659947711 ) ) ;
#6311 = CARTESIAN_POINT ( 'NONE',  ( 0.3862712429686894766, -1.188820645368940276, 3.333333333333333481 ) ) ;
#6312 = CARTESIAN_POINT ( 'NONE',  ( -12.78770032058971395, -31.68259716188267916, 7.455576670931136185 ) ) ;
#6313 = CARTESIAN_POINT ( 'NONE',  ( 344.0000000000000000, -167.0000000000000853, -342.0000000000002842 ) ) ;
#6314 = CARTESIAN_POINT ( 'NONE',  ( -19.99999999999878142, 17.00000000000000000, 5.000000000000004441 ) ) ;
#6315 = ORIENTED_EDGE ( 'NONE', *, *, #12252, .T. ) ;
#6316 = ORIENTED_EDGE ( 'NONE', *, *, #12510, .F. ) ;
#6317 = FACE_OUTER_BOUND ( 'NONE', #44802, .T. ) ;
#6318 = FACE_OUTER_BOUND ( 'NONE', #7397, .T. ) ;
#6319 = VECTOR ( 'NONE', #44811, 1000.000000000000000 ) ;
#6320 = ORIENTED_EDGE ( 'NONE', *, *, #28791, .F. ) ;
#6321 = CARTESIAN_POINT ( 'NONE',  ( 7.576114424932982594, -50.00000000000000711, 7.906207997025717304 ) ) ;
#6322 = CYLINDRICAL_SURFACE ( 'NONE', #20833, 1.750000000000001554 ) ;
#6323 = ORIENTED_EDGE ( 'NONE', *, *, #35100, .T. ) ;
#6324 = EDGE_LOOP ( 'NONE', ( #40781, #39962, #3977, #41126, #30715 ) ) ;
#6325 = EDGE_CURVE ( 'NONE', #28214, #37651, #18397, .T. ) ;
#6326 = ORIENTED_EDGE ( 'NONE', *, *, #41178, .F. ) ;
#6327 = CARTESIAN_POINT ( 'NONE',  ( 4.999999999999999112, -175.0000000000000284, -350.0000000000002274 ) ) ;
#6328 = CARTESIAN_POINT ( 'NONE',  ( -126.6959734468149321, -1.749999999999996891, -159.1817124430720298 ) ) ;
#6329 = DIRECTION ( 'NONE',  ( -0.000000000000000000, -0.000000000000000000, -1.000000000000000000 ) ) ;
#6330 = VERTEX_POINT ( 'NONE', #49900 ) ;
#6331 = CARTESIAN_POINT ( 'NONE',  ( -6.695973446814940111, 1.750000000000023315, -159.1817124430720298 ) ) ;
#6332 = VERTEX_POINT ( 'NONE', #30206 ) ;
#6333 =( BOUNDED_CURVE ( )  B_SPLINE_CURVE ( 3, ( #23324, #49964, #46120, #38494 ),
 .UNSPECIFIED., .F., .F. ) 
 B_SPLINE_CURVE_WITH_KNOTS ( ( 4, 4 ),
 ( 0.000000000000000000, 1.570796326794896558 ),
 .UNSPECIFIED. ) 
 CURVE ( )  GEOMETRIC_REPRESENTATION_ITEM ( )  RATIONAL_B_SPLINE_CURVE ( ( 1.000000000000000000, 0.8047378541243649375, 0.8047378541243649375, 1.000000000000000000 ) ) 
 REPRESENTATION_ITEM ( '' )  );
#6334 = ORIENTED_EDGE ( 'NONE', *, *, #4346, .F. ) ;
#6335 = LINE ( 'NONE', #29936, #13914 ) ;
#6336 = FACE_OUTER_BOUND ( 'NONE', #25061, .T. ) ;
#6337 = LINE ( 'NONE', #49875, #38985 ) ;
#6338 = ORIENTED_EDGE ( 'NONE', *, *, #3266, .T. ) ;
#6339 = LINE ( 'NONE', #26084, #13505 ) ;
#6340 = FILL_AREA_STYLE_COLOUR ( '', #10035 ) ;
#6341 = CARTESIAN_POINT ( 'NONE',  ( 210.0000000000000568, 0.000000000000000000, 40.81828755692798438 ) ) ;
#6342 = CARTESIAN_POINT ( 'NONE',  ( -87.72109971266203843, 1.750000000000009326, -158.1565861772249377 ) ) ;
#6343 = DIRECTION ( 'NONE',  ( -1.000000000000000000, -0.000000000000000000, -0.000000000000000000 ) ) ;
#6344 = CARTESIAN_POINT ( 'NONE',  ( 111.5540265531850679, 0.000000000000000000, -165.0000000000000000 ) ) ;
#6345 = CARTESIAN_POINT ( 'NONE',  ( -166.6959734468149463, -1.750000000000010214, -39.18171244307202983 ) ) ;
#6346 = CARTESIAN_POINT ( 'NONE',  ( 181.0000000000000000, -77.49999999999997158, -340.0000000000001137 ) ) ;
#6347 = FACE_OUTER_BOUND ( 'NONE', #20153, .T. ) ;
#6348 = CARTESIAN_POINT ( 'NONE',  ( -5.670847180967843570, 1.750000000000022871, 1.843413822775074040 ) ) ;
#6349 = VECTOR ( 'NONE', #9627, 1000.000000000000000 ) ;
#6350 = CARTESIAN_POINT ( 'NONE',  ( 113.3040265531850537, -1.749999999999996891, 160.8182875569279702 ) ) ;
#6351 = ORIENTED_EDGE ( 'NONE', *, *, #3536, .T. ) ;
#6352 = DIRECTION ( 'NONE',  ( 0.000000000000000000, 0.000000000000000000, 1.000000000000000000 ) ) ;
#6353 = CARTESIAN_POINT ( 'NONE',  ( 350.0000000000001137, 185.0000000000000284, 355.9999999999997726 ) ) ;
#6354 = LINE ( 'NONE', #14038, #49156 ) ;
#6355 = EDGE_LOOP ( 'NONE', ( #39831, #22422, #27160, #1592, #50379, #22645 ) ) ;
#6356 = DIRECTION ( 'NONE',  ( -1.121065046350011585E-16, -0.7071067811865475727, -0.7071067811865474617 ) ) ;
#6357 = ORIENTED_EDGE ( 'NONE', *, *, #47916, .T. ) ;
#6358 = CARTESIAN_POINT ( 'NONE',  ( 112.2789002873379758, 1.749999999999996669, 161.8434138227750907 ) ) ;
#6359 = FACE_BOUND ( 'NONE', #46768, .T. ) ;
#6360 = DIRECTION ( 'NONE',  ( 1.000000000000000000, 0.000000000000000000, 0.000000000000000000 ) ) ;
#6361 = CARTESIAN_POINT ( 'NONE',  ( 191.5540265531850537, 1.025126265847089435, 122.5682875569280128 ) ) ;
#6362 = VERTEX_POINT ( 'NONE', #34575 ) ;
#6363 = PLANE ( 'NONE',  #13444 ) ;
#6364 = ORIENTED_EDGE ( 'NONE', *, *, #1664, .T. ) ;
#6365 = ORIENTED_EDGE ( 'NONE', *, *, #486, .F. ) ;
#6366 = CARTESIAN_POINT ( 'NONE',  ( -10.00000000000003375, 8.486842105263161073, 18.38522261288946780 ) ) ;
#6367 = EDGE_CURVE ( 'NONE', #44970, #37221, #259, .T. ) ;
#6368 = ORIENTED_EDGE ( 'NONE', *, *, #17586, .T. ) ;
#6369 = PLANE ( 'NONE',  #21284 ) ;
#6370 = CARTESIAN_POINT ( 'NONE',  ( -34.08355720199904226, 2.371364769369340042, 7.455576670931136185 ) ) ;
#6371 = FACE_BOUND ( 'NONE', #19739, .T. ) ;
#6372 = EDGE_CURVE ( 'NONE', #42683, #19177, #49157, .T. ) ;
#6373 = CYLINDRICAL_SURFACE ( 'NONE', #50106, 1.750000000000008438 ) ;
#6374 = CARTESIAN_POINT ( 'NONE',  ( 3.951902928218917754, 0.4322042478607662219, 3.247139300358769631 ) ) ;
#6375 = VERTEX_POINT ( 'NONE', #25608 ) ;
#6376 = EDGE_CURVE ( 'NONE', #8986, #14100, #49662, .T. ) ;
#6377 = CARTESIAN_POINT ( 'NONE',  ( 181.0000000000000000, 165.0000000000000000, -344.0000000000001137 ) ) ;
#6378 = CARTESIAN_POINT ( 'NONE',  ( 183.0000000000000000, -272.4999999999999432, -343.9999999999994316 ) ) ;
#6379 = EDGE_CURVE ( 'NONE', #29467, #16943, #26099, .T. ) ;
#6380 = LINE ( 'NONE', #29734, #33269 ) ;
#6381 =( BOUNDED_CURVE ( )  B_SPLINE_CURVE ( 3, ( #12085, #44117, #23883, #24649 ),
 .UNSPECIFIED., .F., .F. ) 
 B_SPLINE_CURVE_WITH_KNOTS ( ( 4, 4 ),
 ( 3.141592653589793116, 4.712388980384689674 ),
 .UNSPECIFIED. ) 
 CURVE ( )  GEOMETRIC_REPRESENTATION_ITEM ( )  RATIONAL_B_SPLINE_CURVE ( ( 1.000000000000000000, 0.8047378541243649375, 0.8047378541243649375, 1.000000000000000000 ) ) 
 REPRESENTATION_ITEM ( '' )  );
#6382 = EDGE_LOOP ( 'NONE', ( #10105, #18619, #25690 ) ) ;
#6383 = AXIS2_PLACEMENT_3D ( 'NONE', #3366, #33932, #42368 ) ;
#6384 = DIRECTION ( 'NONE',  ( -1.000000000000000000, 0.000000000000000000, 0.000000000000000000 ) ) ;
#6385 = DIRECTION ( 'NONE',  ( -1.000000000000000000, 0.000000000000000000, 0.000000000000000000 ) ) ;
#6386 = ORIENTED_EDGE ( 'NONE', *, *, #27321, .F. ) ;
#6387 = ORIENTED_EDGE ( 'NONE', *, *, #14417, .F. ) ;
#6388 = ORIENTED_EDGE ( 'NONE', *, *, #49052, .F. ) ;
#6389 = DIRECTION ( 'NONE',  ( 1.000000000000000000, 0.000000000000000000, 0.000000000000000000 ) ) ;
#6390 =( BOUNDED_CURVE ( )  B_SPLINE_CURVE ( 3, ( #36694, #32828, #520, #43593 ),
 .UNSPECIFIED., .F., .F. ) 
 B_SPLINE_CURVE_WITH_KNOTS ( ( 4, 4 ),
 ( 4.712388980384689674, 6.283185307179586232 ),
 .UNSPECIFIED. ) 
 CURVE ( )  GEOMETRIC_REPRESENTATION_ITEM ( )  RATIONAL_B_SPLINE_CURVE ( ( 1.000000000000000000, 0.8047378541243649375, 0.8047378541243649375, 1.000000000000000000 ) ) 
 REPRESENTATION_ITEM ( '' )  );
#6391 = DIRECTION ( 'NONE',  ( -0.000000000000000000, -0.000000000000000000, -1.000000000000000000 ) ) ;
#6392 = ORIENTED_EDGE ( 'NONE', *, *, #762, .T. ) ;
#6393 = CARTESIAN_POINT ( 'NONE',  ( 75.05402655318509630, 2.143131898507880377E-16, 122.5682875569279844 ) ) ;
#6394 = CARTESIAN_POINT ( 'NONE',  ( 1.035950918207909632, 33.23661552194049307, -2.408242355805840784 ) ) ;
#6395 = FACE_BOUND ( 'NONE', #44191, .T. ) ;
#6396 = ORIENTED_EDGE ( 'NONE', *, *, #41535, .T. ) ;
#6397 = CARTESIAN_POINT ( 'NONE',  ( 25.40454589245968364, 27.58367357691700406, -8.192531242611265085 ) ) ;
#6398 = CARTESIAN_POINT ( 'NONE',  ( -1.011271242968677875, -0.7347315653656004697, -3.333333333333333481 ) ) ;
#6399 = DIRECTION ( 'NONE',  ( -1.000000000000000000, -0.000000000000000000, -0.000000000000000000 ) ) ;
#6400 = EDGE_CURVE ( 'NONE', #37393, #3284, #45322, .T. ) ;
#6401 = EDGE_CURVE ( 'NONE', #22572, #4058, #5479, .T. ) ;
#6402 = ORIENTED_EDGE ( 'NONE', *, *, #18737, .T. ) ;
#6403 = DIRECTION ( 'NONE',  ( -0.7233555441435720601, -0.6904757466825006684, 0.000000000000000000 ) ) ;
#6404 = LINE ( 'NONE', #37731, #2120 ) ;
#6405 = ADVANCED_FACE ( 'NONE', ( #45815, #10703 ), #14297, .F. ) ;
#6406 = EDGE_CURVE ( 'NONE', #3893, #16542, #2785, .T. ) ;
#6407 = DIRECTION ( 'NONE',  ( 1.000000000000000000, 0.000000000000000000, 0.000000000000000000 ) ) ;
#6408 = CARTESIAN_POINT ( 'NONE',  ( 349.9999999999999432, -168.9999999999999432, 343.9999999999997726 ) ) ;
#6409 = ORIENTED_EDGE ( 'NONE', *, *, #44460, .F. ) ;
#6410 = EDGE_CURVE ( 'NONE', #26079, #14709, #31736, .T. ) ;
#6411 = CARTESIAN_POINT ( 'NONE',  ( 28.05568344207340203, 30.90646677863635716, -8.080361901872242569 ) ) ;
#6412 = CARTESIAN_POINT ( 'NONE',  ( -205.6708471809678827, 1.750000000000010214, 81.84341382277507648 ) ) ;
#6413 = EDGE_CURVE ( 'NONE', #33857, #20200, #47080, .T. ) ;
#6414 = CARTESIAN_POINT ( 'NONE',  ( 113.3040265531850537, 0.000000000000000000, 165.0000000000000000 ) ) ;
#6415 = CARTESIAN_POINT ( 'NONE',  ( 35.00000000000216716, 17.00000000000000000, 95.00000000000000000 ) ) ;
#6416 = DIRECTION ( 'NONE',  ( 0.000000000000000000, 0.000000000000000000, -1.000000000000000000 ) ) ;
#6417 = ORIENTED_EDGE ( 'NONE', *, *, #16790, .T. ) ;
#6418 = CARTESIAN_POINT ( 'NONE',  ( 80.00000000000186162, 17.00000000000000000, 65.00000000000000000 ) ) ;
#6419 = B_SPLINE_CURVE_WITH_KNOTS ( 'NONE', 3,
 ( #16994, #1100, #13384, #47741 ),
 .UNSPECIFIED., .F., .F.,
 ( 4, 4 ),
 ( 0.001152428489661398063, 0.001623376834731057655 ),
 .UNSPECIFIED. ) ;
#6420 = ORIENTED_EDGE ( 'NONE', *, *, #1090, .T. ) ;
#6421 = DIRECTION ( 'NONE',  ( -0.000000000000000000, -0.000000000000000000, -1.000000000000000000 ) ) ;
#6422 = ORIENTED_EDGE ( 'NONE', *, *, #44926, .T. ) ;
#6423 = DIRECTION ( 'NONE',  ( -1.000000000000000000, -0.000000000000000000, -0.000000000000000000 ) ) ;
#6424 = CARTESIAN_POINT ( 'NONE',  ( 35.05402655318504657, 1.025126265847089657, -80.93171244307201562 ) ) ;
#6425 = CARTESIAN_POINT ( 'NONE',  ( 0.000000000000000000, 165.0000000000000000, 343.9999999999997726 ) ) ;
#6426 = ADVANCED_FACE ( 'NONE', ( #7629 ), #43272, .T. ) ;
#6427 = ORIENTED_EDGE ( 'NONE', *, *, #30634, .F. ) ;
#6428 = EDGE_CURVE ( 'NONE', #7894, #36027, #35357, .T. ) ;
#6429 = EDGE_CURVE ( 'NONE', #39174, #10463, #40159, .T. ) ;
#6430 = CARTESIAN_POINT ( 'NONE',  ( -23.83799721022572982, 28.99517291086380411, 3.209567239418972040 ) ) ;
#6431 = EDGE_CURVE ( 'NONE', #323, #12448, #34527, .T. ) ;
#6432 = EDGE_LOOP ( 'NONE', ( #13371, #27149, #26578, #334, #24816, #23393, #40631, #49460, #28788, #30289, #4792, #3098 ) ) ;
#6433 = DIRECTION ( 'NONE',  ( -1.586032892321652236E-16, -1.000000000000000000, -6.853681917100419162E-49 ) ) ;
#6434 = CARTESIAN_POINT ( 'NONE',  ( -7.721099712662037540, 1.750000000000023315, 41.84341382277508359 ) ) ;
#6435 = CARTESIAN_POINT ( 'NONE',  ( -24.47767542868268364, 23.18653802921800278, 8.807470649214879543 ) ) ;
#6436 = DIRECTION ( 'NONE',  ( -1.000000000000000000, 0.000000000000000000, -1.612977847700450206E-50 ) ) ;
#6437 = VERTEX_POINT ( 'NONE', #23783 ) ;
#6438 = ORIENTED_EDGE ( 'NONE', *, *, #26362, .F. ) ;
#6439 = CARTESIAN_POINT ( 'NONE',  ( 192.2789002873380184, 1.750000000000009548, 159.7931612910809065 ) ) ;
#6440 = EDGE_CURVE ( 'NONE', #13303, #25392, #15576, .T. ) ;
#6441 = ORIENTED_EDGE ( 'NONE', *, *, #47534, .F. ) ;
#6442 = CARTESIAN_POINT ( 'NONE',  ( 36.63544619771723632, 20.34968343020639381, 7.544061037322998153 ) ) ;
#6443 = VERTEX_POINT ( 'NONE', #46577 ) ;
#6444 = CARTESIAN_POINT ( 'NONE',  ( 358.0000000000000568, 165.0000000000000000, -94.00000000000019895 ) ) ;
#6445 = EDGE_CURVE ( 'NONE', #30975, #907, #23536, .T. ) ;
#6446 = CARTESIAN_POINT ( 'NONE',  ( 210.0000000000000568, 0.000000000000000000, 82.56828755692799859 ) ) ;
#6447 = ORIENTED_EDGE ( 'NONE', *, *, #36855, .T. ) ;
#6448 = FACE_OUTER_BOUND ( 'NONE', #48613, .T. ) ;
#6449 = CIRCLE ( 'NONE', #23674, 2.000000000000001776 ) ;
#6450 = DIRECTION ( 'NONE',  ( -1.000000000000000000, -0.000000000000000000, -0.000000000000000000 ) ) ;
#6451 = CARTESIAN_POINT ( 'NONE',  ( 195.9526953830863079, -154.8119894309599260, 472.8425600500171981 ) ) ;
#6452 = CARTESIAN_POINT ( 'NONE',  ( 339.9999999999998863, -169.0000000000001137, -349.9999999999998863 ) ) ;
#6453 = ORIENTED_EDGE ( 'NONE', *, *, #12047, .T. ) ;
#6454 = EDGE_CURVE ( 'NONE', #34191, #20388, #50423, .T. ) ;
#6455 = ORIENTED_EDGE ( 'NONE', *, *, #28927, .T. ) ;
#6456 = CARTESIAN_POINT ( 'NONE',  ( 30.21887974406487487, -14.69854701517530060, -8.016098858316199838 ) ) ;
#6457 = DIRECTION ( 'NONE',  ( -7.793956916774525800E-48, 0.000000000000000000, 1.000000000000000000 ) ) ;
#6458 = CLOSED_SHELL ( 'NONE', ( #38372, #1640, #27091, #34780, #41572, #37608, #26824, #41481, #37992, #39997, #2994, #13611, #15526, #36867, #39329, #19306, #24177, #43835 ) ) ;
#6459 = ORIENTED_EDGE ( 'NONE', *, *, #46034, .T. ) ;
#6460 = LINE ( 'NONE', #29064, #29924 ) ;
#6461 = ORIENTED_EDGE ( 'NONE', *, *, #34919, .T. ) ;
#6463 = LINE ( 'NONE', #18512, #39258 ) ;
#6462 = VECTOR ( 'NONE', #11614, 1000.000000000000000 ) ;
#6464 = LINE ( 'NONE', #41621, #5576 ) ;
#6465 = CARTESIAN_POINT ( 'NONE',  ( 177.5000000000000284, 112.5000000000000000, -10.00000000000000000 ) ) ;
#6466 = EDGE_CURVE ( 'NONE', #15741, #13767, #11470, .T. ) ;
#6467 = EDGE_CURVE ( 'NONE', #34142, #43723, #35605, .T. ) ;
#6468 = DIRECTION ( 'NONE',  ( 0.000000000000000000, 0.000000000000000000, -1.000000000000000000 ) ) ;
#6469 = LINE ( 'NONE', #22125, #18389 ) ;
#6470 = CARTESIAN_POINT ( 'NONE',  ( 73.30402655318508209, 0.000000000000000000, 165.0000000000000000 ) ) ;
#6471 = ORIENTED_EDGE ( 'NONE', *, *, #33956, .T. ) ;
#6472 = CARTESIAN_POINT ( 'NONE',  ( -7.721099712662037540, -1.750000000000023315, 39.79316129108089228 ) ) ;
#6473 = EDGE_CURVE ( 'NONE', #29314, #11997, #2195, .T. ) ;
#6474 = B_SPLINE_SURFACE_WITH_KNOTS ( 'NONE', 3, 3, ( 
 ( #35743, #31632, #12604, #7770 ),
 ( #46711, #11863, #35224, #36237 ),
 ( #31880, #1074, #28272, #39321 ),
 ( #27262, #4414, #8268, #42887 ) ),
 .UNSPECIFIED., .F., .F., .F.,
 ( 4, 4 ),
 ( 4, 4 ),
 ( 0.000000000000000000, 1.000000000000000000 ),
 ( 0.000000000000000000, 1.000000000000000000 ),
 .UNSPECIFIED. ) ;
#6475 = CARTESIAN_POINT ( 'NONE',  ( -210.0000000000000568, 0.000000000000000000, 82.56828755692799859 ) ) ;
#6476 = CARTESIAN_POINT ( 'NONE',  ( 0.9989200098981507736, 1.123829893718967687, 9.927319414211233095 ) ) ;
#6477 = EDGE_CURVE ( 'NONE', #12217, #38289, #12228, .T. ) ;
#6478 = CARTESIAN_POINT ( 'NONE',  ( -0.1287570809895576818, -0.3962735484563154609, 10.00000000000000000 ) ) ;
#6479 = EDGE_LOOP ( 'NONE', ( #33213, #35563, #27771, #2612 ) ) ;
#6480 = FACE_OUTER_BOUND ( 'NONE', #49849, .T. ) ;
#6481 = ORIENTED_EDGE ( 'NONE', *, *, #30533, .T. ) ;
#6482 = DIRECTION ( 'NONE',  ( -0.000000000000000000, -1.000000000000000000, -0.000000000000000000 ) ) ;
#6483 = CARTESIAN_POINT ( 'NONE',  ( 210.0000000000000568, 2.143131898507881116E-16, -40.93171244307203693 ) ) ;
#6484 = EDGE_CURVE ( 'NONE', #36910, #30921, #39531, .T. ) ;
#6485 = DIRECTION ( 'NONE',  ( 1.000000000000000000, 0.000000000000000000, 0.000000000000000000 ) ) ;
#6486 = ORIENTED_EDGE ( 'NONE', *, *, #43350, .F. ) ;
#6487 = AXIS2_PLACEMENT_3D ( 'NONE', #3897, #47218, #19798 ) ;
#6488 = AXIS2_PLACEMENT_3D ( 'NONE', #44453, #631, #32680 ) ;
#6489 = EDGE_CURVE ( 'NONE', #40379, #30326, #41958, .T. ) ;
#6490 = DIRECTION ( 'NONE',  ( -1.000000000000000000, 0.000000000000000000, 0.000000000000000000 ) ) ;
#6491 = ORIENTED_EDGE ( 'NONE', *, *, #6700, .T. ) ;
#6492 = CARTESIAN_POINT ( 'NONE',  ( -46.69597344681494633, 1.750000000000010214, 40.81828755692798438 ) ) ;
#6493 = DIRECTION ( 'NONE',  ( 1.000000000000000000, 0.000000000000000000, 0.000000000000000000 ) ) ;
#6494 = VECTOR ( 'NONE', #37963, 1000.000000000000000 ) ;
#6495 = CYLINDRICAL_SURFACE ( 'NONE', #470, 1.750000000000001554 ) ;
#6496 = ORIENTED_EDGE ( 'NONE', *, *, #47690, .F. ) ;
#6497 = ORIENTED_EDGE ( 'NONE', *, *, #34401, .F. ) ;
#6498 = CARTESIAN_POINT ( 'NONE',  ( -28.05568344207363296, -30.90646677863614045, -8.080361901872242569 ) ) ;
#6499 = LINE ( 'NONE', #22157, #23032 ) ;
#6500 = CIRCLE ( 'NONE', #38504, 1.750000000000015543 ) ;
#6501 = ORIENTED_EDGE ( 'NONE', *, *, #39050, .T. ) ;
#6502 = ORIENTED_EDGE ( 'NONE', *, *, #21794, .T. ) ;
#6503 = CARTESIAN_POINT ( 'NONE',  ( -0.2773062244624664441, 1.251557370488897813, 9.948547179989621014 ) ) ;
#6504 = CARTESIAN_POINT ( 'NONE',  ( 80.00000000000122213, 17.00000000000000000, 5.000000000000004441 ) ) ;
#6505 = CARTESIAN_POINT ( 'NONE',  ( 1.040834085586084257E-14, -6.912230148066169200, 5.000000000000000000 ) ) ;
#6506 = ORIENTED_EDGE ( 'NONE', *, *, #44322, .T. ) ;
#6507 = CARTESIAN_POINT ( 'NONE',  ( -0.9989200098981521059, -1.123829893718962802, 9.927319414211225990 ) ) ;
#6508 = VERTEX_POINT ( 'NONE', #27380 ) ;
#6509 = B_SPLINE_CURVE_WITH_KNOTS ( 'NONE', 3,
 ( #28239, #12081, #27726, #16429 ),
 .UNSPECIFIED., .F., .F.,
 ( 4, 4 ),
 ( 0.000000000000000000, 0.002458791966311101550 ),
 .UNSPECIFIED. ) ;
#6510 = PLANE ( 'NONE',  #6219 ) ;
#6511 = LINE ( 'NONE', #6280, #5236 ) ;
#6512 = B_SPLINE_CURVE_WITH_KNOTS ( 'NONE', 3,
 ( #8907, #1226, #37585, #14714 ),
 .UNSPECIFIED., .F., .F.,
 ( 4, 4 ),
 ( 0.7998230999345288250, 0.9869080488566185361 ),
 .UNSPECIFIED. ) ;
#6513 = ORIENTED_EDGE ( 'NONE', *, *, #36875, .F. ) ;
#6514 = EDGE_LOOP ( 'NONE', ( #6875, #26279, #37179, #8431 ) ) ;
#6515 = CARTESIAN_POINT ( 'NONE',  ( -1.104477492316108256, -0.6506302558160915739, 9.957892297621011579 ) ) ;
#6516 = CARTESIAN_POINT ( 'NONE',  ( -14.49999999999999822, 12.87566193687862715, -19.86060803177194956 ) ) ;
#6517 = EDGE_LOOP ( 'NONE', ( #2795, #32012, #44075 ) ) ;
#6518 = LINE ( 'NONE', #36668, #14947 ) ;
#6520 = ORIENTED_EDGE ( 'NONE', *, *, #7095, .T. ) ;
#6519 = VECTOR ( 'NONE', #7968, 1000.000000000000000 ) ;
#6521 = LINE ( 'NONE', #25779, #30742 ) ;
#6522 =( LENGTH_UNIT ( ) NAMED_UNIT ( * ) SI_UNIT ( .MILLI., .METRE. ) );
#6524 = ORIENTED_EDGE ( 'NONE', *, *, #40567, .F. ) ;
#6523 = AXIS2_PLACEMENT_3D ( 'NONE', #27643, #10964, #3502 ) ;
#6525 = DIRECTION ( 'NONE',  ( -1.000000000000000000, 0.000000000000000000, 0.000000000000000000 ) ) ;
#6526 =( BOUNDED_CURVE ( )  B_SPLINE_CURVE ( 3, ( #24299, #12966, #31996, #40187 ),
 .UNSPECIFIED., .F., .F. ) 
 B_SPLINE_CURVE_WITH_KNOTS ( ( 4, 4 ),
 ( 4.712388980384689674, 6.283185307179586232 ),
 .UNSPECIFIED. ) 
 CURVE ( )  GEOMETRIC_REPRESENTATION_ITEM ( )  RATIONAL_B_SPLINE_CURVE ( ( 1.000000000000000000, 0.8047378541243649375, 0.8047378541243649375, 1.000000000000000000 ) ) 
 REPRESENTATION_ITEM ( '' )  );
#6527 = LINE ( 'NONE', #32995, #48928 ) ;
#6528 = DIRECTION ( 'NONE',  ( 0.000000000000000000, 1.000000000000000000, 0.000000000000000000 ) ) ;
#6529 = EDGE_CURVE ( 'NONE', #6375, #36250, #12673, .T. ) ;
#6530 = AXIS2_PLACEMENT_3D ( 'NONE', #50614, #15762, #11667 ) ;
#6531 = EDGE_CURVE ( 'NONE', #25811, #35155, #15658, .T. ) ;
#6532 = PLANE ( 'NONE',  #9395 ) ;
#6533 = ORIENTED_EDGE ( 'NONE', *, *, #10801, .T. ) ;
#6535 = CIRCLE ( 'NONE', #8198, 4.000000000000003553 ) ;
#6534 = CARTESIAN_POINT ( 'NONE',  ( -19.99999999999908695, 16.00000000000000000, 0.000000000000000000 ) ) ;
#6536 =( BOUNDED_CURVE ( )  B_SPLINE_CURVE ( 3, ( #31078, #4640, #35953, #11319 ),
 .UNSPECIFIED., .F., .F. ) 
 B_SPLINE_CURVE_WITH_KNOTS ( ( 4, 4 ),
 ( 0.000000000000000000, 1.570796326794896558 ),
 .UNSPECIFIED. ) 
 CURVE ( )  GEOMETRIC_REPRESENTATION_ITEM ( )  RATIONAL_B_SPLINE_CURVE ( ( 1.000000000000000000, 0.8047378541243649375, 0.8047378541243649375, 1.000000000000000000 ) ) 
 REPRESENTATION_ITEM ( '' )  );
#6537 = CARTESIAN_POINT ( 'NONE',  ( 75.05402655318509630, 2.143131898507880377E-16, 165.0000000000000000 ) ) ;
#6538 = EDGE_CURVE ( 'NONE', #17655, #34173, #20941, .T. ) ;
#6539 = DIRECTION ( 'NONE',  ( 0.000000000000000000, 0.000000000000000000, 1.000000000000000000 ) ) ;
#6540 = LINE ( 'NONE', #30925, #19199 ) ;
#6541 = EDGE_CURVE ( 'NONE', #10961, #405, #13484, .T. ) ;
#6542 = EDGE_CURVE ( 'NONE', #38070, #5777, #44130, .T. ) ;
#6543 = AXIS2_PLACEMENT_3D ( 'NONE', #40334, #838, #35755 ) ;
#6544 = LINE ( 'NONE', #41440, #1080 ) ;
#6545 = LINE ( 'NONE', #45758, #28590 ) ;
#6546 = LINE ( 'NONE', #22201, #17979 ) ;
#6547 = CARTESIAN_POINT ( 'NONE',  ( 10.00419011302945904, 8.486842105263161073, -18.42339408367723053 ) ) ;
#6548 = EDGE_CURVE ( 'NONE', #27522, #37293, #44018, .T. ) ;
#6549 =( BOUNDED_CURVE ( )  B_SPLINE_CURVE ( 3, ( #45233, #1924, #10116, #41671 ),
 .UNSPECIFIED., .F., .F. ) 
 B_SPLINE_CURVE_WITH_KNOTS ( ( 4, 4 ),
 ( 0.000000000000000000, 1.570796326794896780 ),
 .UNSPECIFIED. ) 
 CURVE ( )  GEOMETRIC_REPRESENTATION_ITEM ( )  RATIONAL_B_SPLINE_CURVE ( ( 1.000000000000000000, 0.8047378541243649375, 0.8047378541243649375, 1.000000000000000000 ) ) 
 REPRESENTATION_ITEM ( '' )  );
#6550 = DIRECTION ( 'NONE',  ( 0.000000000000000000, 1.000000000000000000, 6.123233995736766036E-17 ) ) ;
#6551 = ORIENTED_EDGE ( 'NONE', *, *, #5031, .F. ) ;
#6552 = CARTESIAN_POINT ( 'NONE',  ( 22.75063655912441973, 24.61040335498486442, -8.466730184410787174 ) ) ;
#6553 = CARTESIAN_POINT ( 'NONE',  ( -32.43949840348904701, -7.871562655726274116, -9.367992836599954742 ) ) ;
#6554 = DIRECTION ( 'NONE',  ( -1.000000000000000000, -0.000000000000000000, -0.000000000000000000 ) ) ;
#6555 = CARTESIAN_POINT ( 'NONE',  ( -205.6708471809678827, -1.750000000000009548, -160.2068387089191219 ) ) ;
#6556 = CARTESIAN_POINT ( 'NONE',  ( -119.9999999999984652, 17.00000000000000000, 35.00000000000000000 ) ) ;
#6557 = VERTEX_POINT ( 'NONE', #28892 ) ;
#6558 = ORIENTED_EDGE ( 'NONE', *, *, #20803, .T. ) ;
#6559 = VECTOR ( 'NONE', #20961, 1000.000000000000000 ) ;
#6560 = DIRECTION ( 'NONE',  ( 1.000000000000000000, 1.156482317317870492E-16, -0.000000000000000000 ) ) ;
#6561 = CARTESIAN_POINT ( 'NONE',  ( -44.94597344681493922, 2.143131898507880377E-16, 165.0000000000000000 ) ) ;
#6562 = VECTOR ( 'NONE', #37876, 1000.000000000000000 ) ;
#6563 = AXIS2_PLACEMENT_3D ( 'NONE', #30667, #27319, #36045 ) ;
#6564 = ORIENTED_EDGE ( 'NONE', *, *, #47449, .T. ) ;
#6565 = CARTESIAN_POINT ( 'NONE',  ( -44.94597344681497475, 0.000000000000000000, 162.5682875569279702 ) ) ;
#6566 = CARTESIAN_POINT ( 'NONE',  ( -206.6959734468149463, 1.750000000000010658, -119.1817124430720440 ) ) ;
#6567 = EDGE_LOOP ( 'NONE', ( #3903, #8809, #39078, #40618 ) ) ;
#6568 = ORIENTED_EDGE ( 'NONE', *, *, #48132, .F. ) ;
#6569 = VECTOR ( 'NONE', #23296, 1000.000000000000000 ) ;
#6570 = B_SPLINE_CURVE_WITH_KNOTS ( 'NONE', 3,
 ( #31205, #18860, #23227, #11689 ),
 .UNSPECIFIED., .F., .F.,
 ( 4, 4 ),
 ( 0.0002936521407521901629, 0.0006663369986142733160 ),
 .UNSPECIFIED. ) ;
#6571 = EDGE_LOOP ( 'NONE', ( #6023, #6420, #8362, #30515 ) ) ;
#6572 = EDGE_CURVE ( 'NONE', #24636, #4376, #47472, .T. ) ;
#6573 = CARTESIAN_POINT ( 'NONE',  ( -205.6708471809678827, 1.750000000000009548, -38.15658617722494483 ) ) ;
#6574 = CARTESIAN_POINT ( 'NONE',  ( -88.44597344681497475, 0.000000000000000000, 2.568287556928006143 ) ) ;
#6575 = DIRECTION ( 'NONE',  ( -0.000000000000000000, -0.000000000000000000, -1.000000000000000000 ) ) ;
#6576 = VECTOR ( 'NONE', #772, 1000.000000000000000 ) ;
#6577 = ORIENTED_EDGE ( 'NONE', *, *, #46007, .F. ) ;
#6578 = CARTESIAN_POINT ( 'NONE',  ( 168.9999999999999716, 165.0000000000000000, -342.0000000000001137 ) ) ;
#6579 = DIRECTION ( 'NONE',  ( -1.942330104924128867E-32, 0.000000000000000000, -1.000000000000000000 ) ) ;
#6580 = CARTESIAN_POINT ( 'NONE',  ( -48.44597344681496054, -1.025126265847089879, -117.4317124430720156 ) ) ;
#6581 = VERTEX_POINT ( 'NONE', #16588 ) ;
#6582 = EDGE_LOOP ( 'NONE', ( #11865, #7339, #43736, #19141, #27309, #25903, #22286, #4232 ) ) ;
#6583 = LINE ( 'NONE', #22234, #39382 ) ;
#6584 = DIRECTION ( 'NONE',  ( -0.000000000000000000, 0.000000000000000000, -1.000000000000000000 ) ) ;
#6585 = DIRECTION ( 'NONE',  ( 0.000000000000000000, 0.000000000000000000, -1.000000000000000000 ) ) ;
#6586 = ORIENTED_EDGE ( 'NONE', *, *, #2849, .F. ) ;
#6587 = DIRECTION ( 'NONE',  ( -0.000000000000000000, -0.000000000000000000, -1.000000000000000000 ) ) ;
#6588 = LINE ( 'NONE', #30448, #5924 ) ;
#6589 = CARTESIAN_POINT ( 'NONE',  ( 1.655785408456140084, 0.7536129375913136474, 9.903764339332061795 ) ) ;
#6590 = CARTESIAN_POINT ( 'NONE',  ( 358.3431457505077447, 185.0000000000000284, 359.9999999999998863 ) ) ;
#6591 = CARTESIAN_POINT ( 'NONE',  ( -2.945500763482279627, -16.64098165802040086, -9.008049429158100807 ) ) ;
#6592 = EDGE_LOOP ( 'NONE', ( #6077, #260, #40368, #26391, #36192, #19814, #23537, #23326 ) ) ;
#6593 = FACE_OUTER_BOUND ( 'NONE', #19243, .T. ) ;
#6594 = DIRECTION ( 'NONE',  ( -1.000000000000000000, 0.000000000000000000, 0.000000000000000000 ) ) ;
#6595 = LINE ( 'NONE', #34564, #14160 ) ;
#6596 = CARTESIAN_POINT ( 'NONE',  ( -36.01122090644304308, -10.59066248886169070, -2.490396854064194532 ) ) ;
#6597 = AXIS2_PLACEMENT_3D ( 'NONE', #32525, #48106, #16346 ) ;
#6598 = CARTESIAN_POINT ( 'NONE',  ( 111.5540265531850679, 0.000000000000000000, -157.4317124430720582 ) ) ;
#6599 = AXIS2_PLACEMENT_3D ( 'NONE', #29273, #1072, #25424 ) ;
#6600 = DIRECTION ( 'NONE',  ( -1.000000000000000000, 0.000000000000000000, 0.000000000000000000 ) ) ;
#6601 = ORIENTED_EDGE ( 'NONE', *, *, #26431, .T. ) ;
#6602 = EDGE_CURVE ( 'NONE', #22111, #11547, #7718, .T. ) ;
#6603 = DIRECTION ( 'NONE',  ( -0.000000000000000000, -0.000000000000000000, -1.000000000000000000 ) ) ;
#6604 = VECTOR ( 'NONE', #4255, 1000.000000000000000 ) ;
#6605 = CARTESIAN_POINT ( 'NONE',  ( -29.39982726364978660, -16.78152490921149109, 8.356839323120299312 ) ) ;
#6606 = CARTESIAN_POINT ( 'NONE',  ( -84.94597344681493212, 1.025126265847089435, -157.4317124430720582 ) ) ;
#6607 = ORIENTED_EDGE ( 'NONE', *, *, #44982, .F. ) ;
#6608 = CARTESIAN_POINT ( 'NONE',  ( 111.5540265531850679, 0.000000000000000000, -77.43171244307204404 ) ) ;
#6609 = B_SPLINE_CURVE_WITH_KNOTS ( 'NONE', 3,
 ( #9277, #31884, #13369, #47480 ),
 .UNSPECIFIED., .F., .F.,
 ( 4, 4 ),
 ( 5.641302087946644680E-05, 0.0003272669002642551728 ),
 .UNSPECIFIED. ) ;
#6610 = DIRECTION ( 'NONE',  ( -1.000000000000000000, 0.000000000000000000, 0.000000000000000000 ) ) ;
#6611 = ORIENTED_EDGE ( 'NONE', *, *, #44325, .F. ) ;
#6612 = CARTESIAN_POINT ( 'NONE',  ( 111.5540265531850537, 1.025126265847081442, 162.5682875569279133 ) ) ;
#6613 = LINE ( 'NONE', #2014, #45101 ) ;
#6614 = DIRECTION ( 'NONE',  ( -0.000000000000000000, -0.000000000000000000, -1.000000000000000000 ) ) ;
#6615 = CARTESIAN_POINT ( 'NONE',  ( -44.94597344681493922, -1.025126265847089435, -40.93171244307204404 ) ) ;
#6616 = ORIENTED_EDGE ( 'NONE', *, *, #8597, .F. ) ;
#6617 = DIRECTION ( 'NONE',  ( -0.000000000000000000, -0.000000000000000000, -1.000000000000000000 ) ) ;
#6618 = EDGE_LOOP ( 'NONE', ( #14587, #14269, #12096 ) ) ;
#6619 = ORIENTED_EDGE ( 'NONE', *, *, #40725, .T. ) ;
#6620 = CARTESIAN_POINT ( 'NONE',  ( 350.0000000000000000, 169.0000000000000000, -356.0000000000002274 ) ) ;
#6621 = EDGE_LOOP ( 'NONE', ( #40075, #27301, #48862, #10561 ) ) ;
#6622 = CARTESIAN_POINT ( 'NONE',  ( -194.9999999999999432, 164.9999999999999716, 352.0000000000000000 ) ) ;
#6623 = CARTESIAN_POINT ( 'NONE',  ( -48.99656738986512039, 11.00747004110376182, 1.847720168420772691 ) ) ;
#6624 =( BOUNDED_CURVE ( )  B_SPLINE_CURVE ( 3, ( #23376, #16190, #19774, #35454 ),
 .UNSPECIFIED., .F., .F. ) 
 B_SPLINE_CURVE_WITH_KNOTS ( ( 4, 4 ),
 ( 0.000000000000000000, 1.570796326794896558 ),
 .UNSPECIFIED. ) 
 CURVE ( )  GEOMETRIC_REPRESENTATION_ITEM ( )  RATIONAL_B_SPLINE_CURVE ( ( 1.000000000000000000, 0.8047378541243649375, 0.8047378541243649375, 1.000000000000000000 ) ) 
 REPRESENTATION_ITEM ( '' )  );
#6625 = DIRECTION ( 'NONE',  ( 1.000000000000000000, 0.000000000000000000, 0.000000000000000000 ) ) ;
#6626 = CARTESIAN_POINT ( 'NONE',  ( 29.38926261462312439, 40.45084971874776159, 0.000000000000000000 ) ) ;
#6627 = B_SPLINE_CURVE_WITH_KNOTS ( 'NONE', 3,
 ( #11920, #12658, #19853, #31427 ),
 .UNSPECIFIED., .F., .F.,
 ( 4, 4 ),
 ( 0.7998230999345287140, 0.9869080488566183140 ),
 .UNSPECIFIED. ) ;
#6628 = CYLINDRICAL_SURFACE ( 'NONE', #13662, 1.750000000000008438 ) ;
#6629 = VERTEX_POINT ( 'NONE', #36625 ) ;
#6631 = EDGE_CURVE ( 'NONE', #38172, #7457, #12972, .T. ) ;
#6630 = CARTESIAN_POINT ( 'NONE',  ( -44.94597344681493922, 2.143131898507880377E-16, -37.43171244307200141 ) ) ;
#6632 = AXIS2_PLACEMENT_3D ( 'NONE', #26765, #42396, #27013 ) ;
#6633 = CARTESIAN_POINT ( 'NONE',  ( 166.9999999999999716, -164.9999999999999432, 343.9999999999998863 ) ) ;
#6634 = LINE ( 'NONE', #3028, #34072 ) ;
#6635 = ORIENTED_EDGE ( 'NONE', *, *, #10833, .T. ) ;
#6636 = CARTESIAN_POINT ( 'NONE',  ( -177.4999999999999716, 74.83106485270648989, -130.5992382549688955 ) ) ;
#6637 = CARTESIAN_POINT ( 'NONE',  ( 210.0000000000000568, 0.000000000000000000, -79.18171244307201562 ) ) ;
#6638 = ORIENTED_EDGE ( 'NONE', *, *, #9099, .F. ) ;
#6639 = APPLICATION_CONTEXT ( 'automotive_design' ) ;
#6640 = EDGE_LOOP ( 'NONE', ( #42790, #15204, #31412, #26288, #39097, #23130, #39834, #22033 ) ) ;
#6641 = ORIENTED_EDGE ( 'NONE', *, *, #45637, .T. ) ;
#6642 = DIRECTION ( 'NONE',  ( 0.000000000000000000, -0.2791762785758810650, 0.9602398687205827565 ) ) ;
#6643 = CARTESIAN_POINT ( 'NONE',  ( -50.64730461691362962, 47.68801056904006685, 742.8425600500171413 ) ) ;
#6644 = AXIS2_PLACEMENT_3D ( 'NONE', #46015, #6550, #17841 ) ;
#6645 = ORIENTED_EDGE ( 'NONE', *, *, #42734, .F. ) ;
#6646 = FACE_OUTER_BOUND ( 'NONE', #1275, .T. ) ;
#6647 = CARTESIAN_POINT ( 'NONE',  ( 0.000000000000000000, -250.0000000000000000, 225.0000000000000000 ) ) ;
#6648 = ORIENTED_EDGE ( 'NONE', *, *, #4887, .F. ) ;
#6649 = DIRECTION ( 'NONE',  ( 0.000000000000000000, 0.000000000000000000, 1.000000000000000000 ) ) ;
#6650 = CARTESIAN_POINT ( 'NONE',  ( 1.073226156958098532, 0.6788500330460306431, 9.975314328424618182 ) ) ;
#6651 = ORIENTED_EDGE ( 'NONE', *, *, #50432, .F. ) ;
#6652 = FACE_OUTER_BOUND ( 'NONE', #35530, .T. ) ;
#6653 = LINE ( 'NONE', #6160, #15236 ) ;
#6654 = CARTESIAN_POINT ( 'NONE',  ( 8.470991794550016607, 5.371644396275345734, 9.390253821402620105 ) ) ;
#6655 = DIRECTION ( 'NONE',  ( -0.000000000000000000, -0.000000000000000000, -1.000000000000000000 ) ) ;
#6656 = VERTEX_POINT ( 'NONE', #4774 ) ;
#6657 = LINE ( 'NONE', #46123, #33752 ) ;
#6658 = EDGE_CURVE ( 'NONE', #21408, #36017, #8882, .T. ) ;
#6659 = CARTESIAN_POINT ( 'NONE',  ( -40.76831105797795374, -21.94948152812802178, 7.455576670931137073 ) ) ;
#6660 = AXIS2_PLACEMENT_3D ( 'NONE', #29673, #25323, #45293 ) ;
#6661 = CARTESIAN_POINT ( 'NONE',  ( -65.00000000000002842, 17.00000000000000000, -114.9999999999999858 ) ) ;
#6662 = FACE_OUTER_BOUND ( 'NONE', #28009, .T. ) ;
#6663 = VECTOR ( 'NONE', #40743, 1000.000000000000000 ) ;
#6664 = ORIENTED_EDGE ( 'NONE', *, *, #32113, .T. ) ;
#6665 = CARTESIAN_POINT ( 'NONE',  ( 33.30402655318503946, -1.750000000000010658, 80.81828755692798438 ) ) ;
#6666 = ORIENTED_EDGE ( 'NONE', *, *, #9875, .F. ) ;
#6667 = CARTESIAN_POINT ( 'NONE',  ( -3.996390545799824334, 16.57371371864897469, 8.953103998512858652 ) ) ;
#6668 = EDGE_LOOP ( 'NONE', ( #43590, #42292, #30083, #16544 ) ) ;
#6669 = CARTESIAN_POINT ( 'NONE',  ( -86.69597344681494633, -1.750000000000010214, -39.18171244307202983 ) ) ;
#6671 = ADVANCED_FACE ( 'NONE', ( #32747 ), #48340, .T. ) ;
#6670 = CARTESIAN_POINT ( 'NONE',  ( 33.30402655318503946, 1.750000000000010658, -79.18171244307201562 ) ) ;
#6672 = EDGE_CURVE ( 'NONE', #37522, #42553, #32026, .T. ) ;
#6673 = VECTOR ( 'NONE', #42889, 1000.000000000000000 ) ;
#6674 = ORIENTED_EDGE ( 'NONE', *, *, #14486, .F. ) ;
#6675 = SURFACE_SIDE_STYLE ('',( #49983 ) ) ;
#6676 = ORIENTED_EDGE ( 'NONE', *, *, #7323, .F. ) ;
#6677 = EDGE_CURVE ( 'NONE', #29935, #41724, #47839, .T. ) ;
#6678 =( BOUNDED_CURVE ( )  B_SPLINE_CURVE ( 3, ( #22047, #13827, #37721, #9738 ),
 .UNSPECIFIED., .F., .F. ) 
 B_SPLINE_CURVE_WITH_KNOTS ( ( 4, 4 ),
 ( 0.000000000000000000, 1.570796326794896780 ),
 .UNSPECIFIED. ) 
 CURVE ( )  GEOMETRIC_REPRESENTATION_ITEM ( )  RATIONAL_B_SPLINE_CURVE ( ( 1.000000000000000000, 0.8047378541243649375, 0.8047378541243649375, 1.000000000000000000 ) ) 
 REPRESENTATION_ITEM ( '' )  );
#6679 = FACE_OUTER_BOUND ( 'NONE', #45452, .T. ) ;
#6680 = ORIENTED_EDGE ( 'NONE', *, *, #18204, .F. ) ;
#6681 = DIRECTION ( 'NONE',  ( -1.000000000000000000, -0.000000000000000000, -0.000000000000000000 ) ) ;
#6682 = CARTESIAN_POINT ( 'NONE',  ( 181.0000000000000284, -174.9999999999999716, -113.0000000000001563 ) ) ;
#6683 = CARTESIAN_POINT ( 'NONE',  ( -13.59579750444763668, 10.60877755095910935, 8.727788335465566760 ) ) ;
#6684 = CARTESIAN_POINT ( 'NONE',  ( -176.3085477938156487, 47.50000000000000000, -19.92876838486919411 ) ) ;
#6685 = CYLINDRICAL_SURFACE ( 'NONE', #29004, 1.750000000000015543 ) ;
#6686 =( BOUNDED_CURVE ( )  B_SPLINE_CURVE ( 3, ( #12270, #20988, #39741, #13268 ),
 .UNSPECIFIED., .F., .F. ) 
 B_SPLINE_CURVE_WITH_KNOTS ( ( 4, 4 ),
 ( 1.570796326794896558, 3.141592653589793116 ),
 .UNSPECIFIED. ) 
 CURVE ( )  GEOMETRIC_REPRESENTATION_ITEM ( )  RATIONAL_B_SPLINE_CURVE ( ( 1.000000000000000000, 0.8047378541243649375, 0.8047378541243649375, 1.000000000000000000 ) ) 
 REPRESENTATION_ITEM ( '' )  );
#6687 = ORIENTED_EDGE ( 'NONE', *, *, #23028, .F. ) ;
#6689 = ORIENTED_EDGE ( 'NONE', *, *, #15366, .T. ) ;
#6688 = EDGE_CURVE ( 'NONE', #16962, #38289, #43772, .T. ) ;
#6690 = CARTESIAN_POINT ( 'NONE',  ( 183.0000000000000000, -5.999999999999950262, 339.9999999999998295 ) ) ;
#6691 = EDGE_CURVE ( 'NONE', #32541, #50118, #37120, .T. ) ;
#6692 = EDGE_CURVE ( 'NONE', #46399, #31585, #44769, .T. ) ;
#6693 = ADVANCED_FACE ( 'NONE', ( #40949 ), #48912, .T. ) ;
#6694 = EDGE_LOOP ( 'NONE', ( #26065, #24713, #33988, #48027, #47760, #3493 ) ) ;
#6695 = CARTESIAN_POINT ( 'NONE',  ( 33.57695195286775913, 16.69845195084893064, 8.914903342594561408 ) ) ;
#6696 = DIRECTION ( 'NONE',  ( -1.000000000000000000, 0.000000000000000000, 0.000000000000000000 ) ) ;
#6697 = VERTEX_POINT ( 'NONE', #18585 ) ;
#6698 = CARTESIAN_POINT ( 'NONE',  ( -0.9494396179258391966, 9.954826186926261755, 9.646707543097345905 ) ) ;
#6699 = AXIS2_PLACEMENT_3D ( 'NONE', #1550, #8992, #21801 ) ;
#6700 = EDGE_CURVE ( 'NONE', #13420, #17053, #10899, .T. ) ;
#6701 = DIRECTION ( 'NONE',  ( 0.000000000000000000, 0.000000000000000000, -1.000000000000000000 ) ) ;
#6702 = ORIENTED_EDGE ( 'NONE', *, *, #23940, .T. ) ;
#6703 = CARTESIAN_POINT ( 'NONE',  ( 0.000000000000000000, 0.000000000000000000, 10.00000000000000000 ) ) ;
#6704 = CARTESIAN_POINT ( 'NONE',  ( 34.38425513258721367, -36.82177522737821107, 8.807470649214879543 ) ) ;
#6705 = FACE_OUTER_BOUND ( 'NONE', #42021, .T. ) ;
#6706 = CARTESIAN_POINT ( 'NONE',  ( -87.72109971266203843, 1.750000000000009548, 39.79316129108089228 ) ) ;
#6707 = CIRCLE ( 'NONE', #31311, 4.000000000000003553 ) ;
#6708 = EDGE_LOOP ( 'NONE', ( #41960, #34655, #7524, #47985 ) ) ;
#6709 = EDGE_LOOP ( 'NONE', ( #15716, #4983, #40703, #34939 ) ) ;
#6710 = CARTESIAN_POINT ( 'NONE',  ( 135.0000000000003411, 17.00000000000000000, -60.00000000000000000 ) ) ;
#6711 = DIRECTION ( 'NONE',  ( 1.000000000000000000, 0.000000000000000000, -1.860490536778032451E-50 ) ) ;
#6712 = ORIENTED_EDGE ( 'NONE', *, *, #29955, .T. ) ;
#6713 = ADVANCED_FACE ( 'NONE', ( #41699 ), #14496, .F. ) ;
#6714 = ORIENTED_EDGE ( 'NONE', *, *, #47843, .T. ) ;
#6715 =( NAMED_UNIT ( * ) SI_UNIT ( $, .STERADIAN. ) SOLID_ANGLE_UNIT ( ) );
#6716 = CARTESIAN_POINT ( 'NONE',  ( 75.05402655318509630, 1.025126265847089657, -120.9317124430720440 ) ) ;
#6717 = CARTESIAN_POINT ( 'NONE',  ( -44.94597344681493922, -1.025126265847089435, 162.5682875569279133 ) ) ;
#6718 = CARTESIAN_POINT ( 'NONE',  ( -22.69295089195507487, -45.31600496604688999, 7.455576670931136185 ) ) ;
#6719 = EDGE_CURVE ( 'NONE', #6011, #45351, #41184, .T. ) ;
#6720 = EDGE_CURVE ( 'NONE', #26345, #33351, #34012, .T. ) ;
#6721 = DIRECTION ( 'NONE',  ( 0.000000000000000000, 0.000000000000000000, 1.000000000000000000 ) ) ;
#6722 = CARTESIAN_POINT ( 'NONE',  ( -1.437255894074058515, 3.713052624461494755, 6.606856988583542645E-16 ) ) ;
#6723 = LINE ( 'NONE', #2858, #14130 ) ;
#6724 = EDGE_LOOP ( 'NONE', ( #17001, #30815, #36441 ) ) ;
#6725 = CARTESIAN_POINT ( 'NONE',  ( 1.025617443043004062, 1.003000432358625238, 9.950105812514292936 ) ) ;
#6726 = ADVANCED_FACE ( 'NONE', ( #2201, #48848 ), #49598, .T. ) ;
#6727 = LINE ( 'NONE', #49777, #20408 ) ;
#6728 = LINE ( 'NONE', #7240, #8606 ) ;
#6729 = EDGE_CURVE ( 'NONE', #4735, #33351, #37872, .T. ) ;
#6730 = FILL_AREA_STYLE_COLOUR ( '', #5082 ) ;
#6731 = ORIENTED_EDGE ( 'NONE', *, *, #11598, .F. ) ;
#6732 = VECTOR ( 'NONE', #40922, 1000.000000000000000 ) ;
#6733 = FACE_OUTER_BOUND ( 'NONE', #4106, .T. ) ;
#6734 = EDGE_LOOP ( 'NONE', ( #635, #47451, #7310, #5661, #30992, #14840 ) ) ;
#6735 = DIRECTION ( 'NONE',  ( 0.000000000000000000, -1.000000000000000000, 0.000000000000000000 ) ) ;
#6736 = VECTOR ( 'NONE', #27929, 1000.000000000000000 ) ;
#6737 = DIRECTION ( 'NONE',  ( -1.000000000000000000, 0.000000000000000000, 0.000000000000000000 ) ) ;
#6738 = CARTESIAN_POINT ( 'NONE',  ( -207.7210997126620384, -1.750000000000010214, -78.15658617722490931 ) ) ;
#6739 = VERTEX_POINT ( 'NONE', #10644 ) ;
#6740 = VECTOR ( 'NONE', #22946, 1000.000000000000000 ) ;
#6741 = AXIS2_PLACEMENT_3D ( 'NONE', #13315, #21274, #17177 ) ;
#6742 = CARTESIAN_POINT ( 'NONE',  ( -114.9999999999991047, 16.00000000000000000, 0.000000000000000000 ) ) ;
#6743 = EDGE_LOOP ( 'NONE', ( #6243, #36241, #2536, #33323 ) ) ;
#6744 = FACE_OUTER_BOUND ( 'NONE', #37353, .T. ) ;
#6745 = EDGE_CURVE ( 'NONE', #20029, #40480, #18895, .T. ) ;
#6746 = DIRECTION ( 'NONE',  ( -1.000000000000000000, -0.000000000000000000, -0.000000000000000000 ) ) ;
#6747 = CARTESIAN_POINT ( 'NONE',  ( -114.9999999999981526, 16.00000000000000000, 90.00000000000000000 ) ) ;
#6748 = ORIENTED_EDGE ( 'NONE', *, *, #36709, .F. ) ;
#6749 = VERTEX_POINT ( 'NONE', #7063 ) ;
#6750 = CARTESIAN_POINT ( 'NONE',  ( -4.190612935961002705, -4.237468719480293800, 5.692061405548898279E-16 ) ) ;
#6751 = DIRECTION ( 'NONE',  ( 0.000000000000000000, 1.000000000000000000, 0.000000000000000000 ) ) ;
#6752 = EDGE_CURVE ( 'NONE', #24640, #14882, #22699, .T. ) ;
#6753 = EDGE_CURVE ( 'NONE', #5437, #36214, #23162, .T. ) ;
#6754 = ORIENTED_EDGE ( 'NONE', *, *, #27997, .T. ) ;
#6755 = ORIENTED_EDGE ( 'NONE', *, *, #28674, .F. ) ;
#6756 = CARTESIAN_POINT ( 'NONE',  ( -165.0000000000000284, 16.00000000000000000, 115.0000000000000142 ) ) ;
#6757 = DIRECTION ( 'NONE',  ( 0.000000000000000000, 0.3790464617558786942, -0.9253776417389547593 ) ) ;
#6758 = DIRECTION ( 'NONE',  ( 1.000000000000000000, 0.000000000000000000, -0.000000000000000000 ) ) ;
#6759 = ORIENTED_EDGE ( 'NONE', *, *, #25597, .T. ) ;
#6760 = LINE ( 'NONE', #19059, #1408 ) ;
#6761 = ADVANCED_FACE ( 'NONE', ( #6800, #22447 ), #6307, .T. ) ;
#6762 = ORIENTED_EDGE ( 'NONE', *, *, #21537, .T. ) ;
#6763 = VECTOR ( 'NONE', #15781, 1000.000000000000000 ) ;
#6764 = EDGE_CURVE ( 'NONE', #13831, #12618, #18088, .T. ) ;
#6765 = EDGE_CURVE ( 'NONE', #24983, #41718, #10144, .T. ) ;
#6766 = DIRECTION ( 'NONE',  ( 0.000000000000000000, 0.4027858274925601445, 0.9152942571496521795 ) ) ;
#6767 = CARTESIAN_POINT ( 'NONE',  ( -69.99999999999940314, 17.00000000000000000, -54.99999999999999289 ) ) ;
#6768 = ORIENTED_EDGE ( 'NONE', *, *, #46179, .F. ) ;
#6769 = ORIENTED_EDGE ( 'NONE', *, *, #36702, .T. ) ;
#6770 = MECHANICAL_DESIGN_GEOMETRIC_PRESENTATION_REPRESENTATION (  '', ( #28896 ), #45071 ) ;
#6771 = VERTEX_POINT ( 'NONE', #14235 ) ;
#6772 = FILL_AREA_STYLE ('',( #26280 ) ) ;
#6773 = AXIS2_PLACEMENT_3D ( 'NONE', #44817, #1499, #49146 ) ;
#6774 = CARTESIAN_POINT ( 'NONE',  ( 10.50000000000000178, -46.01315789473684248, -5.916985404131818171 ) ) ;
#6775 = EDGE_LOOP ( 'NONE', ( #8519, #20508, #12338, #1769, #5058 ) ) ;
#6776 = CARTESIAN_POINT ( 'NONE',  ( 0.8510287611193416701, 1.787020300839067932, 9.897807938190497978 ) ) ;
#6777 = ORIENTED_EDGE ( 'NONE', *, *, #27524, .F. ) ;
#6778 = PRESENTATION_LAYER_ASSIGNMENT (  '', '', ( #14951 ) ) ;
#6779 = CARTESIAN_POINT ( 'NONE',  ( 35.05402655318504657, 2.143131898507880377E-16, 165.0000000000000000 ) ) ;
#6780 = PLANE ( 'NONE',  #14978 ) ;
#6781 = ORIENTED_EDGE ( 'NONE', *, *, #44542, .F. ) ;
#6782 = CARTESIAN_POINT ( 'NONE',  ( -34.38425513258695077, 36.82177522737848108, 8.807470649214879543 ) ) ;
#6783 = DIRECTION ( 'NONE',  ( -1.000000000000000000, 0.000000000000000000, 0.000000000000000000 ) ) ;
#6784 = FACE_OUTER_BOUND ( 'NONE', #19902, .T. ) ;
#6785 = LINE ( 'NONE', #50082, #41688 ) ;
#6786 = EDGE_CURVE ( 'NONE', #9357, #22918, #45520, .T. ) ;
#6787 = CARTESIAN_POINT ( 'NONE',  ( 210.0000000000000568, 2.143131898507881856E-16, 79.06828755692797017 ) ) ;
#6788 = ORIENTED_EDGE ( 'NONE', *, *, #43538, .F. ) ;
#6789 = DIRECTION ( 'NONE',  ( 1.000000000000000000, 0.000000000000000000, 0.000000000000000000 ) ) ;
#6790 = CARTESIAN_POINT ( 'NONE',  ( 35.00000000000061107, 17.00000000000000000, -54.99999999999999289 ) ) ;
#6791 = B_SPLINE_SURFACE_WITH_KNOTS ( 'NONE', 3, 3, ( 
 ( #21183, #17838, #29147, #40946 ),
 ( #36873, #17084, #29895, #9389 ),
 ( #45516, #25542, #14231, #33263 ),
 ( #25048, #33006, #5788, #10400 ) ),
 .UNSPECIFIED., .F., .F., .F.,
 ( 4, 4 ),
 ( 4, 4 ),
 ( 0.000000000000000000, 1.000000000000000000 ),
 ( 0.000000000000000000, 1.000000000000000000 ),
 .UNSPECIFIED. ) ;
#6792 = PRODUCT_DEFINITION ( 'UNKNOWN', '', #48740, #20094 ) ;
#6793 = CARTESIAN_POINT ( 'NONE',  ( 1.011271242968683648, 0.7347315653655930312, 3.333333333333333481 ) ) ;
#6794 = DIRECTION ( 'NONE',  ( 1.000000000000000000, 0.000000000000000000, 0.000000000000000000 ) ) ;
#6795 = FACE_OUTER_BOUND ( 'NONE', #16561, .T. ) ;
#6796 = CYLINDRICAL_SURFACE ( 'NONE', #35174, 1.750000000000001554 ) ;
#6797 = CARTESIAN_POINT ( 'NONE',  ( -86.69597344681494633, -1.750000000000009992, -159.1817124430720298 ) ) ;
#6798 = EDGE_CURVE ( 'NONE', #38906, #36749, #3185, .T. ) ;
#6799 = CARTESIAN_POINT ( 'NONE',  ( 0.000000000000000000, 23.48684210526316107, 0.000000000000000000 ) ) ;
#6800 = FACE_BOUND ( 'NONE', #36001, .T. ) ;
#6801 = ORIENTED_EDGE ( 'NONE', *, *, #2827, .T. ) ;
#6802 = CARTESIAN_POINT ( 'NONE',  ( -15.00000000000001421, 17.00000000000000000, -90.00000000000000000 ) ) ;
#6803 = CARTESIAN_POINT ( 'NONE',  ( 30.25247992116058526, -39.82368563463805344, -3.760136334089591248 ) ) ;
#6804 = VECTOR ( 'NONE', #27452, 1000.000000000000000 ) ;
#6805 = CARTESIAN_POINT ( 'NONE',  ( -5.888214538810513154, -16.20866436362413410, 8.727788335465566760 ) ) ;
#6806 = CYLINDRICAL_SURFACE ( 'NONE', #38800, 4.000000000000003553 ) ;
#6807 = CARTESIAN_POINT ( 'NONE',  ( -8.445973446814976526, 0.000000000000000000, -40.93171244307205825 ) ) ;
#6808 = AXIS2_PLACEMENT_3D ( 'NONE', #38107, #41685, #30144 ) ;
#6809 = ORIENTED_EDGE ( 'NONE', *, *, #40032, .T. ) ;
#6810 = ORIENTED_EDGE ( 'NONE', *, *, #3337, .F. ) ;
#6811 = CARTESIAN_POINT ( 'NONE',  ( 1.250000000000000222, 0.000000000000000000, 10.00000000000000000 ) ) ;
#6812 = PRESENTATION_LAYER_ASSIGNMENT (  '', '', ( #24846 ) ) ;
#6813 = CARTESIAN_POINT ( 'NONE',  ( 167.0000000000000000, -168.9999999999999432, -115.0000000000001847 ) ) ;
#6814 = ADVANCED_FACE ( 'NONE', ( #15515 ), #34789, .T. ) ;
#6815 = ADVANCED_FACE ( 'NONE', ( #27059 ), #35295, .F. ) ;
#6816 = ORIENTED_EDGE ( 'NONE', *, *, #22360, .T. ) ;
#6817 = TOROIDAL_SURFACE ( 'NONE', #21572, 27.58190990837850265, 8.000000000000000000 ) ;
#6818 = CARTESIAN_POINT ( 'NONE',  ( 3.996390545799824334, -16.57371371864897469, 8.953103998512858652 ) ) ;
#6819 = DIRECTION ( 'NONE',  ( -0.000000000000000000, -1.000000000000000000, 2.537652627714643577E-15 ) ) ;
#6820 = LINE ( 'NONE', #18852, #7874 ) ;
#6821 = ORIENTED_EDGE ( 'NONE', *, *, #12059, .T. ) ;
#6822 = ORIENTED_EDGE ( 'NONE', *, *, #34964, .F. ) ;
#6823 = ORIENTED_EDGE ( 'NONE', *, *, #31272, .T. ) ;
#6824 = EDGE_CURVE ( 'NONE', #47608, #35061, #42694, .T. ) ;
#6826 = EDGE_CURVE ( 'NONE', #5803, #1861, #23479, .T. ) ;
#6825 = PLANE ( 'NONE',  #20068 ) ;
#6827 = LINE ( 'NONE', #42977, #36570 ) ;
#6828 = ADVANCED_FACE ( 'NONE', ( #8333 ), #11668, .F. ) ;
#6829 = CARTESIAN_POINT ( 'NONE',  ( 25.60949810002064098, 43.19700938445193827, 1.847720168420772691 ) ) ;
#6830 =( BOUNDED_CURVE ( )  B_SPLINE_CURVE ( 3, ( #39925, #27865, #32221, #31973 ),
 .UNSPECIFIED., .F., .F. ) 
 B_SPLINE_CURVE_WITH_KNOTS ( ( 4, 4 ),
 ( 0.000000000000000000, 1.570796326794896558 ),
 .UNSPECIFIED. ) 
 CURVE ( )  GEOMETRIC_REPRESENTATION_ITEM ( )  RATIONAL_B_SPLINE_CURVE ( ( 1.000000000000000000, 0.8047378541243649375, 0.8047378541243649375, 1.000000000000000000 ) ) 
 REPRESENTATION_ITEM ( '' )  );
#6831 = ORIENTED_EDGE ( 'NONE', *, *, #26303, .F. ) ;
#6832 = CARTESIAN_POINT ( 'NONE',  ( -207.7210997126620384, -1.750000000000010214, 81.84341382277507648 ) ) ;
#6833 = CARTESIAN_POINT ( 'NONE',  ( -204.9459734468148895, 1.025126265847089435, 2.568287556927986159 ) ) ;
#6834 = CARTESIAN_POINT ( 'NONE',  ( -47.72109971266203132, -1.750000000000010214, -118.1565861772249519 ) ) ;
#6835 = ORIENTED_EDGE ( 'NONE', *, *, #48462, .T. ) ;
#6836 = ORIENTED_EDGE ( 'NONE', *, *, #41640, .F. ) ;
#6837 = CARTESIAN_POINT ( 'NONE',  ( -8.445973446814976526, 0.000000000000000000, 39.06828755692792754 ) ) ;
#6839 = CYLINDRICAL_SURFACE ( 'NONE', #36611, 4.000000000000003553 ) ;
#6838 =( BOUNDED_CURVE ( )  B_SPLINE_CURVE ( 3, ( #4627, #47176, #8482, #27470 ),
 .UNSPECIFIED., .F., .F. ) 
 B_SPLINE_CURVE_WITH_KNOTS ( ( 4, 4 ),
 ( 3.141592653589793116, 4.712388980384689674 ),
 .UNSPECIFIED. ) 
 CURVE ( )  GEOMETRIC_REPRESENTATION_ITEM ( )  RATIONAL_B_SPLINE_CURVE ( ( 1.000000000000000000, 0.8047378541243649375, 0.8047378541243649375, 1.000000000000000000 ) ) 
 REPRESENTATION_ITEM ( '' )  );
#6840 = EDGE_CURVE ( 'NONE', #18355, #18198, #23726, .T. ) ;
#6841 = CARTESIAN_POINT ( 'NONE',  ( -48.44597344681496054, 1.025126265847089435, -40.93171244307204404 ) ) ;
#6842 = VERTEX_POINT ( 'NONE', #7570 ) ;
#6843 = ORIENTED_EDGE ( 'NONE', *, *, #34749, .T. ) ;
#6844 = DIRECTION ( 'NONE',  ( -1.000000000000000000, -0.000000000000000000, -0.000000000000000000 ) ) ;
#6845 = DIRECTION ( 'NONE',  ( 0.000000000000000000, 0.000000000000000000, -1.000000000000000000 ) ) ;
#6846 = CARTESIAN_POINT ( 'NONE',  ( -1.290940757015139662, 0.08848829412237076142, 9.947020512645400103 ) ) ;
#6847 = LINE ( 'NONE', #10943, #749 ) ;
#6848 = AXIS2_PLACEMENT_3D ( 'NONE', #12713, #12953, #24784 ) ;
#6849 = VECTOR ( 'NONE', #13860, 1000.000000000000000 ) ;
#6850 = DIRECTION ( 'NONE',  ( -1.000000000000000000, -0.000000000000000000, -0.000000000000000000 ) ) ;
#6851 = ORIENTED_EDGE ( 'NONE', *, *, #36811, .T. ) ;
#6852 = PLANE ( 'NONE',  #34967 ) ;
#6853 = DIRECTION ( 'NONE',  ( 0.000000000000000000, 0.000000000000000000, 1.000000000000000000 ) ) ;
#6854 =( BOUNDED_CURVE ( )  B_SPLINE_CURVE ( 3, ( #45923, #10804, #6962, #46430 ),
 .UNSPECIFIED., .F., .F. ) 
 B_SPLINE_CURVE_WITH_KNOTS ( ( 4, 4 ),
 ( 3.141592653589793116, 4.712388980384689674 ),
 .UNSPECIFIED. ) 
 CURVE ( )  GEOMETRIC_REPRESENTATION_ITEM ( )  RATIONAL_B_SPLINE_CURVE ( ( 1.000000000000000000, 0.8047378541243649375, 0.8047378541243649375, 1.000000000000000000 ) ) 
 REPRESENTATION_ITEM ( '' )  );
#6855 = CARTESIAN_POINT ( 'NONE',  ( -33.57695195286787282, -16.69845195084869616, 8.914903342594564961 ) ) ;
#6856=STYLED_ITEM('',(#50754),#39479);
#6857 = CARTESIAN_POINT ( 'NONE',  ( 33.08717642956893457, 5.870837526465158440, -8.016098858316205167 ) ) ;
#6858 = DIRECTION ( 'NONE',  ( 0.000000000000000000, -1.000000000000000000, 2.537652627714642000E-15 ) ) ;
#6859 = ORIENTED_EDGE ( 'NONE', *, *, #46926, .T. ) ;
#6860 = CARTESIAN_POINT ( 'NONE',  ( -1.250000000000000222, 0.000000000000000000, 10.00000000000000000 ) ) ;
#6861 = CARTESIAN_POINT ( 'NONE',  ( 183.0000000000000000, -5.999999999999950262, 339.9999999999998295 ) ) ;
#6862 = DIRECTION ( 'NONE',  ( 0.000000000000000000, 0.000000000000000000, 1.000000000000000000 ) ) ;
#6863 = EDGE_CURVE ( 'NONE', #22911, #11669, #42953, .T. ) ;
#6864 = ORIENTED_EDGE ( 'NONE', *, *, #14260, .F. ) ;
#6865 = CARTESIAN_POINT ( 'NONE',  ( 195.0540265531851105, 2.143131898507880377E-16, 82.56828755692798438 ) ) ;
#6866 = VECTOR ( 'NONE', #32157, 1000.000000000000114 ) ;
#6867 = LINE ( 'NONE', #41011, #31966 ) ;
#6868 = ORIENTED_EDGE ( 'NONE', *, *, #46653, .T. ) ;
#6869 = CARTESIAN_POINT ( 'NONE',  ( -48.44597344681496054, -1.025126265847089435, 39.06828755692797728 ) ) ;
#6870 = CARTESIAN_POINT ( 'NONE',  ( -164.9459734468149463, 2.143131898507880377E-16, 79.06828755692797017 ) ) ;
#6871 = DIRECTION ( 'NONE',  ( 0.000000000000000000, -1.000000000000000000, 0.000000000000000000 ) ) ;
#6872 = CARTESIAN_POINT ( 'NONE',  ( -87.72109971266203843, 1.750000000000009548, 41.84341382277508359 ) ) ;
#6873 = VERTEX_POINT ( 'NONE', #39139 ) ;
#6874 = DIRECTION ( 'NONE',  ( 0.000000000000000000, 0.000000000000000000, 1.000000000000000000 ) ) ;
#6875 = ORIENTED_EDGE ( 'NONE', *, *, #29069, .F. ) ;
#6876 = VERTEX_POINT ( 'NONE', #50098 ) ;
#6877 = CARTESIAN_POINT ( 'NONE',  ( 358.3431457505076878, 165.0000000000000284, 339.9999999999998295 ) ) ;
#6878 = ADVANCED_FACE ( 'NONE', ( #30668 ), #15010, .T. ) ;
#6879 = ORIENTED_EDGE ( 'NONE', *, *, #2276, .F. ) ;
#6880 = CARTESIAN_POINT ( 'NONE',  ( -128.4459734468149463, 1.025126265847081886, 39.06828755692799149 ) ) ;
#6881 = CARTESIAN_POINT ( 'NONE',  ( -175.0000000000000000, 0.000000000000000000, 122.5000000000000142 ) ) ;
#6882 = VECTOR ( 'NONE', #44035, 1000.000000000000000 ) ;
#6883 = CARTESIAN_POINT ( 'NONE',  ( -0.3862712429686977478, 1.188820645368937390, 10.00000000000000000 ) ) ;
#6884 = AXIS2_PLACEMENT_3D ( 'NONE', #29867, #21403, #32979 ) ;
#6885 = CARTESIAN_POINT ( 'NONE',  ( 9.999999999999998224, 8.486842105263161073, 18.46084505325461933 ) ) ;
#6886 = DIRECTION ( 'NONE',  ( 0.000000000000000000, 0.000000000000000000, -1.000000000000000000 ) ) ;
#6887 = VERTEX_POINT ( 'NONE', #46265 ) ;
#6888 = DIRECTION ( 'NONE',  ( -0.4374820812098861866, 0.3178493372392685590, 0.8411784753765543243 ) ) ;
#6890 = EDGE_CURVE ( 'NONE', #47659, #12079, #23481, .T. ) ;
#6889 = DIRECTION ( 'NONE',  ( 0.000000000000000000, 1.000000000000000000, -2.537652627714642000E-15 ) ) ;
#6891 = ADVANCED_FACE ( 'NONE', ( #8083 ), #42444, .T. ) ;
#6892 = DIRECTION ( 'NONE',  ( -1.000000000000000000, -1.156482317317870492E-16, 0.000000000000000000 ) ) ;
#6893 = ORIENTED_EDGE ( 'NONE', *, *, #26918, .T. ) ;
#6894 = CARTESIAN_POINT ( 'NONE',  ( 0.000000000000000000, -180.9999999999999716, -344.0000000000001705 ) ) ;
#6895 = CARTESIAN_POINT ( 'NONE',  ( 9.999999999999998224, 8.486842105263161073, -18.46084505325461578 ) ) ;
#6896 = ORIENTED_EDGE ( 'NONE', *, *, #24569, .F. ) ;
#6897 = ORIENTED_EDGE ( 'NONE', *, *, #39672, .F. ) ;
#6898 = EDGE_LOOP ( 'NONE', ( #33958, #7577, #23608, #21034, #41757 ) ) ;
#6899 = CARTESIAN_POINT ( 'NONE',  ( 1.250000000000000222, 0.000000000000000000, 10.00000000000000000 ) ) ;
#6900 = ADVANCED_FACE ( 'NONE', ( #35541 ), #26815, .F. ) ;
#6901 = CARTESIAN_POINT ( 'NONE',  ( -119.9999999999994174, 17.00000000000000000, -30.00000000000000000 ) ) ;
#6902 = B_SPLINE_SURFACE_WITH_KNOTS ( 'NONE', 3, 3, ( 
 ( #43430, #19829, #35774, #47250 ),
 ( #32151, #47744, #8806, #35507 ),
 ( #23941, #12634, #16499, #23693 ),
 ( #32403, #4699, #19574, #8300 ) ),
 .UNSPECIFIED., .F., .F., .F.,
 ( 4, 4 ),
 ( 4, 4 ),
 ( 0.000000000000000000, 1.000000000000000000 ),
 ( 0.000000000000000000, 1.000000000000000000 ),
 .UNSPECIFIED. ) ;
#6903 = ORIENTED_EDGE ( 'NONE', *, *, #44836, .F. ) ;
#6904 = CARTESIAN_POINT ( 'NONE',  ( 74.32915281903215998, -1.750000000000009548, 121.8434138227750623 ) ) ;
#6905 = LINE ( 'NONE', #3040, #13917 ) ;
#6906 = CARTESIAN_POINT ( 'NONE',  ( -88.44597344681497475, 0.000000000000000000, 119.0682875569279418 ) ) ;
#6907 = VECTOR ( 'NONE', #19140, 1000.000000000000000 ) ;
#6908 = DIRECTION ( 'NONE',  ( 0.000000000000000000, 0.000000000000000000, -1.000000000000000000 ) ) ;
#6909 = CARTESIAN_POINT ( 'NONE',  ( 341.6568542494922553, -165.0000000000001137, -340.0000000000002842 ) ) ;
#6910 = CARTESIAN_POINT ( 'NONE',  ( 71.55402655318505367, -1.025126265847089879, 82.56828755692798438 ) ) ;
#6911 = DIRECTION ( 'NONE',  ( -0.000000000000000000, -0.000000000000000000, -1.000000000000000000 ) ) ;
#6912 = CARTESIAN_POINT ( 'NONE',  ( -7.359817328027146388, -15.16751262232800102, 2.590526750877053086 ) ) ;
#6913 = B_SPLINE_CURVE_WITH_KNOTS ( 'NONE', 3,
 ( #3113, #43316, #31549, #38041 ),
 .UNSPECIFIED., .F., .F.,
 ( 4, 4 ),
 ( 3.806883176665572679E-16, 0.009762429722931321996 ),
 .UNSPECIFIED. ) ;
#6914 = ORIENTED_EDGE ( 'NONE', *, *, #10808, .F. ) ;
#6915 = CARTESIAN_POINT ( 'NONE',  ( -6.695973446814940111, 1.750000000000024203, 80.81828755692798438 ) ) ;
#6916 = CARTESIAN_POINT ( 'NONE',  ( -1.011271242968677875, -0.7347315653656004697, -3.333333333333333481 ) ) ;
#6917 = VECTOR ( 'NONE', #25895, 1000.000000000000000 ) ;
#6918 = FACE_OUTER_BOUND ( 'NONE', #9421, .T. ) ;
#6919 = DIRECTION ( 'NONE',  ( 0.000000000000000000, 0.000000000000000000, 1.000000000000000000 ) ) ;
#6920 = EDGE_LOOP ( 'NONE', ( #13462, #46064, #40915, #35482, #37027, #868 ) ) ;
#6921 = CARTESIAN_POINT ( 'NONE',  ( 1.448406091252584238, -0.9360325558322883932, 9.928159647716132241 ) ) ;
#6922 = VECTOR ( 'NONE', #22891, 1000.000000000000000 ) ;
#6923 = CARTESIAN_POINT ( 'NONE',  ( 340.0000000000000568, 169.0000000000000000, 349.9999999999998295 ) ) ;
#6924 = CARTESIAN_POINT ( 'NONE',  ( -14.99999999999906919, 16.00000000000000000, -24.99999999999999289 ) ) ;
#6925 = DIRECTION ( 'NONE',  ( 0.000000000000000000, 0.000000000000000000, 1.000000000000000000 ) ) ;
#6926 = VECTOR ( 'NONE', #45420, 1000.000000000000000 ) ;
#6927 = CARTESIAN_POINT ( 'NONE',  ( 168.9999999999999716, -164.9999999999999432, -344.0000000000001137 ) ) ;
#6928 = EDGE_CURVE ( 'NONE', #43155, #24145, #16474, .T. ) ;
#6929 = ORIENTED_EDGE ( 'NONE', *, *, #43129, .F. ) ;
#6930 = CARTESIAN_POINT ( 'NONE',  ( 153.3040265531850537, 0.000000000000000000, 165.0000000000000000 ) ) ;
#6931 = ORIENTED_EDGE ( 'NONE', *, *, #4477, .T. ) ;
#6932 = CARTESIAN_POINT ( 'NONE',  ( -6.174150299305392053, 50.00000000000000711, 8.807470649214879543 ) ) ;
#6933 = ORIENTED_EDGE ( 'NONE', *, *, #32149, .F. ) ;
#6934 = CARTESIAN_POINT ( 'NONE',  ( 1.275927284277173834, -0.1224368140627448004, 9.976582533991679824 ) ) ;
#6935 = CARTESIAN_POINT ( 'NONE',  ( -206.6959734468149463, 0.000000000000000000, 165.0000000000000000 ) ) ;
#6936 = VERTEX_POINT ( 'NONE', #3711 ) ;
#6937 = VERTEX_POINT ( 'NONE', #12177 ) ;
#6938 = AXIS2_PLACEMENT_3D ( 'NONE', #5273, #47827, #21172 ) ;
#6939 = DIRECTION ( 'NONE',  ( 0.000000000000000000, 0.000000000000000000, -1.000000000000000000 ) ) ;
#6940 = ORIENTED_EDGE ( 'NONE', *, *, #6175, .T. ) ;
#6941 = CARTESIAN_POINT ( 'NONE',  ( -164.9999999999987779, 16.00000000000000000, 30.00000000000000000 ) ) ;
#6942 = LINE ( 'NONE', #3079, #36393 ) ;
#6943 = VECTOR ( 'NONE', #26486, 1000.000000000000000 ) ;
#6944 = ORIENTED_EDGE ( 'NONE', *, *, #49981, .F. ) ;
#6945 = DIRECTION ( 'NONE',  ( -0.000000000000000000, -1.000000000000000000, 2.537652627714643577E-15 ) ) ;
#6946 = DIRECTION ( 'NONE',  ( 6.938893903907233308E-16, -1.000000000000000000, 0.000000000000000000 ) ) ;
#6947 = CARTESIAN_POINT ( 'NONE',  ( -47.72109971266203132, -1.750000000000010214, -80.20683870891910772 ) ) ;
#6948 = ORIENTED_EDGE ( 'NONE', *, *, #27087, .F. ) ;
#6949 = ORIENTED_EDGE ( 'NONE', *, *, #34297, .T. ) ;
#6950 = LINE ( 'NONE', #37275, #37422 ) ;
#6951 = CARTESIAN_POINT ( 'NONE',  ( -0.6677345994471270973, 1.504830332936299975, 9.927568724237746167 ) ) ;
#6952 = ORIENTED_EDGE ( 'NONE', *, *, #38542, .F. ) ;
#6953 = LINE ( 'NONE', #22603, #43922 ) ;
#6954 = AXIS2_PLACEMENT_3D ( 'NONE', #9415, #12996, #49122 ) ;
#6955 = CARTESIAN_POINT ( 'NONE',  ( 344.0000000000000000, -165.0000000000001137, -340.0000000000003411 ) ) ;
#6956 = ORIENTED_EDGE ( 'NONE', *, *, #7114, .F. ) ;
#6957 = CARTESIAN_POINT ( 'NONE',  ( 0.8155877869298099325, 0.9072449372238458043, 9.963925895597341764 ) ) ;
#6958 = ADVANCED_FACE ( 'NONE', ( #34519 ), #19094, .T. ) ;
#6959 = FACE_OUTER_BOUND ( 'NONE', #21472, .T. ) ;
#6960 = VERTEX_POINT ( 'NONE', #1644 ) ;
#6961 = AXIS2_PLACEMENT_3D ( 'NONE', #14530, #6844, #17871 ) ;
#6962 = CARTESIAN_POINT ( 'NONE',  ( 34.32915281903212446, -1.750000000000009326, -158.1565861772249377 ) ) ;
#6963 = CARTESIAN_POINT ( 'NONE',  ( -215.0000000000000568, 164.9999999999999716, 111.9999999999999858 ) ) ;
#6964 = DIRECTION ( 'NONE',  ( 0.8962124318248270161, -0.000000000000000000, 0.4436251537532894806 ) ) ;
#6965 = CARTESIAN_POINT ( 'NONE',  ( -225.0000000000000568, 164.9999999999999716, 498.0000000000001137 ) ) ;
#6966 = ORIENTED_EDGE ( 'NONE', *, *, #43237, .F. ) ;
#6967 = CARTESIAN_POINT ( 'NONE',  ( -23.26005729352344176, -44.90397804740339183, 7.906207997025717304 ) ) ;
#6968 = CARTESIAN_POINT ( 'NONE',  ( -0.3370904143228943828, -0.2449105217885308716, 10.00000000000000000 ) ) ;
#6969 = CARTESIAN_POINT ( 'NONE',  ( 36.08557433729230723, -35.58569447144768105, 7.455576670931136185 ) ) ;
#6970 = ORIENTED_EDGE ( 'NONE', *, *, #24303, .F. ) ;
#6971 = EDGE_CURVE ( 'NONE', #5052, #12618, #48285, .T. ) ;
#6972 = ORIENTED_EDGE ( 'NONE', *, *, #41993, .T. ) ;
#6973 = SHAPE_REPRESENTATION_RELATIONSHIP ( 'NONE' , 'NONE' ,  #41838, #12371 ) ;
#6974 = DIRECTION ( 'NONE',  ( 1.000000000000000000, -0.000000000000000000, -0.000000000000000000 ) ) ;
#6975 = CARTESIAN_POINT ( 'NONE',  ( -114.9999999999987779, 16.00000000000000000, 5.000000000000004441 ) ) ;
#6976 = LINE ( 'NONE', #25985, #39781 ) ;
#6977 = AXIS2_PLACEMENT_3D ( 'NONE', #21956, #45271, #37879 ) ;
#6978 = CARTESIAN_POINT ( 'NONE',  ( -114.9999999999991047, 17.00000000000000000, -24.99999999999999289 ) ) ;
#6979 = CARTESIAN_POINT ( 'NONE',  ( 181.0000000000000000, 165.0000000000000000, -360.0000000000002274 ) ) ;
#6980 = AXIS2_PLACEMENT_3D ( 'NONE', #13034, #17149, #44560 ) ;
#6981 = CARTESIAN_POINT ( 'NONE',  ( -167.4999999999999432, -102.5000000000000142, 10.00000000000000000 ) ) ;
#6982 = ORIENTED_EDGE ( 'NONE', *, *, #1231, .F. ) ;
#6983 = CARTESIAN_POINT ( 'NONE',  ( -164.9459734468149463, 2.143131898507880377E-16, 2.568287556927978166 ) ) ;
#6984 = CARTESIAN_POINT ( 'NONE',  ( -17.23491422248386584, 0.5912720620001978844, 8.727788335465566760 ) ) ;
#6985 = CARTESIAN_POINT ( 'NONE',  ( 344.0000000000000000, 174.9999999999996589, -340.0000000000002842 ) ) ;
#6986 = EDGE_CURVE ( 'NONE', #49939, #4452, #900, .T. ) ;
#6987 = VECTOR ( 'NONE', #26855, 999.9999999999998863 ) ;
#6988 = ORIENTED_EDGE ( 'NONE', *, *, #4509, .T. ) ;
#6989 = VECTOR ( 'NONE', #33249, 1000.000000000000000 ) ;
#6990 = VECTOR ( 'NONE', #17626, 1000.000000000000000 ) ;
#6991 = CARTESIAN_POINT ( 'NONE',  ( 13.35436367797824353, 31.26996044524050333, 7.906207997025717304 ) ) ;
#6992 = VERTEX_POINT ( 'NONE', #28834 ) ;
#6993 = DIRECTION ( 'NONE',  ( -1.000000000000000000, -0.000000000000000000, -0.000000000000000000 ) ) ;
#6994 = CARTESIAN_POINT ( 'NONE',  ( 1.288422560825904783, -0.1812466941682506494, 9.986087673579199020 ) ) ;
#6995 =( BOUNDED_CURVE ( )  B_SPLINE_CURVE ( 3, ( #36146, #32042, #5328, #4812 ),
 .UNSPECIFIED., .F., .F. ) 
 B_SPLINE_CURVE_WITH_KNOTS ( ( 4, 4 ),
 ( 1.570796326794896558, 3.141592653589793116 ),
 .UNSPECIFIED. ) 
 CURVE ( )  GEOMETRIC_REPRESENTATION_ITEM ( )  RATIONAL_B_SPLINE_CURVE ( ( 1.000000000000000000, 0.8047378541243649375, 0.8047378541243649375, 1.000000000000000000 ) ) 
 REPRESENTATION_ITEM ( '' )  );
#6996 = LINE ( 'NONE', #15633, #34336 ) ;
#6997 = CARTESIAN_POINT ( 'NONE',  ( 192.2789002873380184, -1.750000000000009548, -158.1565861772249377 ) ) ;
#6998 = AXIS2_PLACEMENT_3D ( 'NONE', #21667, #49075, #29623 ) ;
#6999 = EDGE_LOOP ( 'NONE', ( #43685, #44081, #35669 ) ) ;
#7000 = CARTESIAN_POINT ( 'NONE',  ( -1.173396789973005783, -0.3425192899591036344, 9.969517326150320713 ) ) ;
#7001 = ORIENTED_EDGE ( 'NONE', *, *, #26488, .T. ) ;
#7002 = CARTESIAN_POINT ( 'NONE',  ( 31.28234235046230793, 11.28615439405779064, -3.760136334089591248 ) ) ;
#7003 = CARTESIAN_POINT ( 'NONE',  ( -215.0000000000000568, 164.9999999999999716, 252.0000000000000000 ) ) ;
#7004 = CARTESIAN_POINT ( 'NONE',  ( -128.4459734468149463, -1.025126265847081664, 2.568287556927973281 ) ) ;
#7005 = ORIENTED_EDGE ( 'NONE', *, *, #25734, .T. ) ;
#7006 = ORIENTED_EDGE ( 'NONE', *, *, #48422, .F. ) ;
#7007 = DIRECTION ( 'NONE',  ( 0.000000000000000000, 0.000000000000000000, 1.000000000000000000 ) ) ;
#7008 = CARTESIAN_POINT ( 'NONE',  ( 0.4266413953668419246, 1.250184266969606162, 9.943883492372851407 ) ) ;
#7009 = B_SPLINE_CURVE_WITH_KNOTS ( 'NONE', 3,
 ( #15795, #16996, #46798, #35324 ),
 .UNSPECIFIED., .F., .F.,
 ( 4, 4 ),
 ( 4.165368725351569974E-18, 0.0004170521429101314869 ),
 .UNSPECIFIED. ) ;
#7010 = VECTOR ( 'NONE', #50048, 1000.000000000000000 ) ;
#7011 = EDGE_CURVE ( 'NONE', #38516, #12576, #35810, .T. ) ;
#7012 = VERTEX_POINT ( 'NONE', #40141 ) ;
#7013 = EDGE_CURVE ( 'NONE', #10841, #48741, #23901, .T. ) ;
#7014 = VERTEX_POINT ( 'NONE', #32957 ) ;
#7015 = CARTESIAN_POINT ( 'NONE',  ( -4.945973446814903696, 2.143131898507912917E-16, -157.4317124430720014 ) ) ;
#7016 = CARTESIAN_POINT ( 'NONE',  ( -208.1473046169136580, -154.8119894309599260, 22.84256005001721945 ) ) ;
#7017 = CARTESIAN_POINT ( 'NONE',  ( 342.0000000000000568, 169.0000000000000000, 343.9999999999998863 ) ) ;
#7018 = VECTOR ( 'NONE', #42228, 1000.000000000000000 ) ;
#7019 = ORIENTED_EDGE ( 'NONE', *, *, #26508, .F. ) ;
#7020 = DIRECTION ( 'NONE',  ( 1.000000000000000000, 0.000000000000000000, -4.625929269271635797E-16 ) ) ;
#7021 = EDGE_CURVE ( 'NONE', #3215, #33964, #44425, .T. ) ;
#7022 = ORIENTED_EDGE ( 'NONE', *, *, #2380, .T. ) ;
#7023 = CIRCLE ( 'NONE', #2084, 4.000000000000003553 ) ;
#7024 = DIRECTION ( 'NONE',  ( -0.000000000000000000, -0.000000000000000000, -1.000000000000000000 ) ) ;
#7025 = EDGE_CURVE ( 'NONE', #25245, #16715, #4973, .T. ) ;
#7026 = CARTESIAN_POINT ( 'NONE',  ( 30.00000000000123279, 16.00000000000000000, 5.000000000000004441 ) ) ;
#7027 = EDGE_CURVE ( 'NONE', #24412, #17736, #1397, .T. ) ;
#7029 = VECTOR ( 'NONE', #43294, 1000.000000000000000 ) ;
#7028 = CARTESIAN_POINT ( 'NONE',  ( 4.672045878990125800, -33.19353511768168374, 1.847720168420772691 ) ) ;
#7030 = ORIENTED_EDGE ( 'NONE', *, *, #23116, .T. ) ;
#7031 = ORIENTED_EDGE ( 'NONE', *, *, #37246, .T. ) ;
#7032 = MECHANICAL_DESIGN_GEOMETRIC_PRESENTATION_REPRESENTATION (  '', ( #14427 ), #17686 ) ;
#7033 = ORIENTED_EDGE ( 'NONE', *, *, #8020, .T. ) ;
#7034 = LINE ( 'NONE', #3159, #47970 ) ;
#7035 = DIRECTION ( 'NONE',  ( -0.000000000000000000, -0.000000000000000000, -1.000000000000000000 ) ) ;
#7036 = VERTEX_POINT ( 'NONE', #36047 ) ;
#7037 = CARTESIAN_POINT ( 'NONE',  ( -36.76598589393961447, -7.383243274241610088, -8.192531242611266862 ) ) ;
#7038 = ORIENTED_EDGE ( 'NONE', *, *, #10197, .F. ) ;
#7039 = AXIS2_PLACEMENT_3D ( 'NONE', #2738, #38174, #34065 ) ;
#7040 = VECTOR ( 'NONE', #15019, 1000.000000000000000 ) ;
#7041 = CYLINDRICAL_SURFACE ( 'NONE', #48743, 1.750000000000015543 ) ;
#7042 = DIRECTION ( 'NONE',  ( 0.000000000000000000, 0.000000000000000000, -1.000000000000000000 ) ) ;
#7043 = ORIENTED_EDGE ( 'NONE', *, *, #3490, .T. ) ;
#7044 = CARTESIAN_POINT ( 'NONE',  ( -36.08557433729205144, 35.58569447144795816, 7.455576670931136185 ) ) ;
#7045 = CARTESIAN_POINT ( 'NONE',  ( 113.3040265531850537, -1.749999999999997113, -39.18171244307202983 ) ) ;
#7046 = CARTESIAN_POINT ( 'NONE',  ( -46.76852358249002606, 17.86468378716741512, -9.367992836599954742 ) ) ;
#7047 = CARTESIAN_POINT ( 'NONE',  ( 39.35269538308637038, 47.68801056904006685, 742.8425600500171413 ) ) ;
#7048 = DIRECTION ( 'NONE',  ( -0.000000000000000000, -0.000000000000000000, -1.000000000000000000 ) ) ;
#7049 = ORIENTED_EDGE ( 'NONE', *, *, #42164, .F. ) ;
#7050 = CARTESIAN_POINT ( 'NONE',  ( 155.0540265531850537, 2.143131898507880377E-16, 119.0682875569279702 ) ) ;
#7051 = CARTESIAN_POINT ( 'NONE',  ( 0.4830800013901592194, 1.200413232422924192, 9.947020512645421420 ) ) ;
#7052 = CARTESIAN_POINT ( 'NONE',  ( 4.592425496802573972E-16, 13.98684210526316107, 3.750000000000000000 ) ) ;
#7053 = CARTESIAN_POINT ( 'NONE',  ( -30.21887974406478250, 14.69854701517550666, -8.016098858316199838 ) ) ;
#7054 = EDGE_CURVE ( 'NONE', #18098, #24636, #23525, .T. ) ;
#7055 = EDGE_CURVE ( 'NONE', #48040, #20500, #12670, .T. ) ;
#7056 = EDGE_CURVE ( 'NONE', #38020, #1662, #894, .T. ) ;
#7057 = EDGE_CURVE ( 'NONE', #36214, #38997, #14314, .T. ) ;
#7058 = CARTESIAN_POINT ( 'NONE',  ( -49.46074318306826001, 9.578883844007169301, 8.807470649214879543 ) ) ;
#7059 = VECTOR ( 'NONE', #43429, 1000.000000000000000 ) ;
#7060 = CARTESIAN_POINT ( 'NONE',  ( 0.3862712429686894766, -1.188820645368940276, 10.00000000000000000 ) ) ;
#7061 = EDGE_CURVE ( 'NONE', #16247, #22924, #31945, .T. ) ;
#7062 = EDGE_CURVE ( 'NONE', #35881, #31952, #32188, .T. ) ;
#7063 = CARTESIAN_POINT ( 'NONE',  ( 80.00000000000153477, 16.00000000000000000, 35.00000000000000000 ) ) ;
#7064 = ORIENTED_EDGE ( 'NONE', *, *, #11770, .T. ) ;
#7065 = AXIS2_PLACEMENT_3D ( 'NONE', #37030, #21087, #9547 ) ;
#7066 = DIRECTION ( 'NONE',  ( 0.000000000000000000, 0.000000000000000000, 1.000000000000000000 ) ) ;
#7067 = VECTOR ( 'NONE', #31546, 999.9999999999998863 ) ;
#7068 = CARTESIAN_POINT ( 'NONE',  ( -22.69295089195507487, -45.31600496604688999, 7.455576670931136185 ) ) ;
#7069 = LINE ( 'NONE', #34524, #16835 ) ;
#7070 = EDGE_LOOP ( 'NONE', ( #30297, #22034, #27610, #48993 ) ) ;
#7071 = EDGE_LOOP ( 'NONE', ( #32883, #14586, #31441, #8056, #17554 ) ) ;
#7072 = EDGE_CURVE ( 'NONE', #10836, #29314, #38926, .T. ) ;
#7073 = CARTESIAN_POINT ( 'NONE',  ( 342.0000000000000000, 175.0000000000000284, -94.00000000000019895 ) ) ;
#7074 = CIRCLE ( 'NONE', #46377, 1.750000000000001554 ) ;
#7075 = CARTESIAN_POINT ( 'NONE',  ( 181.0000000000000284, -174.9999999999999716, -111.0000000000001563 ) ) ;
#7076 = EDGE_CURVE ( 'NONE', #46979, #1473, #50064, .T. ) ;
#7077 = ORIENTED_EDGE ( 'NONE', *, *, #18745, .F. ) ;
#7078 = EDGE_CURVE ( 'NONE', #3283, #35970, #43964, .T. ) ;
#7079 = VERTEX_POINT ( 'NONE', #4727 ) ;
#7080 = CARTESIAN_POINT ( 'NONE',  ( -84.94597344681497475, 0.000000000000000000, 162.5682875569279702 ) ) ;
#7081 = FACE_OUTER_BOUND ( 'NONE', #49441, .T. ) ;
#7082 = ORIENTED_EDGE ( 'NONE', *, *, #46969, .T. ) ;
#7083 = VERTEX_POINT ( 'NONE', #20369 ) ;
#7084 = ORIENTED_EDGE ( 'NONE', *, *, #10641, .F. ) ;
#7085 = LINE ( 'NONE', #26072, #42180 ) ;
#7086 = CARTESIAN_POINT ( 'NONE',  ( -8.445973446814964092, -1.025126265847097651, 122.5682875569280128 ) ) ;
#7087 = CARTESIAN_POINT ( 'NONE',  ( 168.9999999999999716, -5.999999999999950262, -340.0000000000001137 ) ) ;
#7088 = EDGE_LOOP ( 'NONE', ( #18910, #15695, #45340, #12088 ) ) ;
#7089 = DIRECTION ( 'NONE',  ( -0.000000000000000000, -0.000000000000000000, -1.000000000000000000 ) ) ;
#7090 = VECTOR ( 'NONE', #19056, 1000.000000000000000 ) ;
#7091 = CARTESIAN_POINT ( 'NONE',  ( 35.00000000000152767, 16.00000000000000000, 60.00000000000000000 ) ) ;
#7092 = CARTESIAN_POINT ( 'NONE',  ( 1.133908876584335257, 0.5183204401656757998, 9.981352469109932457 ) ) ;
#7093 = ORIENTED_EDGE ( 'NONE', *, *, #37841, .T. ) ;
#7094 = ORIENTED_EDGE ( 'NONE', *, *, #15775, .F. ) ;
#7095 = EDGE_CURVE ( 'NONE', #22294, #39423, #47781, .T. ) ;
#7096 = DIRECTION ( 'NONE',  ( 0.000000000000000000, 1.000000000000000000, 0.000000000000000000 ) ) ;
#7097 = CARTESIAN_POINT ( 'NONE',  ( -46.69597344681494633, 1.750000000000010214, -39.18171244307202983 ) ) ;
#7098 = ORIENTED_EDGE ( 'NONE', *, *, #45095, .F. ) ;
#7099 = EDGE_LOOP ( 'NONE', ( #38413, #49678, #30253, #13879 ) ) ;
#7100 = CARTESIAN_POINT ( 'NONE',  ( 74.32915281903215998, 1.750000000000009548, -160.2068387089191219 ) ) ;
#7101 = CARTESIAN_POINT ( 'NONE',  ( 153.3040265531850537, 1.750000000000010658, -119.1817124430720440 ) ) ;
#7102 = VECTOR ( 'NONE', #41042, 1000.000000000000000 ) ;
#7103 = LINE ( 'NONE', #4009, #35899 ) ;
#7104 = LINE ( 'NONE', #26851, #48313 ) ;
#7105 = EDGE_CURVE ( 'NONE', #23986, #41219, #12962, .T. ) ;
#7106 = LINE ( 'NONE', #2985, #15070 ) ;
#7107 = VERTEX_POINT ( 'NONE', #33701 ) ;
#7108 = CARTESIAN_POINT ( 'NONE',  ( 135.0000000000000000, 16.00000000000000000, -114.9999999999999858 ) ) ;
#7109 = DIRECTION ( 'NONE',  ( 0.000000000000000000, 0.000000000000000000, -1.000000000000000000 ) ) ;
#7110 = CARTESIAN_POINT ( 'NONE',  ( -124.9459734468149463, 2.143131898507847836E-16, -37.43171244307205825 ) ) ;
#7111 = AXIS2_PLACEMENT_3D ( 'NONE', #17910, #49435, #25892 ) ;
#7112 = CARTESIAN_POINT ( 'NONE',  ( -225.0000000000000568, 175.0000000000000000, 0.000000000000000000 ) ) ;
#7113 = EDGE_CURVE ( 'NONE', #7866, #1662, #37840, .T. ) ;
#7114 = EDGE_CURVE ( 'NONE', #20701, #39523, #30456, .T. ) ;
#7115 = VERTEX_POINT ( 'NONE', #9832 ) ;
#7116 = CARTESIAN_POINT ( 'NONE',  ( 3.229232847726260403, -16.57333684275945629, 9.178419661560148768 ) ) ;
#7117 = EDGE_CURVE ( 'NONE', #36660, #2139, #21899, .T. ) ;
#7118 = CYLINDRICAL_SURFACE ( 'NONE', #25047, 1.750000000000001554 ) ;
#7119 = CARTESIAN_POINT ( 'NONE',  ( -64.99999999999877787, 17.00000000000000000, 5.000000000000004441 ) ) ;
#7120 = ADVANCED_FACE ( 'NONE', ( #45456 ), #10350, .T. ) ;
#7121 = EDGE_CURVE ( 'NONE', #4802, #24870, #29612, .T. ) ;
#7122 = ORIENTED_EDGE ( 'NONE', *, *, #24961, .T. ) ;
#7123 = CARTESIAN_POINT ( 'NONE',  ( 210.0000000000000568, 0.000000000000000000, 120.8182875569279702 ) ) ;
#7124 = VECTOR ( 'NONE', #24884, 1000.000000000000000 ) ;
#7125 = CARTESIAN_POINT ( 'NONE',  ( -4.945973446814903696, 2.143131898507912917E-16, -77.43171244307198720 ) ) ;
#7126 = VERTEX_POINT ( 'NONE', #6249 ) ;
#7127 = CARTESIAN_POINT ( 'NONE',  ( 111.5540265531850537, 0.000000000000000000, 162.5682875569279702 ) ) ;
#7128 = CARTESIAN_POINT ( 'NONE',  ( 0.6440276692615867216, 16.64212148744554298, -9.683996418299976483 ) ) ;
#7129 = CARTESIAN_POINT ( 'NONE',  ( -164.9999999999984936, 17.00000000000000000, 60.00000000000000000 ) ) ;
#7130 = DIRECTION ( 'NONE',  ( 0.000000000000000000, 1.000000000000000000, 0.000000000000000000 ) ) ;
#7131 = EDGE_CURVE ( 'NONE', #2021, #1277, #1891, .T. ) ;
#7132 = VERTEX_POINT ( 'NONE', #45704 ) ;
#7133 = CARTESIAN_POINT ( 'NONE',  ( -7.749480817862350435, -14.85497772329513211, 9.403735324607438884 ) ) ;
#7134 = ORIENTED_EDGE ( 'NONE', *, *, #30959, .T. ) ;
#7135 = ORIENTED_EDGE ( 'NONE', *, *, #24647, .F. ) ;
#7136 = DIRECTION ( 'NONE',  ( 0.000000000000000000, 1.000000000000000000, 0.000000000000000000 ) ) ;
#7137 =( BOUNDED_CURVE ( )  B_SPLINE_CURVE ( 3, ( #32252, #33014, #44271, #12978 ),
 .UNSPECIFIED., .F., .F. ) 
 B_SPLINE_CURVE_WITH_KNOTS ( ( 4, 4 ),
 ( 3.141592653589793116, 4.712388980384689674 ),
 .UNSPECIFIED. ) 
 CURVE ( )  GEOMETRIC_REPRESENTATION_ITEM ( )  RATIONAL_B_SPLINE_CURVE ( ( 1.000000000000000000, 0.8047378541243649375, 0.8047378541243649375, 1.000000000000000000 ) ) 
 REPRESENTATION_ITEM ( '' )  );
#7138 = ORIENTED_EDGE ( 'NONE', *, *, #11475, .F. ) ;
#7139 = DIRECTION ( 'NONE',  ( 0.000000000000000000, 0.000000000000000000, -1.000000000000000000 ) ) ;
#7140 = CARTESIAN_POINT ( 'NONE',  ( -17.23491422248386584, 0.5912720620001978844, 8.727788335465566760 ) ) ;
#7141 = LINE ( 'NONE', #15087, #36015 ) ;
#7142 =( BOUNDED_CURVE ( )  B_SPLINE_CURVE ( 3, ( #34653, #46655, #30804, #26184 ),
 .UNSPECIFIED., .F., .F. ) 
 B_SPLINE_CURVE_WITH_KNOTS ( ( 4, 4 ),
 ( 1.570796326794896558, 3.141592653589793116 ),
 .UNSPECIFIED. ) 
 CURVE ( )  GEOMETRIC_REPRESENTATION_ITEM ( )  RATIONAL_B_SPLINE_CURVE ( ( 1.000000000000000000, 0.8047378541243649375, 0.8047378541243649375, 1.000000000000000000 ) ) 
 REPRESENTATION_ITEM ( '' )  );
#7143 = CARTESIAN_POINT ( 'NONE',  ( 359.9999999999999432, -177.9999999999999147, -353.0000000000001137 ) ) ;
#7144 = VERTEX_POINT ( 'NONE', #45199 ) ;
#7145 = LINE ( 'NONE', #26129, #45450 ) ;
#7146 = CARTESIAN_POINT ( 'NONE',  ( 356.0000000000001137, 169.0000000000000000, 349.9999999999998295 ) ) ;
#7147 = CARTESIAN_POINT ( 'NONE',  ( -6.880036658038815922, -222.4999999999999716, -228.6347188485896140 ) ) ;
#7148 = ORIENTED_EDGE ( 'NONE', *, *, #25295, .T. ) ;
#7149 = CARTESIAN_POINT ( 'NONE',  ( 0.3862712429686815385, 1.188820645368943385, 9.972675548442461846 ) ) ;
#7150 = LINE ( 'NONE', #220, #42524 ) ;
#7151 = EDGE_LOOP ( 'NONE', ( #4995, #47656, #11427, #25624, #20511, #3983 ) ) ;
#7152 = ORIENTED_EDGE ( 'NONE', *, *, #42796, .T. ) ;
#7153 = ORIENTED_EDGE ( 'NONE', *, *, #14278, .F. ) ;
#7154 = CARTESIAN_POINT ( 'NONE',  ( 210.0000000000000568, 2.143131898507880377E-16, 159.0682875569279702 ) ) ;
#7155 =( BOUNDED_CURVE ( )  B_SPLINE_CURVE ( 3, ( #24230, #39891, #23200, #16269 ),
 .UNSPECIFIED., .F., .F. ) 
 B_SPLINE_CURVE_WITH_KNOTS ( ( 4, 4 ),
 ( 0.000000000000000000, 1.570796326794896558 ),
 .UNSPECIFIED. ) 
 CURVE ( )  GEOMETRIC_REPRESENTATION_ITEM ( )  RATIONAL_B_SPLINE_CURVE ( ( 1.000000000000000000, 0.8047378541243649375, 0.8047378541243649375, 1.000000000000000000 ) ) 
 REPRESENTATION_ITEM ( '' )  );
#7156 = CARTESIAN_POINT ( 'NONE',  ( 2.499999999999948930, -214.9999999999999716, -230.2499999999999716 ) ) ;
#7157 = ORIENTED_EDGE ( 'NONE', *, *, #45119, .F. ) ;
#7158 = EDGE_CURVE ( 'NONE', #9291, #50718, #38060, .T. ) ;
#7159 = CYLINDRICAL_SURFACE ( 'NONE', #24996, 1.749999999999987566 ) ;
#7160 = CARTESIAN_POINT ( 'NONE',  ( 113.3040265531850537, 1.749999999999997335, 80.81828755692798438 ) ) ;
#7161 = DIRECTION ( 'NONE',  ( 0.000000000000000000, -1.000000000000000000, 0.000000000000000000 ) ) ;
#7162 = CYLINDRICAL_SURFACE ( 'NONE', #26825, 1.749999999999987566 ) ;
#7163 = CARTESIAN_POINT ( 'NONE',  ( -88.44597344681497475, 0.000000000000000000, 82.56828755692801280 ) ) ;
#7164 = VECTOR ( 'NONE', #47655, 1000.000000000000000 ) ;
#7165 = CARTESIAN_POINT ( 'NONE',  ( 33.30402655318503946, -1.750000000000010214, -39.18171244307202983 ) ) ;
#7166 = CARTESIAN_POINT ( 'NONE',  ( -206.6959734468149463, 0.000000000000000000, 165.0000000000000000 ) ) ;
#7167 = LINE ( 'NONE', #18694, #25939 ) ;
#7168 = CARTESIAN_POINT ( 'NONE',  ( -10.30302290646040575, -13.08520913973572419, -9.683996418299976483 ) ) ;
#7169 = VERTEX_POINT ( 'NONE', #5983 ) ;
#7170 = DIRECTION ( 'NONE',  ( -0.000000000000000000, -0.000000000000000000, -1.000000000000000000 ) ) ;
#7171 = CARTESIAN_POINT ( 'NONE',  ( 1.228394325311184421, -1.341866297401743235, 9.903764339332088440 ) ) ;
#7172 = ADVANCED_FACE ( 'NONE', ( #10584 ), #45254, .T. ) ;
#7173 = EDGE_CURVE ( 'NONE', #24207, #33697, #45959, .T. ) ;
#7174 = CARTESIAN_POINT ( 'NONE',  ( 112.2789002873379758, 1.749999999999996225, 1.843413822775058497 ) ) ;
#7175 = LINE ( 'NONE', #34141, #29751 ) ;
#7176 = ORIENTED_EDGE ( 'NONE', *, *, #48271, .T. ) ;
#7177 = DIRECTION ( 'NONE',  ( -1.000000000000000000, -0.000000000000000000, -0.000000000000000000 ) ) ;
#7178 = CARTESIAN_POINT ( 'NONE',  ( -0.3862712429686889770, 1.188820645368940720, 9.972675548442463622 ) ) ;
#7179 = ADVANCED_FACE ( 'NONE', ( #29340 ), #44949, .F. ) ;
#7180 = CARTESIAN_POINT ( 'NONE',  ( 0.3862712429686727678, 1.188820645368945605, -3.333333333333333481 ) ) ;
#7181 = CARTESIAN_POINT ( 'NONE',  ( -128.4459734468149463, 1.025126265847081664, 122.5682875569279702 ) ) ;
#7182 = CARTESIAN_POINT ( 'NONE',  ( 30.00000000000187228, 16.00000000000000000, 90.00000000000000000 ) ) ;
#7183 = ADVANCED_FACE ( 'NONE', ( #10089 ), #25746, .F. ) ;
#7184 = EDGE_CURVE ( 'NONE', #36250, #43432, #35481, .T. ) ;
#7185 = ORIENTED_EDGE ( 'NONE', *, *, #31190, .T. ) ;
#7186 = PRESENTATION_STYLE_ASSIGNMENT (( #42325 ) ) ;
#7187 = ORIENTED_EDGE ( 'NONE', *, *, #16757, .T. ) ;
#7188 = CARTESIAN_POINT ( 'NONE',  ( 71.55402655318505367, 0.000000000000000000, 42.56828755692799859 ) ) ;
#7189 = ORIENTED_EDGE ( 'NONE', *, *, #13566, .T. ) ;
#7190 = EDGE_CURVE ( 'NONE', #36, #10961, #38821, .T. ) ;
#7191 = FACE_OUTER_BOUND ( 'NONE', #24159, .T. ) ;
#7192 = CARTESIAN_POINT ( 'NONE',  ( 210.0000000000000568, 0.000000000000000000, -119.1817124430720440 ) ) ;
#7193 = ORIENTED_EDGE ( 'NONE', *, *, #49595, .F. ) ;
#7194 = FILL_AREA_STYLE_COLOUR ( '', #50194 ) ;
#7195 = ORIENTED_EDGE ( 'NONE', *, *, #31485, .F. ) ;
#7196 = VECTOR ( 'NONE', #29436, 1000.000000000000000 ) ;
#7197 = ORIENTED_EDGE ( 'NONE', *, *, #25233, .F. ) ;
#7198 = LINE ( 'NONE', #49492, #48275 ) ;
#7199 = DIRECTION ( 'NONE',  ( 1.000000000000000000, -0.000000000000000000, 0.000000000000000000 ) ) ;
#7200 = VERTEX_POINT ( 'NONE', #19803 ) ;
#7201 = CARTESIAN_POINT ( 'NONE',  ( 210.0000000000000568, 2.143131898507881856E-16, 79.06828755692797017 ) ) ;
#7202 = DIRECTION ( 'NONE',  ( -1.000000000000000000, -6.938893903907233308E-16, 0.000000000000000000 ) ) ;
#7203 = CARTESIAN_POINT ( 'NONE',  ( -46.69597344681494633, 1.750000000000009992, 0.8182875569279768335 ) ) ;
#7204 = ORIENTED_EDGE ( 'NONE', *, *, #50260, .F. ) ;
#7205 = ORIENTED_EDGE ( 'NONE', *, *, #50324, .T. ) ;
#7206 = CYLINDRICAL_SURFACE ( 'NONE', #49611, 1.750000000000001554 ) ;
#7207 = B_SPLINE_CURVE_WITH_KNOTS ( 'NONE', 3,
 ( #1374, #39615, #16009, #12399 ),
 .UNSPECIFIED., .F., .F.,
 ( 4, 4 ),
 ( 3.388966592816271738E-16, 0.009782300387714822770 ),
 .UNSPECIFIED. ) ;
#7208 = DIRECTION ( 'NONE',  ( 0.000000000000000000, -1.000000000000000000, 0.000000000000000000 ) ) ;
#7209 = ORIENTED_EDGE ( 'NONE', *, *, #13339, .F. ) ;
#7210 = DIRECTION ( 'NONE',  ( 0.000000000000000000, 1.000000000000000000, 1.544785076050074834E-48 ) ) ;
#7211 = DIRECTION ( 'NONE',  ( 0.000000000000000000, -0.000000000000000000, 1.000000000000000000 ) ) ;
#7212 = ORIENTED_EDGE ( 'NONE', *, *, #9729, .T. ) ;
#7213 = CARTESIAN_POINT ( 'NONE',  ( 210.0000000000000568, 0.000000000000000000, 120.8182875569279702 ) ) ;
#7214 = EDGE_CURVE ( 'NONE', #47457, #48103, #7745, .T. ) ;
#7215 = CARTESIAN_POINT ( 'NONE',  ( 341.9999999999999432, -181.0000000000001705, -356.0000000000003411 ) ) ;
#7216 = B_SPLINE_SURFACE_WITH_KNOTS ( 'NONE', 3, 3, ( 
 ( #24822, #40475, #44793, #48116 ),
 ( #5311, #48369, #35880, #12999 ),
 ( #28916, #13508, #29178, #20211 ),
 ( #4795, #9666, #16359, #39979 ) ),
 .UNSPECIFIED., .F., .F., .F.,
 ( 4, 4 ),
 ( 4, 4 ),
 ( 0.000000000000000000, 1.000000000000000000 ),
 ( 0.000000000000000000, 1.000000000000000000 ),
 .UNSPECIFIED. ) ;
#7217 = ORIENTED_EDGE ( 'NONE', *, *, #1371, .F. ) ;
#7218 = EDGE_CURVE ( 'NONE', #10836, #2436, #10717, .T. ) ;
#7219 = CARTESIAN_POINT ( 'NONE',  ( 181.0000000000000284, -174.9999999999999716, -99.00000000000014211 ) ) ;
#7220 = CARTESIAN_POINT ( 'NONE',  ( -128.4459734468149179, 0.000000000000000000, -77.43171244307204404 ) ) ;
#7221 = DIRECTION ( 'NONE',  ( 1.000000000000000000, 0.000000000000000000, 0.000000000000000000 ) ) ;
#7222 = CARTESIAN_POINT ( 'NONE',  ( -14.99999999999937472, 17.00000000000000000, -54.99999999999999289 ) ) ;
#7223 = VERTEX_POINT ( 'NONE', #23415 ) ;
#7224 = CARTESIAN_POINT ( 'NONE',  ( 16.69947034530964913, -2.312583065866261389, 2.590526750877053086 ) ) ;
#7225 = CARTESIAN_POINT ( 'NONE',  ( 113.3040265531850537, 1.749999999999996891, 0.8182875569279768335 ) ) ;
#7226 = CARTESIAN_POINT ( 'NONE',  ( 27.33593271309472073, -41.94268121623323964, -9.367992836599954742 ) ) ;
#7227 = VERTEX_POINT ( 'NONE', #3902 ) ;
#7228 = VERTEX_POINT ( 'NONE', #31108 ) ;
#7229 = DIRECTION ( 'NONE',  ( 0.9976107099581962290, -4.447988690094344769E-15, -0.06908597091091817077 ) ) ;
#7230 = DIRECTION ( 'NONE',  ( -9.711650524620651178E-33, 1.223873602809432483E-48, -1.000000000000000000 ) ) ;
#7231 = LINE ( 'NONE', #39497, #27709 ) ;
#7232 = CARTESIAN_POINT ( 'NONE',  ( 342.0000000000000568, 181.0000000000000568, 355.9999999999998295 ) ) ;
#7233 = AXIS2_PLACEMENT_3D ( 'NONE', #50019, #14927, #47382 ) ;
#7234 = SURFACE_STYLE_FILL_AREA ( #7747 ) ;
#7235 = DIRECTION ( 'NONE',  ( 1.000000000000000000, 0.000000000000000000, -4.758098676964956461E-16 ) ) ;
#7236 = FACE_OUTER_BOUND ( 'NONE', #16008, .T. ) ;
#7237 = ORIENTED_EDGE ( 'NONE', *, *, #8244, .T. ) ;
#7238 = CARTESIAN_POINT ( 'NONE',  ( 195.0540265531851105, 2.143131898507880377E-16, 119.0682875569279702 ) ) ;
#7239 = DIRECTION ( 'NONE',  ( -1.000000000000000000, -0.000000000000000000, -0.000000000000000000 ) ) ;
#7240 = CARTESIAN_POINT ( 'NONE',  ( -5.000000000000000000, -184.7999999999999545, -359.8000000000002387 ) ) ;
#7241 = DIRECTION ( 'NONE',  ( 2.958228394578794708E-31, 0.000000000000000000, -1.000000000000000000 ) ) ;
#7242 = EDGE_LOOP ( 'NONE', ( #23431, #35818, #42706, #49198 ) ) ;
#7243 = FACE_BOUND ( 'NONE', #35835, .T. ) ;
#7244 = CARTESIAN_POINT ( 'NONE',  ( -1.011271242968693862, 0.7347315653655780432, 10.00000000000000000 ) ) ;
#7245 = ORIENTED_EDGE ( 'NONE', *, *, #13949, .F. ) ;
#7246 = ADVANCED_FACE ( 'NONE', ( #19296 ), #35226, .T. ) ;
#7247 = LINE ( 'NONE', #14168, #1635 ) ;
#7248 = CARTESIAN_POINT ( 'NONE',  ( 344.0000000000000568, 165.0000000000000000, 339.9999999999998295 ) ) ;
#7249 = CARTESIAN_POINT ( 'NONE',  ( 21.23829395927641883, -7.388441598285492518, 230.0000000000000000 ) ) ;
#7250 = ORIENTED_EDGE ( 'NONE', *, *, #38192, .F. ) ;
#7251 = B_SPLINE_CURVE_WITH_KNOTS ( 'NONE', 3,
 ( #1802, #9490, #45370, #48695 ),
 .UNSPECIFIED., .F., .F.,
 ( 4, 4 ),
 ( 0.7491799374948677759, 1.000000000000000000 ),
 .UNSPECIFIED. ) ;
#7252 = DIRECTION ( 'NONE',  ( 0.000000000000000000, 0.000000000000000000, 1.000000000000000000 ) ) ;
#7253 = DIRECTION ( 'NONE',  ( 0.000000000000000000, 2.969158215481698263E-48, -1.000000000000000000 ) ) ;
#7254 = ORIENTED_EDGE ( 'NONE', *, *, #24579, .F. ) ;
#7255 = CARTESIAN_POINT ( 'NONE',  ( 193.3040265531851105, -1.750000000000009992, 160.8182875569279702 ) ) ;
#7256 = CARTESIAN_POINT ( 'NONE',  ( 210.0000000000000568, 0.000000000000000000, -39.18171244307202983 ) ) ;
#7257 = DIRECTION ( 'NONE',  ( 0.000000000000000000, 1.000000000000000000, -1.604368532695312981E-16 ) ) ;
#7258 = VERTEX_POINT ( 'NONE', #46714 ) ;
#7259 = VERTEX_POINT ( 'NONE', #7511 ) ;
#7260 = CARTESIAN_POINT ( 'NONE',  ( -0.8965959638259611841, -1.582931917743307215, 9.903764339332084887 ) ) ;
#7261 = CARTESIAN_POINT ( 'NONE',  ( 113.3040265531850537, -1.749999999999997335, -79.18171244307201562 ) ) ;
#7262 = CIRCLE ( 'NONE', #37614, 2.000000000000001776 ) ;
#7263 = ORIENTED_EDGE ( 'NONE', *, *, #37324, .F. ) ;
#7264 = ORIENTED_EDGE ( 'NONE', *, *, #22227, .F. ) ;
#7265 = CARTESIAN_POINT ( 'NONE',  ( 75.05402655318509630, 1.025126265847089213, -0.9317124430720324924 ) ) ;
#7266 = LINE ( 'NONE', #22913, #46353 ) ;
#7267 = CYLINDRICAL_SURFACE ( 'NONE', #19020, 1.750000000000001554 ) ;
#7268 = ORIENTED_EDGE ( 'NONE', *, *, #22763, .T. ) ;
#7269 = CARTESIAN_POINT ( 'NONE',  ( -164.9999999999984936, 16.00000000000000000, 60.00000000000000000 ) ) ;
#7270 = EDGE_LOOP ( 'NONE', ( #25862, #6224, #367, #44266, #66, #9102 ) ) ;
#7271 = DIRECTION ( 'NONE',  ( 1.000000000000000000, 0.000000000000000000, 0.000000000000000000 ) ) ;
#7272 = CLOSED_SHELL ( 'NONE', ( #18927, #43714, #46822, #342, #22177, #23686, #28004, #1750, #42808, #41362, #48697, #26015, #11744, #28368, #23224, #43415, #21259, #19388, #38381, #50269, #18972, #16515, #14568, #10938, #44795, #41279, #17789, #42653, #44036, #37273, #10881, #10910, #41826, #39115, #8876, #16811, #36818 ) ) ;
#7273 = EDGE_CURVE ( 'NONE', #28229, #5824, #15967, .T. ) ;
#7274 = CARTESIAN_POINT ( 'NONE',  ( 168.9999999999998863, -164.9999999999999432, 357.9999999999998863 ) ) ;
#7275 = FACE_OUTER_BOUND ( 'NONE', #21467, .T. ) ;
#7276 = ORIENTED_EDGE ( 'NONE', *, *, #5130, .F. ) ;
#7277 = VERTEX_POINT ( 'NONE', #11612 ) ;
#7278 = ORIENTED_EDGE ( 'NONE', *, *, #8105, .F. ) ;
#7279 = CARTESIAN_POINT ( 'NONE',  ( 350.0000000000000000, -174.9999999999999716, 349.9999999999998295 ) ) ;
#7280 = CARTESIAN_POINT ( 'NONE',  ( -0.2458784654125648617, -0.3384226744270785181, 9.992713367193012175 ) ) ;
#7281 = DIRECTION ( 'NONE',  ( -0.000000000000000000, -0.000000000000000000, -1.000000000000000000 ) ) ;
#7282 = ORIENTED_EDGE ( 'NONE', *, *, #32740, .F. ) ;
#7283 = CARTESIAN_POINT ( 'NONE',  ( 165.0000000000000284, 175.0000000000000284, 355.9999999999998863 ) ) ;
#7284 = ORIENTED_EDGE ( 'NONE', *, *, #27754, .T. ) ;
#7285 = DIRECTION ( 'NONE',  ( 0.000000000000000000, 0.000000000000000000, -1.000000000000000000 ) ) ;
#7286 = ORIENTED_EDGE ( 'NONE', *, *, #17752, .F. ) ;
#7287 = CARTESIAN_POINT ( 'NONE',  ( -206.6959734468149463, 1.750000000000009992, 0.8182875569279768335 ) ) ;
#7288 = CARTESIAN_POINT ( 'NONE',  ( -194.9999999999999432, 173.0000000000000000, 112.0000000000000000 ) ) ;
#7289 = CARTESIAN_POINT ( 'NONE',  ( -0.3862712429686809279, -1.188820645368943163, 10.00000000000000000 ) ) ;
#7290 = CARTESIAN_POINT ( 'NONE',  ( 210.0000000000000568, 0.000000000000000000, 160.8182875569279702 ) ) ;
#7291 = CARTESIAN_POINT ( 'NONE',  ( 210.0000000000000568, 2.143131898507881116E-16, -40.93171244307203693 ) ) ;
#7292 = ORIENTED_EDGE ( 'NONE', *, *, #22439, .T. ) ;
#7293 = CARTESIAN_POINT ( 'NONE',  ( -0.7601424845489993531, 1.297311920617006065, 9.927319414211224213 ) ) ;
#7294 = CARTESIAN_POINT ( 'NONE',  ( -64.99999999999909051, 17.00000000000000000, 0.000000000000000000 ) ) ;
#7295 =( BOUNDED_CURVE ( )  B_SPLINE_CURVE ( 3, ( #6111, #6361, #5859, #44831 ),
 .UNSPECIFIED., .F., .F. ) 
 B_SPLINE_CURVE_WITH_KNOTS ( ( 4, 4 ),
 ( 3.141592653589793116, 4.712388980384689674 ),
 .UNSPECIFIED. ) 
 CURVE ( )  GEOMETRIC_REPRESENTATION_ITEM ( )  RATIONAL_B_SPLINE_CURVE ( ( 1.000000000000000000, 0.8047378541243649375, 0.8047378541243649375, 1.000000000000000000 ) ) 
 REPRESENTATION_ITEM ( '' )  );
#7296 = CARTESIAN_POINT ( 'NONE',  ( 38.83576208387763273, -41.71198943095993172, 741.9425600500172777 ) ) ;
#7297 = LINE ( 'NONE', #7562, #14293 ) ;
#7298 = AXIS2_PLACEMENT_3D ( 'NONE', #29946, #45562, #18629 ) ;
#7299 = AXIS2_PLACEMENT_3D ( 'NONE', #39823, #317, #20301 ) ;
#7300 = LINE ( 'NONE', #11403, #6740 ) ;
#7301 = CARTESIAN_POINT ( 'NONE',  ( -45.64490844644706868, -21.32281559348764333, 8.807470649214879543 ) ) ;
#7302 = VECTOR ( 'NONE', #17266, 1000.000000000000000 ) ;
#7303 = AXIS2_PLACEMENT_3D ( 'NONE', #29237, #17918, #9984 ) ;
#7304 = ORIENTED_EDGE ( 'NONE', *, *, #23469, .F. ) ;
#7305 = EDGE_CURVE ( 'NONE', #11492, #35493, #948, .T. ) ;
#7306 = AXIS2_PLACEMENT_3D ( 'NONE', #34640, #28697, #4597 ) ;
#7307 = PLANE ( 'NONE',  #9822 ) ;
#7308 = DIRECTION ( 'NONE',  ( -1.000000000000000000, 0.000000000000000000, 0.000000000000000000 ) ) ;
#7309 = EDGE_CURVE ( 'NONE', #35301, #17811, #42130, .T. ) ;
#7310 = ORIENTED_EDGE ( 'NONE', *, *, #44305, .T. ) ;
#7311 = EDGE_CURVE ( 'NONE', #11806, #6011, #72, .T. ) ;
#7312 = FACE_OUTER_BOUND ( 'NONE', #1243, .T. ) ;
#7313 =( REPRESENTATION_RELATIONSHIP ('NONE','NONE', #45699, #50327 ) REPRESENTATION_RELATIONSHIP_WITH_TRANSFORMATION ( #29253 )SHAPE_REPRESENTATION_RELATIONSHIP( ) );
#7314 = DIRECTION ( 'NONE',  ( 0.000000000000000000, 1.000000000000000000, 0.000000000000000000 ) ) ;
#7315 = CARTESIAN_POINT ( 'NONE',  ( 73.30402655318508209, 1.750000000000010658, -119.1817124430720440 ) ) ;
#7316 = EDGE_CURVE ( 'NONE', #21384, #9147, #38320, .T. ) ;
#7317 = ADVANCED_FACE ( 'NONE', ( #18777 ), #31376, .T. ) ;
#7318 = VERTEX_POINT ( 'NONE', #46967 ) ;
#7319 = PRODUCT_DEFINITION_SHAPE ( 'NONE', 'NONE',  #50733 ) ;
#7320 = ORIENTED_EDGE ( 'NONE', *, *, #37487, .T. ) ;
#7321 = CARTESIAN_POINT ( 'NONE',  ( -2.569099690548740877, 50.00000000000000711, 3.199614146704519602 ) ) ;
#7322 = CARTESIAN_POINT ( 'NONE',  ( 71.55402655318505367, 0.000000000000000000, 119.0682875569279560 ) ) ;
#7323 = EDGE_CURVE ( 'NONE', #41885, #35737, #3130, .T. ) ;
#7324 = ORIENTED_EDGE ( 'NONE', *, *, #31534, .F. ) ;
#7325 = EDGE_LOOP ( 'NONE', ( #22359, #3712, #17058, #14186 ) ) ;
#7326 = CARTESIAN_POINT ( 'NONE',  ( -46.69597344681494633, 1.750000000000010214, -39.18171244307202983 ) ) ;
#7327 = CARTESIAN_POINT ( 'NONE',  ( 0.4166666666666669072, 0.000000000000000000, 10.00000000000000000 ) ) ;
#7328 = CARTESIAN_POINT ( 'NONE',  ( 350.0000000000000000, -184.9999999999999716, -340.0000000000001705 ) ) ;
#7329 = ORIENTED_EDGE ( 'NONE', *, *, #47497, .F. ) ;
#7330 = ORIENTED_EDGE ( 'NONE', *, *, #10247, .T. ) ;
#7331 = ORIENTED_EDGE ( 'NONE', *, *, #22390, .F. ) ;
#7332 = EDGE_CURVE ( 'NONE', #24760, #36401, #15981, .T. ) ;
#7333 = EDGE_CURVE ( 'NONE', #22392, #41767, #40279, .T. ) ;
#7334 = VECTOR ( 'NONE', #44332, 1000.000000000000000 ) ;
#7335 = CARTESIAN_POINT ( 'NONE',  ( -119.9999999999994174, 16.00000000000000000, -30.00000000000000000 ) ) ;
#7336 = AXIS2_PLACEMENT_3D ( 'NONE', #46828, #39694, #43771 ) ;
#7337 = CARTESIAN_POINT ( 'NONE',  ( -86.69597344681494633, 1.750000000000009992, 160.8182875569279702 ) ) ;
#7338 = EDGE_CURVE ( 'NONE', #27092, #43206, #30868, .T. ) ;
#7339 = ORIENTED_EDGE ( 'NONE', *, *, #15158, .F. ) ;
#7340 = EDGE_CURVE ( 'NONE', #1481, #23962, #43399, .T. ) ;
#7341 = AXIS2_PLACEMENT_3D ( 'NONE', #22381, #37317, #21894 ) ;
#7342 = FACE_OUTER_BOUND ( 'NONE', #47818, .T. ) ;
#7343 = CARTESIAN_POINT ( 'NONE',  ( 339.9999999999998863, -180.9999999999999716, 359.9999999999998295 ) ) ;
#7344 = CARTESIAN_POINT ( 'NONE',  ( 80.00000000000216005, 17.00000000000000000, 95.00000000000000000 ) ) ;
#7345 = ORIENTED_EDGE ( 'NONE', *, *, #41068, .T. ) ;
#7346 = ORIENTED_EDGE ( 'NONE', *, *, #8284, .F. ) ;
#7347 = CARTESIAN_POINT ( 'NONE',  ( 360.0000000000000000, 175.0000000000000284, -106.0000000000001990 ) ) ;
#7348 = VECTOR ( 'NONE', #22231, 1000.000000000000000 ) ;
#7349 = EDGE_CURVE ( 'NONE', #23722, #41220, #28274, .T. ) ;
#7350 = AXIS2_PLACEMENT_3D ( 'NONE', #7477, #23106, #16184 ) ;
#7351 = DIRECTION ( 'NONE',  ( 0.000000000000000000, 0.000000000000000000, -1.000000000000000000 ) ) ;
#7352 = ADVANCED_FACE ( 'NONE', ( #8527 ), #48906, .T. ) ;
#7353 = CARTESIAN_POINT ( 'NONE',  ( 210.0000000000000568, 0.000000000000000000, 160.8182875569279702 ) ) ;
#7354 = ORIENTED_EDGE ( 'NONE', *, *, #24488, .F. ) ;
#7355 = VERTEX_POINT ( 'NONE', #13790 ) ;
#7356 = DIRECTION ( 'NONE',  ( 0.000000000000000000, 0.000000000000000000, 1.000000000000000000 ) ) ;
#7357 = FACE_OUTER_BOUND ( 'NONE', #24249, .T. ) ;
#7358 = CARTESIAN_POINT ( 'NONE',  ( -44.94597344681493922, 2.143131898507880377E-16, 2.568287556927978166 ) ) ;
#7359 = DIRECTION ( 'NONE',  ( -1.000000000000000000, 0.000000000000000000, -0.000000000000000000 ) ) ;
#7360 = EDGE_LOOP ( 'NONE', ( #30920, #23282, #13409, #16400 ) ) ;
#7361 = LINE ( 'NONE', #49885, #2863 ) ;
#7362 = DIRECTION ( 'NONE',  ( -1.000000000000000000, 0.000000000000000000, 0.000000000000000000 ) ) ;
#7363 = CARTESIAN_POINT ( 'NONE',  ( -48.44597344681495343, 0.000000000000000000, -117.4317124430720156 ) ) ;
#7364 = CARTESIAN_POINT ( 'NONE',  ( 153.3040265531850537, -1.750000000000010214, -39.18171244307202983 ) ) ;
#7365 = ADVANCED_FACE ( 'NONE', ( #12606 ), #20312, .T. ) ;
#7366 = CARTESIAN_POINT ( 'NONE',  ( 35.00000000000028422, 17.00000000000000000, -60.00000000000000000 ) ) ;
#7367 = ADVANCED_FACE ( 'NONE', ( #44151 ), #35986, .F. ) ;
#7368 = EDGE_CURVE ( 'NONE', #43146, #9965, #32377, .T. ) ;
#7369 = CARTESIAN_POINT ( 'NONE',  ( 169.0000000000000000, -174.9999999999999716, -111.0000000000001563 ) ) ;
#7370 = ORIENTED_EDGE ( 'NONE', *, *, #41631, .F. ) ;
#7371 = CARTESIAN_POINT ( 'NONE',  ( 210.0000000000000568, 0.000000000000000000, 80.81828755692798438 ) ) ;
#7372 = ADVANCED_FACE ( 'NONE', ( #47975 ), #32123, .F. ) ;
#7373 = CARTESIAN_POINT ( 'NONE',  ( -2.569099690548740877, 33.19126772784019153, 3.199614146704519602 ) ) ;
#7374 = B_SPLINE_CURVE_WITH_KNOTS ( 'NONE', 3,
 ( #43757, #932, #16575, #47824 ),
 .UNSPECIFIED., .F., .F.,
 ( 4, 4 ),
 ( 4.123618687664377220E-17, 0.0004072981213155453940 ),
 .UNSPECIFIED. ) ;
#7375 = CIRCLE ( 'NONE', #12277, 20.99999999999999289 ) ;
#7376 = CARTESIAN_POINT ( 'NONE',  ( -0.8965959638259611841, -1.582931917743307215, 9.903764339332084887 ) ) ;
#7377 = EDGE_CURVE ( 'NONE', #49500, #8521, #47392, .T. ) ;
#7378 = VECTOR ( 'NONE', #38944, 1000.000000000000000 ) ;
#7379 = ORIENTED_EDGE ( 'NONE', *, *, #28643, .F. ) ;
#7380 = VECTOR ( 'NONE', #9335, 1000.000000000000000 ) ;
#7381 = DIRECTION ( 'NONE',  ( 0.000000000000000000, -1.000000000000000000, -0.000000000000000000 ) ) ;
#7382 =( BOUNDED_CURVE ( )  B_SPLINE_CURVE ( 3, ( #11813, #20510, #8471, #28223 ),
 .UNSPECIFIED., .F., .F. ) 
 B_SPLINE_CURVE_WITH_KNOTS ( ( 4, 4 ),
 ( 1.570796326794896558, 3.141592653589793116 ),
 .UNSPECIFIED. ) 
 CURVE ( )  GEOMETRIC_REPRESENTATION_ITEM ( )  RATIONAL_B_SPLINE_CURVE ( ( 1.000000000000000000, 0.8047378541243649375, 0.8047378541243649375, 1.000000000000000000 ) ) 
 REPRESENTATION_ITEM ( '' )  );
#7383 = ORIENTED_EDGE ( 'NONE', *, *, #7105, .F. ) ;
#7384 = DIRECTION ( 'NONE',  ( 6.203854594147707562E-25, -2.067951531382569187E-25, 1.000000000000000000 ) ) ;
#7385 = CARTESIAN_POINT ( 'NONE',  ( 2.945500763482280959, 16.64098165802040086, -9.008049429158102583 ) ) ;
#7386 = CARTESIAN_POINT ( 'NONE',  ( 75.05402655318509630, -1.025126265847089657, -80.93171244307201562 ) ) ;
#7387 = VECTOR ( 'NONE', #36516, 1000.000000000000000 ) ;
#7388 = CARTESIAN_POINT ( 'NONE',  ( -0.4426377647354682865, -1.666766018367764834, 9.928159647716134018 ) ) ;
#7389 = VECTOR ( 'NONE', #20025, 1000.000000000000000 ) ;
#7390 = VERTEX_POINT ( 'NONE', #28526 ) ;
#7391 = CARTESIAN_POINT ( 'NONE',  ( -1.011271242968688533, 0.7347315653655859258, 3.333333333333333481 ) ) ;
#7392 = EDGE_LOOP ( 'NONE', ( #23020, #17478, #31410, #21280 ) ) ;
#7393 = ORIENTED_EDGE ( 'NONE', *, *, #81, .T. ) ;
#7394 = ADVANCED_FACE ( 'NONE', ( #47224 ), #2012, .T. ) ;
#7395 = CARTESIAN_POINT ( 'NONE',  ( 0.9989200098981507736, 1.123829893718967687, 9.927319414211233095 ) ) ;
#7396 = AXIS2_PLACEMENT_3D ( 'NONE', #11302, #34406, #12068 ) ;
#7397 = EDGE_LOOP ( 'NONE', ( #11686, #37902, #32542, #23820 ) ) ;
#7398 = DIRECTION ( 'NONE',  ( -1.000000000000000000, -0.000000000000000000, -0.000000000000000000 ) ) ;
#7399 = CYLINDRICAL_SURFACE ( 'NONE', #40479, 1.750000000000015543 ) ;
#7400 = EDGE_CURVE ( 'NONE', #2423, #21356, #1532, .T. ) ;
#7401 = CARTESIAN_POINT ( 'NONE',  ( 28.96803024440893992, 18.11533787072037072, 7.455576670931136185 ) ) ;
#7402 = DIRECTION ( 'NONE',  ( -0.000000000000000000, -1.000000000000000000, -0.000000000000000000 ) ) ;
#7403 = EDGE_LOOP ( 'NONE', ( #36373, #31760, #22102, #48163 ) ) ;
#7404 = CARTESIAN_POINT ( 'NONE',  ( -166.6959734468149463, 0.000000000000000000, -165.0000000000000000 ) ) ;
#7405 = FACE_OUTER_BOUND ( 'NONE', #40165, .T. ) ;
#7406 = CARTESIAN_POINT ( 'NONE',  ( -208.4459734468148611, -1.025126265847089657, 79.06828755692797017 ) ) ;
#7407 = EDGE_CURVE ( 'NONE', #12974, #48624, #12867, .T. ) ;
#7408 = ORIENTED_EDGE ( 'NONE', *, *, #20678, .F. ) ;
#7409 = EDGE_CURVE ( 'NONE', #17284, #3318, #45078, .T. ) ;
#7410 = FACE_OUTER_BOUND ( 'NONE', #44592, .T. ) ;
#7411 = CARTESIAN_POINT ( 'NONE',  ( -3.525518877594380207, 1.771455644630627102, 6.494306115487987086 ) ) ;
#7412 = ORIENTED_EDGE ( 'NONE', *, *, #24326, .T. ) ;
#7413 = ORIENTED_EDGE ( 'NONE', *, *, #14574, .T. ) ;
#7414 = ORIENTED_EDGE ( 'NONE', *, *, #10312, .T. ) ;
#7415 = CARTESIAN_POINT ( 'NONE',  ( 210.0000000000000568, 0.000000000000000000, 160.8182875569279702 ) ) ;
#7416 = EDGE_CURVE ( 'NONE', #44023, #41284, #24823, .T. ) ;
#7417 = EDGE_CURVE ( 'NONE', #16010, #39173, #12121, .T. ) ;
#7418 = CARTESIAN_POINT ( 'NONE',  ( -50.00000000000000000, -50.00000000000000000, 900.0000000000000000 ) ) ;
#7419 = ORIENTED_EDGE ( 'NONE', *, *, #33361, .F. ) ;
#7420 = EDGE_CURVE ( 'NONE', #11639, #29172, #17616, .T. ) ;
#7421 = AXIS2_PLACEMENT_3D ( 'NONE', #39397, #12674, #28082 ) ;
#7422 = CARTESIAN_POINT ( 'NONE',  ( -1.158497635116737312, 16.61944452314319420, -3.546734833711462365 ) ) ;
#7423 = FACE_BOUND ( 'NONE', #2986, .T. ) ;
#7424 = AXIS2_PLACEMENT_3D ( 'NONE', #46404, #42826, #15902 ) ;
#7425 = CARTESIAN_POINT ( 'NONE',  ( -6.875132362119187768, 33.14667368551891258, 8.356839323120299312 ) ) ;
#7426 = FACE_OUTER_BOUND ( 'NONE', #17430, .T. ) ;
#7427 = CARTESIAN_POINT ( 'NONE',  ( 75.05402655318509630, 2.143131898507880377E-16, 122.5682875569279844 ) ) ;
#7428 = DIRECTION ( 'NONE',  ( -9.711650524620651178E-33, 1.223873602809432483E-48, -1.000000000000000000 ) ) ;
#7429 = AXIS2_PLACEMENT_3D ( 'NONE', #37968, #25905, #26394 ) ;
#7430 = CARTESIAN_POINT ( 'NONE',  ( 0.02998614097967981437, 1.600097392939184182, 9.919954280166516369 ) ) ;
#7431 = VECTOR ( 'NONE', #41548, 1000.000000000000000 ) ;
#7432 = LINE ( 'NONE', #8699, #31408 ) ;
#7433 = VECTOR ( 'NONE', #47147, 1000.000000000000000 ) ;
#7434 = ORIENTED_EDGE ( 'NONE', *, *, #7955, .T. ) ;
#7435 = LINE ( 'NONE', #11781, #10147 ) ;
#7436 = CARTESIAN_POINT ( 'NONE',  ( 10.00000000000000000, 249.9999999999999716, -224.9999999999999716 ) ) ;
#7437 = EDGE_CURVE ( 'NONE', #9086, #6173, #31882, .T. ) ;
#7438 = DIRECTION ( 'NONE',  ( 0.000000000000000000, 0.000000000000000000, 1.000000000000000000 ) ) ;
#7439 = CARTESIAN_POINT ( 'NONE',  ( -194.9999999999999432, -173.0000000000000000, 352.0000000000000568 ) ) ;
#7440 = ORIENTED_EDGE ( 'NONE', *, *, #47570, .T. ) ;
#7441 = CARTESIAN_POINT ( 'NONE',  ( -20.37409433808010562, -26.28007012093468475, -2.408242355805840784 ) ) ;
#7442 = CARTESIAN_POINT ( 'NONE',  ( -25.40454589245989325, -27.58367357691681931, -8.192531242611266862 ) ) ;
#7443 = DIRECTION ( 'NONE',  ( -1.000000000000000000, -0.000000000000000000, -0.000000000000000000 ) ) ;
#7444 = CYLINDRICAL_SURFACE ( 'NONE', #35689, 1.750000000000015543 ) ;
#7445 = LINE ( 'NONE', #22315, #13170 ) ;
#7446 =( BOUNDED_CURVE ( )  B_SPLINE_CURVE ( 3, ( #17950, #23072, #26681, #46128 ),
 .UNSPECIFIED., .F., .F. ) 
 B_SPLINE_CURVE_WITH_KNOTS ( ( 4, 4 ),
 ( 3.141592653589793116, 4.712388980384689674 ),
 .UNSPECIFIED. ) 
 CURVE ( )  GEOMETRIC_REPRESENTATION_ITEM ( )  RATIONAL_B_SPLINE_CURVE ( ( 1.000000000000000000, 0.8047378541243649375, 0.8047378541243649375, 1.000000000000000000 ) ) 
 REPRESENTATION_ITEM ( '' )  );
#7447 = VERTEX_POINT ( 'NONE', #50160 ) ;
#7448 = CARTESIAN_POINT ( 'NONE',  ( 35.05402655318504657, 2.143131898507880377E-16, 82.56828755692798438 ) ) ;
#7449 = EDGE_LOOP ( 'NONE', ( #34439, #14565, #48935, #2902, #28578, #41636 ) ) ;
#7450 = CARTESIAN_POINT ( 'NONE',  ( -0.1287570809895576818, -0.3962735484563154609, 10.00000000000000000 ) ) ;
#7451 = VERTEX_POINT ( 'NONE', #18905 ) ;
#7452 = CARTESIAN_POINT ( 'NONE',  ( -64.99999999999940314, 17.00000000000000000, -30.00000000000000000 ) ) ;
#7454 = EDGE_CURVE ( 'NONE', #40358, #34395, #42190, .T. ) ;
#7453 = DIRECTION ( 'NONE',  ( 0.000000000000000000, 0.000000000000000000, 1.000000000000000000 ) ) ;
#7455 =( BOUNDED_CURVE ( )  B_SPLINE_CURVE ( 3, ( #10515, #45888, #8951, #12291 ),
 .UNSPECIFIED., .F., .F. ) 
 B_SPLINE_CURVE_WITH_KNOTS ( ( 4, 4 ),
 ( 0.000000000000000000, 1.570796326794896558 ),
 .UNSPECIFIED. ) 
 CURVE ( )  GEOMETRIC_REPRESENTATION_ITEM ( )  RATIONAL_B_SPLINE_CURVE ( ( 1.000000000000000000, 0.8047378541243649375, 0.8047378541243649375, 1.000000000000000000 ) ) 
 REPRESENTATION_ITEM ( '' )  );
#7456 = VERTEX_POINT ( 'NONE', #2511 ) ;
#7457 = VERTEX_POINT ( 'NONE', #41758 ) ;
#7458 = AXIS2_PLACEMENT_3D ( 'NONE', #2391, #34215, #18035 ) ;
#7459 = ORIENTED_EDGE ( 'NONE', *, *, #16580, .T. ) ;
#7460 = CARTESIAN_POINT ( 'NONE',  ( -84.94597344681494633, 2.143131898507880377E-16, -37.43171244307205825 ) ) ;
#7461 = DIRECTION ( 'NONE',  ( 0.000000000000000000, 5.664403186863042467E-17, 1.000000000000000000 ) ) ;
#7462 = ORIENTED_EDGE ( 'NONE', *, *, #34779, .F. ) ;
#7463 = LINE ( 'NONE', #15407, #48287 ) ;
#7464 = LINE ( 'NONE', #38766, #35760 ) ;
#7465 = FACE_OUTER_BOUND ( 'NONE', #29065, .T. ) ;
#7466 = ORIENTED_EDGE ( 'NONE', *, *, #16868, .T. ) ;
#7467 = VECTOR ( 'NONE', #7831, 1000.000000000000000 ) ;
#7468 = VERTEX_POINT ( 'NONE', #26370 ) ;
#7469 = DIRECTION ( 'NONE',  ( 0.000000000000000000, 0.000000000000000000, 1.000000000000000000 ) ) ;
#7470 = DIRECTION ( 'NONE',  ( 1.132880637372608740E-16, 4.718402560806925739E-50, 1.000000000000000000 ) ) ;
#7471 = EDGE_CURVE ( 'NONE', #12617, #3137, #34517, .T. ) ;
#7472 = ORIENTED_EDGE ( 'NONE', *, *, #49872, .F. ) ;
#7473 = EDGE_CURVE ( 'NONE', #37912, #1398, #26873, .T. ) ;
#7474 = LINE ( 'NONE', #30063, #40687 ) ;
#7475 = DIRECTION ( 'NONE',  ( 0.000000000000000000, 0.000000000000000000, 1.000000000000000000 ) ) ;
#7476 = ORIENTED_EDGE ( 'NONE', *, *, #45645, .F. ) ;
#7477 = CARTESIAN_POINT ( 'NONE',  ( 35.00000000000216716, 17.00000000000000000, 95.00000000000000000 ) ) ;
#7478 = EDGE_CURVE ( 'NONE', #39523, #20701, #16513, .T. ) ;
#7479 = CARTESIAN_POINT ( 'NONE',  ( 15.00000000000000000, -46.12433806312137108, -6.404467680894764925 ) ) ;
#7480 = ORIENTED_EDGE ( 'NONE', *, *, #22248, .F. ) ;
#7481 = CARTESIAN_POINT ( 'NONE',  ( 181.0000000000000284, -174.9999999999999716, -99.00000000000014211 ) ) ;
#7482 = ADVANCED_FACE ( 'NONE', ( #25867 ), #10214, .F. ) ;
#7483 = CARTESIAN_POINT ( 'NONE',  ( 342.8284271247462129, -167.0000000000000000, 341.9999999999998295 ) ) ;
#7484 = CARTESIAN_POINT ( 'NONE',  ( 73.30402655318508209, 1.750000000000010214, 40.81828755692798438 ) ) ;
#7485 = EDGE_CURVE ( 'NONE', #27386, #38025, #49163, .T. ) ;
#7486 = CARTESIAN_POINT ( 'NONE',  ( -88.44597344681497475, 0.000000000000000000, 39.06828755692795596 ) ) ;
#7487 = ORIENTED_EDGE ( 'NONE', *, *, #42143, .F. ) ;
#7488 = DIRECTION ( 'NONE',  ( -0.000000000000000000, -0.000000000000000000, -1.000000000000000000 ) ) ;
#7489 = EDGE_CURVE ( 'NONE', #13763, #33331, #11602, .T. ) ;
#7490 = CARTESIAN_POINT ( 'NONE',  ( 17.51065725283126895, -28.41934970907778890, -9.367992836599954742 ) ) ;
#7491 = ORIENTED_EDGE ( 'NONE', *, *, #8703, .F. ) ;
#7493 = ORIENTED_EDGE ( 'NONE', *, *, #3463, .F. ) ;
#7492 = VECTOR ( 'NONE', #34474, 1000.000000000000000 ) ;
#7494 = CARTESIAN_POINT ( 'NONE',  ( 1067.899967415785568, 792.7343818613084068, 2031.331344752062705 ) ) ;
#7495 = CARTESIAN_POINT ( 'NONE',  ( -206.6959734468149463, 1.750000000000010658, -79.18171244307201562 ) ) ;
#7496 = DIRECTION ( 'NONE',  ( -1.000000000000000000, 0.000000000000000000, 0.000000000000000000 ) ) ;
#7497 = CARTESIAN_POINT ( 'NONE',  ( -556.8973046169135159, -62.56198943095993315, -64.63743994998280584 ) ) ;
#7498 = DIRECTION ( 'NONE',  ( -1.000000000000000000, 0.000000000000000000, 0.000000000000000000 ) ) ;
#7499 = EDGE_LOOP ( 'NONE', ( #16944, #2537, #49672, #22984 ) ) ;
#7500 = CARTESIAN_POINT ( 'NONE',  ( 153.3040265531850537, 1.750000000000010214, 40.81828755692798438 ) ) ;
#7502 = VECTOR ( 'NONE', #18151, 1000.000000000000000 ) ;
#7501 = DIRECTION ( 'NONE',  ( 0.000000000000000000, 1.000000000000000000, 0.000000000000000000 ) ) ;
#7503 = CARTESIAN_POINT ( 'NONE',  ( 34.08406891383362591, -15.63733501198463038, -8.192531242611266862 ) ) ;
#7504 = PLANE ( 'NONE',  #45239 ) ;
#7505 = VERTEX_POINT ( 'NONE', #34322 ) ;
#7506 = CARTESIAN_POINT ( 'NONE',  ( -1.275927284277175167, 0.1224368140627496299, 9.976582533991679824 ) ) ;
#7507 = CARTESIAN_POINT ( 'NONE',  ( 130.0000000000005684, 17.00000000000000000, -54.99999999999999289 ) ) ;
#7508 = ORIENTED_EDGE ( 'NONE', *, *, #35288, .T. ) ;
#7509 = CARTESIAN_POINT ( 'NONE',  ( -14.48769039275601145, -30.44468701195584970, 8.807470649214879543 ) ) ;
#7510 = DIRECTION ( 'NONE',  ( -1.000000000000000000, -0.000000000000000000, -0.000000000000000000 ) ) ;
#7511 = CARTESIAN_POINT ( 'NONE',  ( -14.99999999999845812, 17.00000000000000000, 60.00000000000000000 ) ) ;
#7512 = ORIENTED_EDGE ( 'NONE', *, *, #21317, .F. ) ;
#7513 = EDGE_CURVE ( 'NONE', #26878, #24770, #26461, .T. ) ;
#7514 = DIRECTION ( 'NONE',  ( 0.000000000000000000, -0.000000000000000000, -1.000000000000000000 ) ) ;
#7515 = CARTESIAN_POINT ( 'NONE',  ( 339.9999999999999432, 169.0000000000000000, -358.0000000000002274 ) ) ;
#7516 = VERTEX_POINT ( 'NONE', #30734 ) ;
#7517 = CARTESIAN_POINT ( 'NONE',  ( -7.721099712662037540, 1.750000000000023315, -0.2068387089191201234 ) ) ;
#7518 = CARTESIAN_POINT ( 'NONE',  ( 49.46074318306830975, -9.578883844006833570, 8.807470649214879543 ) ) ;
#7519 = UNCERTAINTY_MEASURE_WITH_UNIT (LENGTH_MEASURE( 1.000000000000000082E-05 ), #4712, 'distance_accuracy_value', 'NONE');
#7520 = PLANE ( 'NONE',  #34057 ) ;
#7521 = AXIS2_PLACEMENT_3D ( 'NONE', #25832, #18119, #49130 ) ;
#7522 = VECTOR ( 'NONE', #23770, 1000.000000000000000 ) ;
#7523 = ORIENTED_EDGE ( 'NONE', *, *, #794, .T. ) ;
#7524 = ORIENTED_EDGE ( 'NONE', *, *, #21872, .F. ) ;
#7525 = DIRECTION ( 'NONE',  ( -0.000000000000000000, -0.000000000000000000, 1.000000000000000000 ) ) ;
#7526 = CARTESIAN_POINT ( 'NONE',  ( 15.00000000000000000, -3.557843729863134463, -15.59977635401528850 ) ) ;
#7527 = ORIENTED_EDGE ( 'NONE', *, *, #40856, .T. ) ;
#7528 = ORIENTED_EDGE ( 'NONE', *, *, #971, .T. ) ;
#7529 = VECTOR ( 'NONE', #16963, 1000.000000000000000 ) ;
#7530 = CARTESIAN_POINT ( 'NONE',  ( 191.5540265531851105, 2.143131898507880377E-16, -160.9317124430720298 ) ) ;
#7531 = CYLINDRICAL_SURFACE ( 'NONE', #14443, 1.750000000000010214 ) ;
#7532 = DIRECTION ( 'NONE',  ( 0.000000000000000000, 0.000000000000000000, -1.000000000000000000 ) ) ;
#7533 = ORIENTED_EDGE ( 'NONE', *, *, #7701, .F. ) ;
#7534 = CARTESIAN_POINT ( 'NONE',  ( -21.61731705588949737, -25.43568671410585935, -9.367992836599954742 ) ) ;
#7535 = ORIENTED_EDGE ( 'NONE', *, *, #46197, .F. ) ;
#7536 = DIRECTION ( 'NONE',  ( -1.000000000000000000, -0.000000000000000000, -0.000000000000000000 ) ) ;
#7537 = AXIS2_PLACEMENT_3D ( 'NONE', #29972, #29712, #45327 ) ;
#7538 = EDGE_CURVE ( 'NONE', #45021, #39034, #38196, .T. ) ;
#7539 = DIRECTION ( 'NONE',  ( -1.000000000000000000, -0.000000000000000000, -0.000000000000000000 ) ) ;
#7540 = VERTEX_POINT ( 'NONE', #18652 ) ;
#7541 = ORIENTED_EDGE ( 'NONE', *, *, #41067, .T. ) ;
#7542 = ORIENTED_EDGE ( 'NONE', *, *, #44762, .F. ) ;
#7543 = CARTESIAN_POINT ( 'NONE',  ( 0.000000000000000000, -182.9999999999999716, -344.0000000000001705 ) ) ;
#7544 = EDGE_CURVE ( 'NONE', #36600, #15720, #3007, .T. ) ;
#7545 = CARTESIAN_POINT ( 'NONE',  ( 344.0000000000000568, 185.0000000000000284, 359.9999999999998295 ) ) ;
#7546 = CARTESIAN_POINT ( 'NONE',  ( -21.17460298198278323, -30.99364813079819214, -3.721387749823083624 ) ) ;
#7547 = VERTEX_POINT ( 'NONE', #49909 ) ;
#7548 = CARTESIAN_POINT ( 'NONE',  ( -87.72109971266203843, -1.750000000000009548, 39.79316129108089228 ) ) ;
#7549 = ORIENTED_EDGE ( 'NONE', *, *, #2180, .T. ) ;
#7550 = PLANE ( 'NONE',  #36510 ) ;
#7551 = ORIENTED_EDGE ( 'NONE', *, *, #47222, .F. ) ;
#7552 = DIRECTION ( 'NONE',  ( 0.000000000000000000, -8.021842663476564905E-17, -1.000000000000000000 ) ) ;
#7553 = CARTESIAN_POINT ( 'NONE',  ( 7.749480817862238524, 14.85497772329518895, 9.403735324607438884 ) ) ;
#7554 = PLANE ( 'NONE',  #21738 ) ;
#7555 = DIRECTION ( 'NONE',  ( -1.000000000000000000, -0.000000000000000000, -0.000000000000000000 ) ) ;
#7556 = ORIENTED_EDGE ( 'NONE', *, *, #13570, .F. ) ;
#7557 = VERTEX_POINT ( 'NONE', #33829 ) ;
#7558 = CARTESIAN_POINT ( 'NONE',  ( -0.9162543521530380763, 1.312131394983868660, 9.919954280166516369 ) ) ;
#7559 = VECTOR ( 'NONE', #32092, 1000.000000000000114 ) ;
#7560 = CARTESIAN_POINT ( 'NONE',  ( 181.0000000000000568, 165.0000000000000000, 343.9999999999998863 ) ) ;
#7561 = PLANE ( 'NONE',  #42488 ) ;
#7562 = CARTESIAN_POINT ( 'NONE',  ( -50.00000000000000000, -50.00000000000000000, 800.0000000000000000 ) ) ;
#7563 = B_SPLINE_CURVE_WITH_KNOTS ( 'NONE', 3,
 ( #25337, #6846, #29194, #48884 ),
 .UNSPECIFIED., .F., .F.,
 ( 4, 4 ),
 ( 0.0006669682284780769407, 0.0007799402130932229886 ),
 .UNSPECIFIED. ) ;
#7564 = VECTOR ( 'NONE', #4224, 1000.000000000000000 ) ;
#7565 = CARTESIAN_POINT ( 'NONE',  ( -2.892039187329358718, 1.502206308778131882, 9.799352050262546854 ) ) ;
#7566 = AXIS2_PLACEMENT_3D ( 'NONE', #5496, #24256, #12933 ) ;
#7567 = CARTESIAN_POINT ( 'NONE',  ( -115.0000000000000284, 17.00000000000000000, -90.00000000000000000 ) ) ;
#7568 = ORIENTED_EDGE ( 'NONE', *, *, #242, .F. ) ;
#7569 = CARTESIAN_POINT ( 'NONE',  ( -50.11058929355264979, 7.578863168071929834, 7.455576670931136185 ) ) ;
#7570 = CARTESIAN_POINT ( 'NONE',  ( 151.5540265531850537, 0.000000000000000000, 79.06828755692797017 ) ) ;
#7571 = EDGE_CURVE ( 'NONE', #49828, #5729, #11234, .T. ) ;
#7572 = VERTEX_POINT ( 'NONE', #23010 ) ;
#7573 = FACE_OUTER_BOUND ( 'NONE', #50256, .T. ) ;
#7574 = CARTESIAN_POINT ( 'NONE',  ( -168.4459734468149747, 1.025126265847089435, 39.06828755692797728 ) ) ;
#7575 = FACE_OUTER_BOUND ( 'NONE', #40709, .T. ) ;
#7576 = ORIENTED_EDGE ( 'NONE', *, *, #23378, .F. ) ;
#7577 = ORIENTED_EDGE ( 'NONE', *, *, #4272, .T. ) ;
#7578 = DIRECTION ( 'NONE',  ( -0.000000000000000000, -0.000000000000000000, -1.000000000000000000 ) ) ;
#7579 = CARTESIAN_POINT ( 'NONE',  ( 0.4166666666666664631, 0.000000000000000000, 10.00000000000000000 ) ) ;
#7580 =( BOUNDED_CURVE ( )  B_SPLINE_CURVE ( 3, ( #48295, #20380, #12429, #27845 ),
 .UNSPECIFIED., .F., .F. ) 
 B_SPLINE_CURVE_WITH_KNOTS ( ( 4, 4 ),
 ( 3.141592653589793116, 4.712388980384689674 ),
 .UNSPECIFIED. ) 
 CURVE ( )  GEOMETRIC_REPRESENTATION_ITEM ( )  RATIONAL_B_SPLINE_CURVE ( ( 1.000000000000000000, 0.8047378541243649375, 0.8047378541243649375, 1.000000000000000000 ) ) 
 REPRESENTATION_ITEM ( '' )  );
#7581 = EDGE_LOOP ( 'NONE', ( #21016, #22608, #26068, #5678 ) ) ;
#7582 = ORIENTED_EDGE ( 'NONE', *, *, #11419, .F. ) ;
#7583 = DIRECTION ( 'NONE',  ( -1.000000000000000000, -0.000000000000000000, -0.000000000000000000 ) ) ;
#7584 = CARTESIAN_POINT ( 'NONE',  ( 71.55402655318505367, 0.000000000000000000, 165.0000000000000000 ) ) ;
#7585 = VECTOR ( 'NONE', #17378, 1000.000000000000000 ) ;
#7586 = ORIENTED_EDGE ( 'NONE', *, *, #40930, .T. ) ;
#7587 = ORIENTED_EDGE ( 'NONE', *, *, #19618, .T. ) ;
#7588 = VECTOR ( 'NONE', #27240, 1000.000000000000000 ) ;
#7589 = EDGE_LOOP ( 'NONE', ( #35675, #43028, #12282, #4807, #19537, #17621 ) ) ;
#7590 = VECTOR ( 'NONE', #11288, 1000.000000000000000 ) ;
#7591 = CARTESIAN_POINT ( 'NONE',  ( 193.3040265531851105, -1.750000000000010214, -39.18171244307202983 ) ) ;
#7592 = PLANE ( 'NONE',  #39058 ) ;
#7593 = ORIENTED_EDGE ( 'NONE', *, *, #6541, .F. ) ;
#7594 = DIRECTION ( 'NONE',  ( -0.000000000000000000, -1.000000000000000000, -0.000000000000000000 ) ) ;
#7595 = VECTOR ( 'NONE', #39885, 1000.000000000000000 ) ;
#7596 = DIRECTION ( 'NONE',  ( 0.000000000000000000, -0.000000000000000000, -1.000000000000000000 ) ) ;
#7597 = CARTESIAN_POINT ( 'NONE',  ( 15.42815683172628738, 34.17926237904582365, 7.697694107796191787 ) ) ;
#7598 = EDGE_LOOP ( 'NONE', ( #41810, #32059, #27601, #5144 ) ) ;
#7599 = ORIENTED_EDGE ( 'NONE', *, *, #16419, .T. ) ;
#7600 = DIRECTION ( 'NONE',  ( -1.000000000000000000, 0.000000000000000000, 0.000000000000000000 ) ) ;
#7601 = EDGE_CURVE ( 'NONE', #17007, #3446, #30468, .T. ) ;
#7602 = SURFACE_SIDE_STYLE ('',( #30440 ) ) ;
#7603 =( BOUNDED_CURVE ( )  B_SPLINE_CURVE ( 3, ( #13939, #25253, #40906, #21394 ),
 .UNSPECIFIED., .F., .F. ) 
 B_SPLINE_CURVE_WITH_KNOTS ( ( 4, 4 ),
 ( 1.570796326794896558, 3.141592653589793116 ),
 .UNSPECIFIED. ) 
 CURVE ( )  GEOMETRIC_REPRESENTATION_ITEM ( )  RATIONAL_B_SPLINE_CURVE ( ( 1.000000000000000000, 0.8047378541243649375, 0.8047378541243649375, 1.000000000000000000 ) ) 
 REPRESENTATION_ITEM ( '' )  );
#7604 = CARTESIAN_POINT ( 'NONE',  ( 111.5540265531850679, 0.000000000000000000, -0.9317124430719969652 ) ) ;
#7605 = UNCERTAINTY_MEASURE_WITH_UNIT (LENGTH_MEASURE( 1.000000000000000082E-05 ), #22635, 'distance_accuracy_value', 'NONE');
#7606 = EDGE_LOOP ( 'NONE', ( #21266, #28265, #39229, #26984, #16343, #32088 ) ) ;
#7607 = ORIENTED_EDGE ( 'NONE', *, *, #2310, .F. ) ;
#7608 = LINE ( 'NONE', #35335, #49508 ) ;
#7609 = CARTESIAN_POINT ( 'NONE',  ( -125.6708471809678542, 1.749999999999996891, 79.79316129108087807 ) ) ;
#7610 = EDGE_LOOP ( 'NONE', ( #10377, #45891, #20577, #22178 ) ) ;
#7611 = CARTESIAN_POINT ( 'NONE',  ( 24.39427009665984869, 44.07992421011656603, 8.807470649214879543 ) ) ;
#7612 = DIRECTION ( 'NONE',  ( -0.000000000000000000, -0.000000000000000000, 1.000000000000000000 ) ) ;
#7613 = DIRECTION ( 'NONE',  ( 1.000000000000000000, 0.000000000000000000, 0.000000000000000000 ) ) ;
#7614 = DIRECTION ( 'NONE',  ( -0.000000000000000000, -1.000000000000000000, -0.000000000000000000 ) ) ;
#7615 = EDGE_LOOP ( 'NONE', ( #45956, #38588, #4468, #14310, #14728, #16993 ) ) ;
#7616 = EDGE_CURVE ( 'NONE', #38600, #25272, #38672, .T. ) ;
#7617 = LINE ( 'NONE', #30977, #31635 ) ;
#7618 = AXIS2_PLACEMENT_3D ( 'NONE', #12378, #348, #43665 ) ;
#7619 = CARTESIAN_POINT ( 'NONE',  ( 0.09523839817332763191, 1.466467394239034050, 9.958264684458713489 ) ) ;
#7620 = DIRECTION ( 'NONE',  ( 0.000000000000000000, 0.000000000000000000, 1.000000000000000000 ) ) ;
#7621 = EDGE_CURVE ( 'NONE', #20141, #17107, #42483, .T. ) ;
#7622 = CARTESIAN_POINT ( 'NONE',  ( 15.62858259096121216, -5.755205073598614440, -9.683996418299976483 ) ) ;
#7623 =( REPRESENTATION_RELATIONSHIP ('NONE','NONE', #45699, #3157 ) REPRESENTATION_RELATIONSHIP_WITH_TRANSFORMATION ( #13092 )SHAPE_REPRESENTATION_RELATIONSHIP( ) );
#7624 = EDGE_LOOP ( 'NONE', ( #37751, #10665, #43068, #18772 ) ) ;
#7625 = CARTESIAN_POINT ( 'NONE',  ( 6.906133693021909714, 3.984196388068609096, -1.219727444046192488E-16 ) ) ;
#7626 = CARTESIAN_POINT ( 'NONE',  ( 130.0000000000015064, 17.00000000000000000, 35.00000000000000000 ) ) ;
#7627 = EDGE_CURVE ( 'NONE', #20559, #38882, #36990, .T. ) ;
#7628 = EDGE_CURVE ( 'NONE', #39919, #18651, #45177, .T. ) ;
#7629 = FACE_OUTER_BOUND ( 'NONE', #7392, .T. ) ;
#7630 = MECHANICAL_DESIGN_GEOMETRIC_PRESENTATION_REPRESENTATION (  '', ( #14986 ), #49363 ) ;
#7632 = ORIENTED_EDGE ( 'NONE', *, *, #45653, .T. ) ;
#7631 = EDGE_CURVE ( 'NONE', #22898, #7540, #16090, .T. ) ;
#7633 = CARTESIAN_POINT ( 'NONE',  ( -5.670847180967843570, -1.750000000000022427, 159.7931612910808781 ) ) ;
#7634 = AXIS2_PLACEMENT_3D ( 'NONE', #36741, #48208, #6919 ) ;
#7635 = CARTESIAN_POINT ( 'NONE',  ( 33.30402655318503946, 0.000000000000000000, -165.0000000000000000 ) ) ;
#7636 = ORIENTED_EDGE ( 'NONE', *, *, #14680, .T. ) ;
#7637 = LINE ( 'NONE', #11731, #37690 ) ;
#7638 = CARTESIAN_POINT ( 'NONE',  ( 72.27890028733797578, 1.750000000000009548, 39.79316129108089228 ) ) ;
#7639 = FACE_OUTER_BOUND ( 'NONE', #15679, .T. ) ;
#7640 = FACE_OUTER_BOUND ( 'NONE', #24597, .T. ) ;
#7641 = ORIENTED_EDGE ( 'NONE', *, *, #14848, .T. ) ;
#7642 = B_SPLINE_SURFACE_WITH_KNOTS ( 'NONE', 3, 3, ( 
 ( #28161, #24320, #41464, #33520 ),
 ( #17853, #49853, #14512, #29659 ),
 ( #10660, #2461, #30164, #2217 ),
 ( #2954, #14254, #21447, #21963 ) ),
 .UNSPECIFIED., .F., .F., .F.,
 ( 4, 4 ),
 ( 4, 4 ),
 ( 0.000000000000000000, 1.000000000000000000 ),
 ( 0.000000000000000000, 1.000000000000000000 ),
 .UNSPECIFIED. ) ;
#7643 = ORIENTED_EDGE ( 'NONE', *, *, #29939, .T. ) ;
#7644 = VERTEX_POINT ( 'NONE', #19682 ) ;
#7645 = PLANE ( 'NONE',  #19714 ) ;
#7646 = ORIENTED_EDGE ( 'NONE', *, *, #11085, .T. ) ;
#7647 = DIRECTION ( 'NONE',  ( 0.000000000000000000, 0.2223603367690619725, -0.9749645535258958384 ) ) ;
#7648 = DIRECTION ( 'NONE',  ( 0.000000000000000000, -1.000000000000000000, -3.186989995019654210E-49 ) ) ;
#7649 = CARTESIAN_POINT ( 'NONE',  ( 0.3905129037392675584, -2.126717070043174562, 9.885585981620943485 ) ) ;
#7650 = EDGE_CURVE ( 'NONE', #23917, #42991, #23791, .T. ) ;
#7651 = ORIENTED_EDGE ( 'NONE', *, *, #33145, .T. ) ;
#7652 = LINE ( 'NONE', #38963, #10256 ) ;
#7653 = CARTESIAN_POINT ( 'NONE',  ( 115.0540265531850395, -1.025126265847081886, -120.9317124430720440 ) ) ;
#7654 = DIRECTION ( 'NONE',  ( 0.000000000000000000, 1.000000000000000000, 0.000000000000000000 ) ) ;
#7655 = ADVANCED_FACE ( 'NONE', ( #39955 ), #12233, .F. ) ;
#7656 = ORIENTED_EDGE ( 'NONE', *, *, #1804, .F. ) ;
#7657 = ADVANCED_FACE ( 'NONE', ( #20186 ), #198, .F. ) ;
#7658 = DIRECTION ( 'NONE',  ( 0.000000000000000000, 0.000000000000000000, 1.000000000000000000 ) ) ;
#7659 = AXIS2_PLACEMENT_3D ( 'NONE', #9704, #9959, #8957 ) ;
#7660 = ORIENTED_EDGE ( 'NONE', *, *, #22451, .T. ) ;
#7661 = VERTEX_POINT ( 'NONE', #3779 ) ;
#7662 = ORIENTED_EDGE ( 'NONE', *, *, #35284, .F. ) ;
#7663 = CARTESIAN_POINT ( 'NONE',  ( 85.00000000000056843, 17.00000000000000000, -54.99999999999999289 ) ) ;
#7664 = EDGE_CURVE ( 'NONE', #34755, #31952, #12256, .T. ) ;
#7665 = CIRCLE ( 'NONE', #14194, 2.000000000000001776 ) ;
#7666 = DIRECTION ( 'NONE',  ( 0.000000000000000000, 1.000000000000000000, 0.000000000000000000 ) ) ;
#7667 = ORIENTED_EDGE ( 'NONE', *, *, #25355, .T. ) ;
#7668 = ADVANCED_FACE ( 'NONE', ( #47341 ), #27898, .F. ) ;
#7669 = CARTESIAN_POINT ( 'NONE',  ( -1.249999999999999778, 0.000000000000000000, 3.333333333333333481 ) ) ;
#7670 = DIRECTION ( 'NONE',  ( 0.000000000000000000, 0.000000000000000000, 1.000000000000000000 ) ) ;
#7671 = CARTESIAN_POINT ( 'NONE',  ( -114.9999999999978542, 17.00000000000000000, 115.0000000000000142 ) ) ;
#7672 = DIRECTION ( 'NONE',  ( -3.172065784643302499E-16, -1.000000000000000000, 2.537652627714642000E-15 ) ) ;
#7673 = CARTESIAN_POINT ( 'NONE',  ( 1.133908876584335257, 0.5183204401656757998, 9.981352469109932457 ) ) ;
#7674 = AXIS2_PLACEMENT_3D ( 'NONE', #1636, #18021, #33694 ) ;
#7675 = LINE ( 'NONE', #26909, #44648 ) ;
#7676 = DIRECTION ( 'NONE',  ( 1.000000000000000000, 0.000000000000000000, -1.734723475976805517E-15 ) ) ;
#7677 = CARTESIAN_POINT ( 'NONE',  ( 370.7621192902014968, -61.66198943095990614, -93.79675437945473959 ) ) ;
#7678 = CARTESIAN_POINT ( 'NONE',  ( 0.1475726264153646716, 1.496347932843221429, 9.927319414211224213 ) ) ;
#7679 = FACE_OUTER_BOUND ( 'NONE', #23290, .T. ) ;
#7680 = ORIENTED_EDGE ( 'NONE', *, *, #1448, .F. ) ;
#7681 = DIRECTION ( 'NONE',  ( 0.000000000000000000, 1.000000000000000000, 0.000000000000000000 ) ) ;
#7682 = CARTESIAN_POINT ( 'NONE',  ( -125.6708471809678542, 1.749999999999996669, 41.84341382277508359 ) ) ;
#7683 = VECTOR ( 'NONE', #30128, 1000.000000000000000 ) ;
#7684 =( BOUNDED_CURVE ( )  B_SPLINE_CURVE ( 3, ( #32319, #12805, #16919, #32576 ),
 .UNSPECIFIED., .F., .F. ) 
 B_SPLINE_CURVE_WITH_KNOTS ( ( 4, 4 ),
 ( 4.712388980384689674, 6.283185307179586232 ),
 .UNSPECIFIED. ) 
 CURVE ( )  GEOMETRIC_REPRESENTATION_ITEM ( )  RATIONAL_B_SPLINE_CURVE ( ( 1.000000000000000000, 0.8047378541243649375, 0.8047378541243649375, 1.000000000000000000 ) ) 
 REPRESENTATION_ITEM ( '' )  );
#7685 = LINE ( 'NONE', #49716, #17509 ) ;
#7686 = DIRECTION ( 'NONE',  ( -1.000000000000000000, 0.000000000000000000, 0.000000000000000000 ) ) ;
#7687 = EDGE_LOOP ( 'NONE', ( #26628, #14716, #26841, #21055 ) ) ;
#7688 = DIRECTION ( 'NONE',  ( -1.000000000000000000, 0.000000000000000000, 0.000000000000000000 ) ) ;
#7689 = CARTESIAN_POINT ( 'NONE',  ( -119.9999999999990905, 16.00000000000000000, 0.000000000000000000 ) ) ;
#7690 = LINE ( 'NONE', #26926, #16837 ) ;
#7691 = EDGE_CURVE ( 'NONE', #28486, #33010, #18205, .T. ) ;
#7692 = ADVANCED_FACE ( 'NONE', ( #11478 ), #39199, .F. ) ;
#7693 = CARTESIAN_POINT ( 'NONE',  ( 16.02661358026014327, 4.530191650547718218, -9.683996418299976483 ) ) ;
#7695 = ORIENTED_EDGE ( 'NONE', *, *, #27088, .F. ) ;
#7694 = EDGE_CURVE ( 'NONE', #10222, #18457, #46837, .T. ) ;
#7696 = SURFACE_STYLE_FILL_AREA ( #26685 ) ;
#7697 = EDGE_CURVE ( 'NONE', #44581, #45897, #24309, .T. ) ;
#7698 = ORIENTED_EDGE ( 'NONE', *, *, #34656, .T. ) ;
#7699 = CARTESIAN_POINT ( 'NONE',  ( 0.1475726264153646716, 1.496347932843221429, 9.927319414211224213 ) ) ;
#7700 = ORIENTED_EDGE ( 'NONE', *, *, #32054, .T. ) ;
#7701 = EDGE_CURVE ( 'NONE', #4897, #43762, #5784, .T. ) ;
#7702 = DIRECTION ( 'NONE',  ( 1.000000000000000000, 0.000000000000000000, 0.000000000000000000 ) ) ;
#7703 = AXIS2_PLACEMENT_3D ( 'NONE', #8195, #4085, #8448 ) ;
#7704 = CARTESIAN_POINT ( 'NONE',  ( 195.0540265531851105, 1.025126265847089879, 122.5682875569280128 ) ) ;
#7705 = EDGE_CURVE ( 'NONE', #19380, #13001, #12478, .T. ) ;
#7706 = ORIENTED_EDGE ( 'NONE', *, *, #16792, .F. ) ;
#7707 = DIRECTION ( 'NONE',  ( -0.000000000000000000, -1.000000000000000000, 2.537652627714643577E-15 ) ) ;
#7708 = VERTEX_POINT ( 'NONE', #46582 ) ;
#7709 = VECTOR ( 'NONE', #6403, 1000.000000000000000 ) ;
#7710 = B_SPLINE_CURVE_WITH_KNOTS ( 'NONE', 3,
 ( #46090, #7649, #42286, #23281 ),
 .UNSPECIFIED., .F., .F.,
 ( 4, 4 ),
 ( 0.9688112071879401155, 0.9724175925769218409 ),
 .UNSPECIFIED. ) ;
#7711 = ORIENTED_EDGE ( 'NONE', *, *, #46471, .T. ) ;
#7712 = DIRECTION ( 'NONE',  ( 1.000000000000000000, 0.000000000000000000, -0.000000000000000000 ) ) ;
#7713 = LINE ( 'NONE', #12552, #20792 ) ;
#7714 = ORIENTED_EDGE ( 'NONE', *, *, #13596, .T. ) ;
#7715 = LINE ( 'NONE', #49992, #4095 ) ;
#7716 = DIRECTION ( 'NONE',  ( -7.793956916774524585E-48, 0.000000000000000000, -1.000000000000000000 ) ) ;
#7717 = DIRECTION ( 'NONE',  ( 0.000000000000000000, 0.000000000000000000, -1.000000000000000000 ) ) ;
#7718 = B_SPLINE_CURVE_WITH_KNOTS ( 'NONE', 3,
 ( #36876, #949, #1696, #20685 ),
 .UNSPECIFIED., .F., .F.,
 ( 4, 4 ),
 ( 0.000000000000000000, 0.2637263876330694368 ),
 .UNSPECIFIED. ) ;
#7719 = ORIENTED_EDGE ( 'NONE', *, *, #46232, .T. ) ;
#7720 = LINE ( 'NONE', #23098, #29202 ) ;
#7721 = FACE_BOUND ( 'NONE', #19713, .T. ) ;
#7722 = EDGE_CURVE ( 'NONE', #47029, #47424, #7637, .T. ) ;
#7723 = ORIENTED_EDGE ( 'NONE', *, *, #45517, .T. ) ;
#7724 = ADVANCED_FACE ( 'NONE', ( #5542 ), #32518, .T. ) ;
#7725 = CARTESIAN_POINT ( 'NONE',  ( 210.0000000000000568, 0.000000000000000000, -159.1817124430720298 ) ) ;
#7726 = CARTESIAN_POINT ( 'NONE',  ( 181.0000000000000000, 6.000000000000060396, 339.9999999999998295 ) ) ;
#7727 = ORIENTED_EDGE ( 'NONE', *, *, #31034, .F. ) ;
#7728 = CARTESIAN_POINT ( 'NONE',  ( -206.6959734468149463, 0.000000000000000000, -165.0000000000000000 ) ) ;
#7729 = DIRECTION ( 'NONE',  ( -1.000000000000000000, 0.000000000000000000, 0.000000000000000000 ) ) ;
#7730 = PRODUCT_RELATED_PRODUCT_CATEGORY ( 'part', '', ( #43383 ) ) ;
#7731 = ORIENTED_EDGE ( 'NONE', *, *, #23304, .T. ) ;
#7732 = CARTESIAN_POINT ( 'NONE',  ( 24.34206871062956168, 28.53454467304761621, -9.011255500499641968 ) ) ;
#7733 = DIRECTION ( 'NONE',  ( -0.000000000000000000, 0.000000000000000000, -1.000000000000000000 ) ) ;
#7734 = CARTESIAN_POINT ( 'NONE',  ( 355.9999999999999432, 174.9999999999996589, -358.0000000000003411 ) ) ;
#7735 = ORIENTED_EDGE ( 'NONE', *, *, #19924, .T. ) ;
#7736 = AXIS2_PLACEMENT_3D ( 'NONE', #34861, #31008, #11494 ) ;
#7737 = CARTESIAN_POINT ( 'NONE',  ( 85.00000000000152056, 17.00000000000000000, 35.00000000000000000 ) ) ;
#7738 = LINE ( 'NONE', #26221, #36586 ) ;
#7739 = VECTOR ( 'NONE', #22143, 1000.000000000000000 ) ;
#7740 = EDGE_CURVE ( 'NONE', #13837, #42454, #28716, .T. ) ;
#7741 = CARTESIAN_POINT ( 'NONE',  ( -33.57695195286787282, -16.69845195084869616, 8.914903342594564961 ) ) ;
#7742 = ORIENTED_EDGE ( 'NONE', *, *, #30355, .F. ) ;
#7743 = ORIENTED_EDGE ( 'NONE', *, *, #11410, .T. ) ;
#7744 = CARTESIAN_POINT ( 'NONE',  ( 32.27890028733795447, 1.750000000000010436, -120.2068387089191219 ) ) ;
#7745 =( BOUNDED_CURVE ( )  B_SPLINE_CURVE ( 3, ( #42640, #11098, #3649, #23142 ),
 .UNSPECIFIED., .F., .F. ) 
 B_SPLINE_CURVE_WITH_KNOTS ( ( 4, 4 ),
 ( 0.000000000000000000, 1.570796326794896780 ),
 .UNSPECIFIED. ) 
 CURVE ( )  GEOMETRIC_REPRESENTATION_ITEM ( )  RATIONAL_B_SPLINE_CURVE ( ( 1.000000000000000000, 0.8047378541243649375, 0.8047378541243649375, 1.000000000000000000 ) ) 
 REPRESENTATION_ITEM ( '' )  );
#7746 = DIRECTION ( 'NONE',  ( 1.542934785277601468E-15, 0.9749645535258959494, -0.2223603367690620558 ) ) ;
#7747 = FILL_AREA_STYLE ('',( #46946 ) ) ;
#7748 = DIRECTION ( 'NONE',  ( 1.000000000000000000, 0.000000000000000000, 0.000000000000000000 ) ) ;
#7749 = EDGE_CURVE ( 'NONE', #12984, #23377, #44024, .T. ) ;
#7750 = DIRECTION ( 'NONE',  ( 1.000000000000000000, 0.000000000000000000, 0.000000000000000000 ) ) ;
#7751 = ORIENTED_EDGE ( 'NONE', *, *, #16405, .T. ) ;
#7752 = CARTESIAN_POINT ( 'NONE',  ( -47.72109971266203132, 1.750000000000009548, -78.15658617722490931 ) ) ;
#7753 =( BOUNDED_CURVE ( )  B_SPLINE_CURVE ( 3, ( #19538, #35223, #577, #16216 ),
 .UNSPECIFIED., .F., .F. ) 
 B_SPLINE_CURVE_WITH_KNOTS ( ( 4, 4 ),
 ( 1.570796326794896558, 3.141592653589793116 ),
 .UNSPECIFIED. ) 
 CURVE ( )  GEOMETRIC_REPRESENTATION_ITEM ( )  RATIONAL_B_SPLINE_CURVE ( ( 1.000000000000000000, 0.8047378541243649375, 0.8047378541243649375, 1.000000000000000000 ) ) 
 REPRESENTATION_ITEM ( '' )  );
#7754 = PRODUCT_DEFINITION_SHAPE ( 'NONE', 'NONE',  #50739 ) ;
#7755 = LINE ( 'NONE', #31362, #3179 ) ;
#7756 = CARTESIAN_POINT ( 'NONE',  ( 113.3040265531850537, 1.749999999999997113, -39.18171244307202983 ) ) ;
#7757 =( LENGTH_UNIT ( ) NAMED_UNIT ( * ) SI_UNIT ( .MILLI., .METRE. ) );
#7759 = ORIENTED_EDGE ( 'NONE', *, *, #34938, .F. ) ;
#7758 = EDGE_CURVE ( 'NONE', #17745, #18968, #36350, .T. ) ;
#7760 = AXIS2_PLACEMENT_3D ( 'NONE', #19523, #42871, #3368 ) ;
#7761 = DIRECTION ( 'NONE',  ( 0.000000000000000000, -0.9230769230769231282, 0.3846153846153845812 ) ) ;
#7762 = ADVANCED_FACE ( 'NONE', ( #36366 ), #29396, .T. ) ;
#7763 = VERTEX_POINT ( 'NONE', #13234 ) ;
#7764 = CARTESIAN_POINT ( 'NONE',  ( 73.30402655318508209, -1.750000000000009992, 160.8182875569279702 ) ) ;
#7765 = TOROIDAL_SURFACE ( 'NONE', #29871, 27.58190990837850265, 8.000000000000000000 ) ;
#7766 = CARTESIAN_POINT ( 'NONE',  ( 6.508636631827673824, 15.75743548351451295, 8.953103998512858652 ) ) ;
#7767 = ORIENTED_EDGE ( 'NONE', *, *, #47179, .T. ) ;
#7768 = B_SPLINE_CURVE_WITH_KNOTS ( 'NONE', 3,
 ( #9424, #36138, #28672, #25331 ),
 .UNSPECIFIED., .F., .F.,
 ( 4, 4 ),
 ( 0.000000000000000000, 2.804146970187276501E-05 ),
 .UNSPECIFIED. ) ;
#7769 = DIRECTION ( 'NONE',  ( -1.612977847700450206E-50, 0.000000000000000000, 1.000000000000000000 ) ) ;
#7770 = CARTESIAN_POINT ( 'NONE',  ( -1.011271242968693862, 0.7347315653655780432, 10.00000000000000000 ) ) ;
#7771 = EDGE_CURVE ( 'NONE', #49813, #39284, #40455, .T. ) ;
#7772 = CARTESIAN_POINT ( 'NONE',  ( 10.92344319659198248, 12.63397777816698486, -9.458680755252684591 ) ) ;
#7773 = EDGE_LOOP ( 'NONE', ( #14732, #41715, #1785, #27743 ) ) ;
#7774 = ADVANCED_FACE ( 'NONE', ( #45017 ), #1704, .T. ) ;
#7775 = EDGE_CURVE ( 'NONE', #449, #16032, #13049, .T. ) ;
#7776 = CARTESIAN_POINT ( 'NONE',  ( -208.4459734468149463, 0.000000000000000000, 39.06828755692798438 ) ) ;
#7777 = CARTESIAN_POINT ( 'NONE',  ( 340.0000000000000568, 165.0000000000000000, 355.9999999999997726 ) ) ;
#7778 = VERTEX_POINT ( 'NONE', #9897 ) ;
#7779 = CARTESIAN_POINT ( 'NONE',  ( 2.499999999999945377, -224.9999999999999716, -240.0000000000000000 ) ) ;
#7780 = CIRCLE ( 'NONE', #36463, 0.5000000000000000000 ) ;
#7781 = CARTESIAN_POINT ( 'NONE',  ( 236.0000000000000000, -169.9999999999999716, 474.9999999999998863 ) ) ;
#7782 = CYLINDRICAL_SURFACE ( 'NONE', #2471, 1.750000000000008438 ) ;
#7783 = DIRECTION ( 'NONE',  ( 0.000000000000000000, 0.000000000000000000, -1.000000000000000000 ) ) ;
#7784 = ADVANCED_FACE ( 'NONE', ( #17597 ), #17344, .T. ) ;
#7785 = ORIENTED_EDGE ( 'NONE', *, *, #16846, .T. ) ;
#7786 = ORIENTED_EDGE ( 'NONE', *, *, #1831, .F. ) ;
#7787 = CARTESIAN_POINT ( 'NONE',  ( -114.9999999999994031, 16.00000000000000000, -54.99999999999999289 ) ) ;
#7788 = VECTOR ( 'NONE', #17316, 1000.000000000000000 ) ;
#7789 = EDGE_LOOP ( 'NONE', ( #28828, #46978, #40860, #45894, #4480, #44245 ) ) ;
#7790 = CARTESIAN_POINT ( 'NONE',  ( 34.99999999999997868, 16.00000000000000000, -90.00000000000000000 ) ) ;
#7791 = CARTESIAN_POINT ( 'NONE',  ( 339.9999999999998863, -168.9999999999999432, 355.9999999999997726 ) ) ;
#7792 = DIRECTION ( 'NONE',  ( -0.5038710255240859137, 0.000000000000000000, 0.8637789008984335659 ) ) ;
#7793 = ORIENTED_EDGE ( 'NONE', *, *, #10803, .F. ) ;
#7794 = CARTESIAN_POINT ( 'NONE',  ( -7.359817328027146388, -15.16751262232800102, 2.590526750877053086 ) ) ;
#7795 = EDGE_LOOP ( 'NONE', ( #1160, #48452, #44718, #2006, #6896 ) ) ;
#7796 = CARTESIAN_POINT ( 'NONE',  ( -1.104609456715841986, -0.6504863887005195577, 9.948547179989617462 ) ) ;
#7797 = PLANE ( 'NONE',  #11121 ) ;
#7798 = DIRECTION ( 'NONE',  ( 6.765175596986472868E-16, -0.9749645535258953943, -0.2223603367690637489 ) ) ;
#7799 = VECTOR ( 'NONE', #49846, 1000.000000000000000 ) ;
#7800 = ORIENTED_EDGE ( 'NONE', *, *, #10307, .T. ) ;
#7801 = ORIENTED_EDGE ( 'NONE', *, *, #18621, .T. ) ;
#7802 = ORIENTED_EDGE ( 'NONE', *, *, #1385, .T. ) ;
#7803 = VECTOR ( 'NONE', #43151, 1000.000000000000000 ) ;
#7804 = CARTESIAN_POINT ( 'NONE',  ( 167.4999999999999716, 74.83106485270648989, -120.5992382549688955 ) ) ;
#7805 = CARTESIAN_POINT ( 'NONE',  ( 193.3040265531851105, -1.750000000000009992, 160.8182875569279702 ) ) ;
#7806 = LINE ( 'NONE', #43436, #23351 ) ;
#7807 = VERTEX_POINT ( 'NONE', #5030 ) ;
#7808 = CYLINDRICAL_SURFACE ( 'NONE', #31373, 2.000000000000001776 ) ;
#7809 = ORIENTED_EDGE ( 'NONE', *, *, #25233, .T. ) ;
#7810 = EDGE_CURVE ( 'NONE', #48234, #4486, #7137, .T. ) ;
#7811 = DIRECTION ( 'NONE',  ( 0.000000000000000000, -0.000000000000000000, -1.000000000000000000 ) ) ;
#7812 = VERTEX_POINT ( 'NONE', #21438 ) ;
#7813 = DIRECTION ( 'NONE',  ( 0.000000000000000000, 0.000000000000000000, 1.000000000000000000 ) ) ;
#7814 = FACE_OUTER_BOUND ( 'NONE', #22893, .T. ) ;
#7815 = DIRECTION ( 'NONE',  ( -0.7233555441435721711, -0.6904757466825005574, 0.000000000000000000 ) ) ;
#7816 = PLANE ( 'NONE',  #13565 ) ;
#7817 = CARTESIAN_POINT ( 'NONE',  ( 164.9999999999999716, -168.9999999999999432, -350.0000000000001705 ) ) ;
#7818 = VERTEX_POINT ( 'NONE', #36633 ) ;
#7819 = ORIENTED_EDGE ( 'NONE', *, *, #6376, .F. ) ;
#7820 = CARTESIAN_POINT ( 'NONE',  ( -14.49999999999999822, -46.51315789473684248, -5.916985404131818171 ) ) ;
#7821 = DIRECTION ( 'NONE',  ( -0.000000000000000000, -0.000000000000000000, -1.000000000000000000 ) ) ;
#7822 = LINE ( 'NONE', #31426, #36778 ) ;
#7823 = DIRECTION ( 'NONE',  ( -1.000000000000000000, -0.000000000000000000, -0.000000000000000000 ) ) ;
#7824 = VECTOR ( 'NONE', #40859, 1000.000000000000000 ) ;
#7825 = ADVANCED_FACE ( 'NONE', ( #20948 ), #25057, .T. ) ;
#7826 = CARTESIAN_POINT ( 'NONE',  ( -0.1287570809895602630, -0.3962735484563142396, 10.00000000000000000 ) ) ;
#7827 = ADVANCED_FACE ( 'NONE', ( #20427 ), #13741, .T. ) ;
#7828 = LINE ( 'NONE', #35042, #44206 ) ;
#7829 = ORIENTED_EDGE ( 'NONE', *, *, #36041, .T. ) ;
#7830 = FACE_OUTER_BOUND ( 'NONE', #44358, .T. ) ;
#7831 = DIRECTION ( 'NONE',  ( 6.203854594147707562E-25, -2.067951531382569187E-25, 1.000000000000000000 ) ) ;
#7832 = EDGE_CURVE ( 'NONE', #25636, #33167, #6500, .T. ) ;
#7833 = ADVANCED_FACE ( 'NONE', ( #25298 ), #41603, .T. ) ;
#7834 = ORIENTED_EDGE ( 'NONE', *, *, #44301, .T. ) ;
#7835 = CIRCLE ( 'NONE', #44671, 10.00000000000000000 ) ;
#7836 = CARTESIAN_POINT ( 'NONE',  ( 115.0540265531850395, -1.025126265847081442, -160.9317124430720014 ) ) ;
#7837 = VECTOR ( 'NONE', #38188, 1000.000000000000000 ) ;
#7838 = CARTESIAN_POINT ( 'NONE',  ( -31.44259251615275019, -38.95901822126145220, -9.367992836599954742 ) ) ;
#7839 = EDGE_CURVE ( 'NONE', #39727, #19789, #22454, .T. ) ;
#7840 = LINE ( 'NONE', #26819, #7799 ) ;
#7841 = AXIS2_PLACEMENT_3D ( 'NONE', #31092, #11332, #39302 ) ;
#7842 = ORIENTED_EDGE ( 'NONE', *, *, #44186, .T. ) ;
#7843 = VERTEX_POINT ( 'NONE', #38128 ) ;
#7844 = CARTESIAN_POINT ( 'NONE',  ( 193.3040265531851105, 0.000000000000000000, 165.0000000000000000 ) ) ;
#7845 = CARTESIAN_POINT ( 'NONE',  ( 181.0000000000000284, -9.999999999999953815, -95.00000000000014211 ) ) ;
#7846 =( GEOMETRIC_REPRESENTATION_CONTEXT ( 3 ) GLOBAL_UNCERTAINTY_ASSIGNED_CONTEXT ( ( #27104 ) ) GLOBAL_UNIT_ASSIGNED_CONTEXT ( ( #23127, #47956, #47455 ) ) REPRESENTATION_CONTEXT ( 'NONE', 'WORKASPACE' ) );
#7847 = ORIENTED_EDGE ( 'NONE', *, *, #30192, .F. ) ;
#7848 = ORIENTED_EDGE ( 'NONE', *, *, #15588, .T. ) ;
#7849 = CARTESIAN_POINT ( 'NONE',  ( -45.67084718096785423, 1.750000000000009548, -38.15658617722494483 ) ) ;
#7850 = CARTESIAN_POINT ( 'NONE',  ( -6.174150299305392053, 33.14591993373988998, 8.807470649214879543 ) ) ;
#7851 = DIRECTION ( 'NONE',  ( -1.000000000000000000, -0.000000000000000000, -0.000000000000000000 ) ) ;
#7852 = AXIS2_PLACEMENT_3D ( 'NONE', #1930, #32044, #36854 ) ;
#7853 = DIRECTION ( 'NONE',  ( 0.000000000000000000, -0.000000000000000000, -1.000000000000000000 ) ) ;
#7854 = AXIS2_PLACEMENT_3D ( 'NONE', #39988, #29189, #21224 ) ;
#7855 = VERTEX_POINT ( 'NONE', #15014 ) ;
#7856 = EDGE_LOOP ( 'NONE', ( #44937, #7082, #31814, #26393, #39662, #17897 ) ) ;
#7857 = ORIENTED_EDGE ( 'NONE', *, *, #39672, .T. ) ;
#7858 = AXIS2_PLACEMENT_3D ( 'NONE', #38106, #21939, #37606 ) ;
#7859 = FACE_OUTER_BOUND ( 'NONE', #8897, .T. ) ;
#7860 = CARTESIAN_POINT ( 'NONE',  ( -164.9999999999987779, 17.00000000000000000, 30.00000000000000000 ) ) ;
#7861 = ORIENTED_EDGE ( 'NONE', *, *, #41074, .F. ) ;
#7862 = CARTESIAN_POINT ( 'NONE',  ( -0.6440276692615888310, -16.64212148744554298, -9.683996418299976483 ) ) ;
#7863 = LINE ( 'NONE', #30960, #39723 ) ;
#7864 = CARTESIAN_POINT ( 'NONE',  ( 194.9999999999999716, 164.9999999999999716, 252.0000000000000000 ) ) ;
#7865 = ORIENTED_EDGE ( 'NONE', *, *, #11591, .T. ) ;
#7866 = VERTEX_POINT ( 'NONE', #30673 ) ;
#7867 = LINE ( 'NONE', #26842, #12318 ) ;
#7868 = FILL_AREA_STYLE_COLOUR ( '', #11202 ) ;
#7869 = VERTEX_POINT ( 'NONE', #49604 ) ;
#7870 = VERTEX_POINT ( 'NONE', #33511 ) ;
#7871 = EDGE_CURVE ( 'NONE', #418, #5585, #26314, .T. ) ;
#7872 = DIRECTION ( 'NONE',  ( -1.000000000000000000, 0.000000000000000000, -0.000000000000000000 ) ) ;
#7873 = ORIENTED_EDGE ( 'NONE', *, *, #13659, .F. ) ;
#7874 = VECTOR ( 'NONE', #46285, 1000.000000000000000 ) ;
#7875 = DIRECTION ( 'NONE',  ( -1.000000000000000000, -0.000000000000000000, -0.000000000000000000 ) ) ;
#7876 = CARTESIAN_POINT ( 'NONE',  ( -0.2050626648094178439, 1.807624707194796843, 9.903764339332081335 ) ) ;
#7877 = LINE ( 'NONE', #23521, #18742 ) ;
#7878 = CARTESIAN_POINT ( 'NONE',  ( 196.8526953830863420, -154.8119894309599260, 472.8425600500170844 ) ) ;
#7879 = VECTOR ( 'NONE', #40972, 1000.000000000000000 ) ;
#7880 = EDGE_LOOP ( 'NONE', ( #2585, #42701, #15661, #2157 ) ) ;
#7881 = LINE ( 'NONE', #42739, #9483 ) ;
#7883 = AXIS2_PLACEMENT_3D ( 'NONE', #12041, #27181, #14866 ) ;
#7882 = CARTESIAN_POINT ( 'NONE',  ( 339.9999999999999432, -181.0000000000001421, -356.0000000000003411 ) ) ;
#7884 = DIRECTION ( 'NONE',  ( 1.000000000000000000, 0.000000000000000000, 0.000000000000000000 ) ) ;
#7885 = CARTESIAN_POINT ( 'NONE',  ( 16.02661358026014327, 4.530191650547719995, -9.683996418299976483 ) ) ;
#7886 = AXIS2_PLACEMENT_3D ( 'NONE', #1232, #1723, #5562 ) ;
#7887 = AXIS2_PLACEMENT_3D ( 'NONE', #12328, #36209, #32352 ) ;
#7888 = VERTEX_POINT ( 'NONE', #49102 ) ;
#7889 = CARTESIAN_POINT ( 'NONE',  ( 9.260964247899973856, -13.84230907185609460, -9.683996418299976483 ) ) ;
#7890 = CARTESIAN_POINT ( 'NONE',  ( -34.08355720199904226, 2.371364769369340042, 7.455576670931136185 ) ) ;
#7891 = CARTESIAN_POINT ( 'NONE',  ( -0.9647729474495799762, -1.276880572101795286, 9.919954280166519922 ) ) ;
#7892 = AXIS2_PLACEMENT_3D ( 'NONE', #23735, #35819, #39404 ) ;
#7893 =( BOUNDED_CURVE ( )  B_SPLINE_CURVE ( 3, ( #31641, #12125, #27770, #35993 ),
 .UNSPECIFIED., .F., .F. ) 
 B_SPLINE_CURVE_WITH_KNOTS ( ( 4, 4 ),
 ( 3.141592653589793116, 4.712388980384689674 ),
 .UNSPECIFIED. ) 
 CURVE ( )  GEOMETRIC_REPRESENTATION_ITEM ( )  RATIONAL_B_SPLINE_CURVE ( ( 1.000000000000000000, 0.8047378541243649375, 0.8047378541243649375, 1.000000000000000000 ) ) 
 REPRESENTATION_ITEM ( '' )  );
#7894 = VERTEX_POINT ( 'NONE', #10650 ) ;
#7895 = DIRECTION ( 'NONE',  ( 1.000000000000000000, -0.000000000000000000, 0.000000000000000000 ) ) ;
#7896 = CARTESIAN_POINT ( 'NONE',  ( 344.0000000000000000, 185.0000000000000000, 359.9999999999998295 ) ) ;
#7897 = VERTEX_POINT ( 'NONE', #34020 ) ;
#7898 = CARTESIAN_POINT ( 'NONE',  ( 33.30402655318503946, -1.750000000000010214, 40.81828755692798438 ) ) ;
#7899 = EDGE_CURVE ( 'NONE', #27098, #45593, #21953, .T. ) ;
#7900 = FACE_OUTER_BOUND ( 'NONE', #31199, .T. ) ;
#7901 = DIRECTION ( 'NONE',  ( 0.000000000000000000, -1.000000000000000000, 8.021842663476564905E-17 ) ) ;
#7902 =( BOUNDED_CURVE ( )  B_SPLINE_CURVE ( 3, ( #9074, #13167, #20615, #12165 ),
 .UNSPECIFIED., .F., .F. ) 
 B_SPLINE_CURVE_WITH_KNOTS ( ( 4, 4 ),
 ( 4.712388980384689674, 6.283185307179586232 ),
 .UNSPECIFIED. ) 
 CURVE ( )  GEOMETRIC_REPRESENTATION_ITEM ( )  RATIONAL_B_SPLINE_CURVE ( ( 1.000000000000000000, 0.8047378541243649375, 0.8047378541243649375, 1.000000000000000000 ) ) 
 REPRESENTATION_ITEM ( '' )  );
#7903 = ORIENTED_EDGE ( 'NONE', *, *, #32396, .F. ) ;
#7904 = CARTESIAN_POINT ( 'NONE',  ( 0.6126904405382156416, 1.085824959725723016, 9.981352469109932457 ) ) ;
#7905 = ORIENTED_EDGE ( 'NONE', *, *, #47152, .T. ) ;
#7906 = VERTEX_POINT ( 'NONE', #33768 ) ;
#7907 = CARTESIAN_POINT ( 'NONE',  ( -0.8433491450857070193, 0.9182416014173486740, 9.981352469109932457 ) ) ;
#7908 = CARTESIAN_POINT ( 'NONE',  ( 210.0000000000000568, 0.000000000000000000, 160.8182875569279702 ) ) ;
#7909 = VECTOR ( 'NONE', #41910, 1000.000000000000000 ) ;
#7910 = VECTOR ( 'NONE', #1096, 1000.000000000000000 ) ;
#7911 = ORIENTED_EDGE ( 'NONE', *, *, #33741, .T. ) ;
#7912 = DIRECTION ( 'NONE',  ( 0.000000000000000000, -1.000000000000000000, -0.000000000000000000 ) ) ;
#7913 = CARTESIAN_POINT ( 'NONE',  ( 0.000000000000000000, -184.7999999999999545, -359.8000000000002387 ) ) ;
#7914 = VECTOR ( 'NONE', #50397, 1000.000000000000000 ) ;
#7915 =( BOUNDED_CURVE ( )  B_SPLINE_CURVE ( 3, ( #26402, #41554, #14601, #3300 ),
 .UNSPECIFIED., .F., .F. ) 
 B_SPLINE_CURVE_WITH_KNOTS ( ( 4, 4 ),
 ( 4.712388980384689674, 6.283185307179586232 ),
 .UNSPECIFIED. ) 
 CURVE ( )  GEOMETRIC_REPRESENTATION_ITEM ( )  RATIONAL_B_SPLINE_CURVE ( ( 1.000000000000000000, 0.8047378541243649375, 0.8047378541243649375, 1.000000000000000000 ) ) 
 REPRESENTATION_ITEM ( '' )  );
#7916 = DIRECTION ( 'NONE',  ( 2.220446049250312588E-16, 0.7071067811865475727, 0.7071067811865474617 ) ) ;
#7917 = VERTEX_POINT ( 'NONE', #18095 ) ;
#7918 = CARTESIAN_POINT ( 'NONE',  ( -206.6959734468149463, 1.750000000000010658, 120.8182875569279702 ) ) ;
#7919 = CARTESIAN_POINT ( 'NONE',  ( 113.3040265531850537, -1.749999999999997335, -119.1817124430720440 ) ) ;
#7920 = CARTESIAN_POINT ( 'NONE',  ( 135.0000000000015632, 16.00000000000000000, 60.00000000000000000 ) ) ;
#7921 = VECTOR ( 'NONE', #14402, 1000.000000000000000 ) ;
#7922 = ORIENTED_EDGE ( 'NONE', *, *, #13439, .T. ) ;
#7923 = CARTESIAN_POINT ( 'NONE',  ( 26.18032376592674737, -21.95228666728361233, 7.455576670931136185 ) ) ;
#7924 = LINE ( 'NONE', #43040, #21221 ) ;
#7925 = B_SPLINE_CURVE_WITH_KNOTS ( 'NONE', 3,
 ( #1624, #5459, #1377, #20606 ),
 .UNSPECIFIED., .F., .F.,
 ( 4, 4 ),
 ( 0.0008016012850907545907, 0.006940113526765079831 ),
 .UNSPECIFIED. ) ;
#7926 = ORIENTED_EDGE ( 'NONE', *, *, #40299, .F. ) ;
#7927 = ORIENTED_EDGE ( 'NONE', *, *, #18014, .F. ) ;
#7928 = VERTEX_POINT ( 'NONE', #34266 ) ;
#7929 = CARTESIAN_POINT ( 'NONE',  ( 115.0540265531850395, 2.143131898507842906E-16, 165.0000000000000000 ) ) ;
#7930 = CARTESIAN_POINT ( 'NONE',  ( -49.46074318306825290, 9.578883844007165749, 8.807470649214879543 ) ) ;
#7931 = ORIENTED_EDGE ( 'NONE', *, *, #4239, .T. ) ;
#7932 = VECTOR ( 'NONE', #16235, 1000.000000000000000 ) ;
#7933 = CARTESIAN_POINT ( 'NONE',  ( -164.9459734468149463, 2.143131898507880377E-16, -77.43171244307204404 ) ) ;
#7934 = CARTESIAN_POINT ( 'NONE',  ( 0.000000000000000000, 0.000000000000000000, 0.000000000000000000 ) ) ;
#7935 = DIRECTION ( 'NONE',  ( 0.1671032855531354722, -0.5142910309547729097, 0.8411784753765541023 ) ) ;
#7936 = CARTESIAN_POINT ( 'NONE',  ( -64.99999999999909051, 17.00000000000000000, -24.99999999999999289 ) ) ;
#7937 = CARTESIAN_POINT ( 'NONE',  ( -1.045807400993774339, 0.6549210616167606691, 9.969907203203804968 ) ) ;
#7938 = CARTESIAN_POINT ( 'NONE',  ( 0.000000000000000000, 175.0000000000000284, 346.2500000000002274 ) ) ;
#7939 = APPLICATION_CONTEXT ( 'automotive_design' ) ;
#7940 = CARTESIAN_POINT ( 'NONE',  ( 1.148889881503678545, 0.6106841242174666506, 9.986087673579140400 ) ) ;
#7941 = DIRECTION ( 'NONE',  ( 0.000000000000000000, 0.000000000000000000, 1.000000000000000000 ) ) ;
#7942 = CARTESIAN_POINT ( 'NONE',  ( -204.9459734468148895, -1.025126265847089435, -117.4317124430720156 ) ) ;
#7943 = LINE ( 'NONE', #46389, #47847 ) ;
#7944 = VECTOR ( 'NONE', #7089, 1000.000000000000000 ) ;
#7945 = CARTESIAN_POINT ( 'NONE',  ( 339.9999999999999432, 165.0000000000000000, -356.0000000000002274 ) ) ;
#7946 = DIRECTION ( 'NONE',  ( 1.000000000000000000, 0.000000000000000000, 0.000000000000000000 ) ) ;
#7947 = ORIENTED_EDGE ( 'NONE', *, *, #7832, .T. ) ;
#7948 = FACE_OUTER_BOUND ( 'NONE', #31414, .T. ) ;
#7949 = CARTESIAN_POINT ( 'NONE',  ( 115.0540265531850395, -1.025126265847081219, 159.0682875569279418 ) ) ;
#7950 = CARTESIAN_POINT ( 'NONE',  ( 71.55402655318505367, 0.000000000000000000, 159.0682875569279702 ) ) ;
#7951 = DIRECTION ( 'NONE',  ( 0.000000000000000000, -1.000000000000000000, 0.000000000000000000 ) ) ;
#7952 = ORIENTED_EDGE ( 'NONE', *, *, #7628, .T. ) ;
#7953 = DIRECTION ( 'NONE',  ( -0.000000000000000000, -0.000000000000000000, -1.000000000000000000 ) ) ;
#7954 = ORIENTED_EDGE ( 'NONE', *, *, #13638, .F. ) ;
#7955 = EDGE_CURVE ( 'NONE', #16183, #12977, #34177, .T. ) ;
#7956 = FACE_OUTER_BOUND ( 'NONE', #5618, .T. ) ;
#7957 = ORIENTED_EDGE ( 'NONE', *, *, #5507, .T. ) ;
#7958 = DIRECTION ( 'NONE',  ( -1.000000000000000000, 0.000000000000000000, 0.000000000000000000 ) ) ;
#7959 = EDGE_CURVE ( 'NONE', #34874, #30968, #21694, .T. ) ;
#7960 = DIRECTION ( 'NONE',  ( -1.000000000000000000, -0.000000000000000000, -0.000000000000000000 ) ) ;
#7961 = ORIENTED_EDGE ( 'NONE', *, *, #6863, .T. ) ;
#7962 = LINE ( 'NONE', #36171, #50231 ) ;
#7963 = ORIENTED_EDGE ( 'NONE', *, *, #30073, .T. ) ;
#7964 = ADVANCED_FACE ( 'NONE', ( #22705 ), #25808, .T. ) ;
#7965 = VECTOR ( 'NONE', #11123, 1000.000000000000000 ) ;
#7966 = EDGE_CURVE ( 'NONE', #34589, #41828, #25124, .T. ) ;
#7967 = ORIENTED_EDGE ( 'NONE', *, *, #43412, .T. ) ;
#7968 = DIRECTION ( 'NONE',  ( -0.000000000000000000, -1.000000000000000000, -0.000000000000000000 ) ) ;
#7969 = CARTESIAN_POINT ( 'NONE',  ( -206.6959734468149463, 1.750000000000010214, 40.81828755692798438 ) ) ;
#7970 = ORIENTED_EDGE ( 'NONE', *, *, #31606, .F. ) ;
#7971 = LINE ( 'NONE', #22591, #32778 ) ;
#7972 = CARTESIAN_POINT ( 'NONE',  ( 115.0540265531850395, 2.143131898507847836E-16, -77.43171244307204404 ) ) ;
#7973 = FACE_OUTER_BOUND ( 'NONE', #1830, .T. ) ;
#7974 = ORIENTED_EDGE ( 'NONE', *, *, #3272, .F. ) ;
#7975 = EDGE_CURVE ( 'NONE', #17766, #23241, #21897, .T. ) ;
#7976 = CARTESIAN_POINT ( 'NONE',  ( -165.0000000000000284, 16.00000000000000000, -114.9999999999999858 ) ) ;
#7977 = DIRECTION ( 'NONE',  ( -1.000000000000000000, -0.000000000000000000, -0.000000000000000000 ) ) ;
#7978 = ORIENTED_EDGE ( 'NONE', *, *, #534, .F. ) ;
#7979 = VECTOR ( 'NONE', #49252, 1000.000000000000000 ) ;
#7980 = CARTESIAN_POINT ( 'NONE',  ( 210.0000000000000568, 0.000000000000000000, 162.5682875569279702 ) ) ;
#7981 = DIRECTION ( 'NONE',  ( -1.586032880504786307E-16, 1.654361225106055350E-24, -1.000000000000000000 ) ) ;
#7982 = ORIENTED_EDGE ( 'NONE', *, *, #45528, .F. ) ;
#7983 = FACE_OUTER_BOUND ( 'NONE', #16547, .T. ) ;
#7984 = LINE ( 'NONE', #47184, #47201 ) ;
#7985 = ADVANCED_FACE ( 'NONE', ( #2451 ), #45674, .T. ) ;
#7986 = ORIENTED_EDGE ( 'NONE', *, *, #50225, .F. ) ;
#7987 = EDGE_CURVE ( 'NONE', #37507, #23383, #12372, .T. ) ;
#7988 = CARTESIAN_POINT ( 'NONE',  ( -54.99999999999997868, -52.50000000000000711, 5.000000000000000000 ) ) ;
#7989 = CYLINDRICAL_SURFACE ( 'NONE', #22488, 4.000000000000003553 ) ;
#7990 = CARTESIAN_POINT ( 'NONE',  ( 111.5540265531850679, 0.000000000000000000, -117.4317124430720725 ) ) ;
#7991 = DIRECTION ( 'NONE',  ( -1.000000000000000000, -0.000000000000000000, -0.000000000000000000 ) ) ;
#7992 = EDGE_CURVE ( 'NONE', #42209, #9166, #31184, .T. ) ;
#7993 = EDGE_CURVE ( 'NONE', #40596, #27788, #49341, .T. ) ;
#7994 = ORIENTED_EDGE ( 'NONE', *, *, #48677, .T. ) ;
#7995 =( BOUNDED_CURVE ( )  B_SPLINE_CURVE ( 3, ( #47585, #27883, #43512, #4522 ),
 .UNSPECIFIED., .F., .F. ) 
 B_SPLINE_CURVE_WITH_KNOTS ( ( 4, 4 ),
 ( 4.712388980384689674, 6.283185307179586232 ),
 .UNSPECIFIED. ) 
 CURVE ( )  GEOMETRIC_REPRESENTATION_ITEM ( )  RATIONAL_B_SPLINE_CURVE ( ( 1.000000000000000000, 0.8047378541243649375, 0.8047378541243649375, 1.000000000000000000 ) ) 
 REPRESENTATION_ITEM ( '' )  );
#7996 = CARTESIAN_POINT ( 'NONE',  ( -1.782521105131510186, 0.3635605703594341209, 9.903764339332088440 ) ) ;
#7997 = EDGE_CURVE ( 'NONE', #41585, #27664, #50364, .T. ) ;
#7998 = FACE_OUTER_BOUND ( 'NONE', #19370, .T. ) ;
#7999 = EDGE_CURVE ( 'NONE', #48485, #48152, #37290, .T. ) ;
#8000 = DIRECTION ( 'NONE',  ( -0.000000000000000000, -0.000000000000000000, -1.000000000000000000 ) ) ;
#8001 = VERTEX_POINT ( 'NONE', #35545 ) ;
#8002 = ORIENTED_EDGE ( 'NONE', *, *, #45371, .T. ) ;
#8003 = SHAPE_DEFINITION_REPRESENTATION ( #32675, #45699 ) ;
#8004 = CARTESIAN_POINT ( 'NONE',  ( -207.2473046169136808, -154.8119894309599260, 23.74256005001722158 ) ) ;
#8005 = CARTESIAN_POINT ( 'NONE',  ( 344.0000000000000000, -164.9999999999999432, 339.9999999999998295 ) ) ;
#8006 = CARTESIAN_POINT ( 'NONE',  ( 191.5540265531851105, 0.000000000000000000, 39.06828755692798438 ) ) ;
#8007 = CARTESIAN_POINT ( 'NONE',  ( -204.9459734468148895, -1.025126265847088991, -157.4317124430720582 ) ) ;
#8008 = DIRECTION ( 'NONE',  ( 0.000000000000000000, -1.000000000000000000, 0.000000000000000000 ) ) ;
#8009 = ORIENTED_EDGE ( 'NONE', *, *, #20165, .F. ) ;
#8010 = CARTESIAN_POINT ( 'NONE',  ( -48.44597344681495343, 0.000000000000000000, -77.43171244307198720 ) ) ;
#8011 = DIRECTION ( 'NONE',  ( -0.000000000000000000, 1.000000000000000000, 0.000000000000000000 ) ) ;
#8012 = FACE_OUTER_BOUND ( 'NONE', #29019, .T. ) ;
#8013 = EDGE_CURVE ( 'NONE', #48818, #16044, #12181, .T. ) ;
#8014 = CYLINDRICAL_SURFACE ( 'NONE', #28099, 2.000000000000001776 ) ;
#8015 = ORIENTED_EDGE ( 'NONE', *, *, #46886, .T. ) ;
#8016 = EDGE_CURVE ( 'NONE', #28737, #16142, #27014, .T. ) ;
#8017 = CARTESIAN_POINT ( 'NONE',  ( 210.0000000000000568, 2.143131898507880377E-16, -160.9317124430720298 ) ) ;
#8019 = ORIENTED_EDGE ( 'NONE', *, *, #4675, .T. ) ;
#8018 = CIRCLE ( 'NONE', #48092, 1.750000000000015543 ) ;
#8020 = EDGE_CURVE ( 'NONE', #39370, #47399, #16281, .T. ) ;
#8021 = DIRECTION ( 'NONE',  ( -1.000000000000000000, 0.000000000000000000, 0.000000000000000000 ) ) ;
#8022 = ORIENTED_EDGE ( 'NONE', *, *, #36864, .F. ) ;
#8023 = DIRECTION ( 'NONE',  ( 1.000000000000000000, 0.000000000000000000, 1.612977847700450206E-50 ) ) ;
#8024 = CARTESIAN_POINT ( 'NONE',  ( -14.99999999999906919, 16.00000000000000000, 0.000000000000000000 ) ) ;
#8025 = B_SPLINE_CURVE_WITH_KNOTS ( 'NONE', 3,
 ( #43057, #7937, #31541, #47128 ),
 .UNSPECIFIED., .F., .F.,
 ( 4, 4 ),
 ( 0.000000000000000000, 0.0002610106747150578552 ),
 .UNSPECIFIED. ) ;
#8026 = DIRECTION ( 'NONE',  ( -0.000000000000000000, -1.000000000000000000, -0.000000000000000000 ) ) ;
#8027 = ORIENTED_EDGE ( 'NONE', *, *, #48379, .T. ) ;
#8028 = EDGE_CURVE ( 'NONE', #3051, #36488, #3716, .T. ) ;
#8029 = DIRECTION ( 'NONE',  ( 0.000000000000000000, 5.664403186863042467E-17, 1.000000000000000000 ) ) ;
#8030 = ORIENTED_EDGE ( 'NONE', *, *, #47446, .F. ) ;
#8031 = LINE ( 'NONE', #7779, #37794 ) ;
#8032 = CARTESIAN_POINT ( 'NONE',  ( 3.087186397306452612, 2.514307945609885131, -2.642742795433417058E-16 ) ) ;
#8033 = DIRECTION ( 'NONE',  ( 0.000000000000000000, 0.000000000000000000, 1.000000000000000000 ) ) ;
#8034 = VECTOR ( 'NONE', #50342, 1000.000000000000000 ) ;
#8035 = ORIENTED_EDGE ( 'NONE', *, *, #13046, .T. ) ;
#8036 = ORIENTED_EDGE ( 'NONE', *, *, #12499, .T. ) ;
#8037 = CARTESIAN_POINT ( 'NONE',  ( 7.241383964640743187, 3.469446951953614189E-15, 5.000000000000000000 ) ) ;
#8038 = EDGE_CURVE ( 'NONE', #17953, #26847, #27065, .T. ) ;
#8039 = ORIENTED_EDGE ( 'NONE', *, *, #19692, .T. ) ;
#8040 = LINE ( 'NONE', #7790, #35624 ) ;
#8041 = DIRECTION ( 'NONE',  ( 1.000000000000000000, 0.000000000000000000, 0.000000000000000000 ) ) ;
#8042 = PLANE ( 'NONE',  #14972 ) ;
#8043 = EDGE_CURVE ( 'NONE', #43960, #48553, #23208, .T. ) ;
#8044 = EDGE_LOOP ( 'NONE', ( #49176, #49626, #22471, #10972, #32273, #48504 ) ) ;
#8045 = CARTESIAN_POINT ( 'NONE',  ( -48.44597344681495343, 0.000000000000000000, 165.0000000000000000 ) ) ;
#8046 = ORIENTED_EDGE ( 'NONE', *, *, #23529, .F. ) ;
#8047 = DIRECTION ( 'NONE',  ( 1.156482317317870492E-16, -1.000000000000000000, -0.000000000000000000 ) ) ;
#8048 = DIRECTION ( 'NONE',  ( 0.5038710255240862468, 0.000000000000000000, 0.8637789008984334549 ) ) ;
#8049 =( BOUNDED_CURVE ( )  B_SPLINE_CURVE ( 3, ( #46417, #33904, #6947, #18985 ),
 .UNSPECIFIED., .F., .F. ) 
 B_SPLINE_CURVE_WITH_KNOTS ( ( 4, 4 ),
 ( 0.000000000000000000, 1.570796326794896558 ),
 .UNSPECIFIED. ) 
 CURVE ( )  GEOMETRIC_REPRESENTATION_ITEM ( )  RATIONAL_B_SPLINE_CURVE ( ( 1.000000000000000000, 0.8047378541243649375, 0.8047378541243649375, 1.000000000000000000 ) ) 
 REPRESENTATION_ITEM ( '' )  );
#8050 = FACE_OUTER_BOUND ( 'NONE', #9334, .T. ) ;
#8051 = ADVANCED_FACE ( 'NONE', ( #47541 ), #4234, .T. ) ;
#8053 = ORIENTED_EDGE ( 'NONE', *, *, #1852, .F. ) ;
#8052 = EDGE_CURVE ( 'NONE', #40121, #28181, #11932, .T. ) ;
#8054 = VECTOR ( 'NONE', #44551, 1000.000000000000000 ) ;
#8055 = EDGE_LOOP ( 'NONE', ( #11064, #23799, #36833, #24824 ) ) ;
#8056 = ORIENTED_EDGE ( 'NONE', *, *, #40839, .T. ) ;
#8057 = LINE ( 'NONE', #16001, #38629 ) ;
#8058 =( BOUNDED_CURVE ( )  B_SPLINE_CURVE ( 3, ( #2815, #10026, #33890, #14885 ),
 .UNSPECIFIED., .F., .F. ) 
 B_SPLINE_CURVE_WITH_KNOTS ( ( 4, 4 ),
 ( 1.570796326794896558, 3.141592653589793116 ),
 .UNSPECIFIED. ) 
 CURVE ( )  GEOMETRIC_REPRESENTATION_ITEM ( )  RATIONAL_B_SPLINE_CURVE ( ( 1.000000000000000000, 0.8047378541243649375, 0.8047378541243649375, 1.000000000000000000 ) ) 
 REPRESENTATION_ITEM ( '' )  );
#8059 = CARTESIAN_POINT ( 'NONE',  ( 3.566525152641073504, -1.569997364302916809, 9.741991644047246268 ) ) ;
#8060 = EDGE_CURVE ( 'NONE', #26993, #48818, #4475, .T. ) ;
#8061 = EDGE_LOOP ( 'NONE', ( #11844, #40146, #23727, #25445 ) ) ;
#8062 = CARTESIAN_POINT ( 'NONE',  ( 115.0540265531850679, 0.000000000000000000, 162.5682875569279702 ) ) ;
#8063 = ORIENTED_EDGE ( 'NONE', *, *, #4044, .T. ) ;
#8064 = EDGE_CURVE ( 'NONE', #46163, #28405, #42779, .T. ) ;
#8065 = PLANE ( 'NONE',  #34857 ) ;
#8066 = ORIENTED_EDGE ( 'NONE', *, *, #1572, .F. ) ;
#8067 = ADVANCED_FACE ( 'NONE', ( #3448 ), #12922, .F. ) ;
#8068 = LINE ( 'NONE', #23189, #38362 ) ;
#8069 = DIRECTION ( 'NONE',  ( -0.000000000000000000, -1.000000000000000000, -0.000000000000000000 ) ) ;
#8070 = LINE ( 'NONE', #23708, #17639 ) ;
#8071 = CARTESIAN_POINT ( 'NONE',  ( 358.0000000000000568, -167.8284271247462414, 342.8284271247461561 ) ) ;
#8072 = CARTESIAN_POINT ( 'NONE',  ( 4.763548243873389154, -16.57409059453848599, 8.727788335465566760 ) ) ;
#8073 = ORIENTED_EDGE ( 'NONE', *, *, #20226, .T. ) ;
#8074 = ORIENTED_EDGE ( 'NONE', *, *, #41579, .T. ) ;
#8075 = DIRECTION ( 'NONE',  ( -0.000000000000000000, -0.000000000000000000, -1.000000000000000000 ) ) ;
#8076 = B_SPLINE_SURFACE_WITH_KNOTS ( 'NONE', 3, 3, ( 
 ( #25750, #48036, #17034, #41136 ),
 ( #33458, #1648, #21381, #13685 ),
 ( #36569, #17289, #5483, #44956 ),
 ( #5233, #13926, #37069, #32962 ) ),
 .UNSPECIFIED., .F., .F., .F.,
 ( 4, 4 ),
 ( 4, 4 ),
 ( 0.000000000000000000, 1.000000000000000000 ),
 ( 0.000000000000000000, 1.000000000000000000 ),
 .UNSPECIFIED. ) ;
#8077 = DIRECTION ( 'NONE',  ( 0.000000000000000000, 1.000000000000000000, 0.000000000000000000 ) ) ;
#8078 = CARTESIAN_POINT ( 'NONE',  ( 114.3291528190321173, -1.749999999999996669, 41.84341382277508359 ) ) ;
#8079 = CARTESIAN_POINT ( 'NONE',  ( -16.52264463346130796, 2.779753662172870232, 9.403735324607438884 ) ) ;
#8080 = EDGE_CURVE ( 'NONE', #39358, #13701, #35207, .T. ) ;
#8081 = CARTESIAN_POINT ( 'NONE',  ( -29.18392875402943432, -17.44843138996582965, 7.906207997025717304 ) ) ;
#8082 = EDGE_LOOP ( 'NONE', ( #35213, #15987, #29822, #26821, #47039, #4758, #23954, #45682 ) ) ;
#8083 = FACE_OUTER_BOUND ( 'NONE', #49608, .T. ) ;
#8084 = EDGE_LOOP ( 'NONE', ( #47393, #9425, #35742, #33035, #8592 ) ) ;
#8085 = AXIS2_PLACEMENT_3D ( 'NONE', #29140, #26299, #33502 ) ;
#8086 = DIRECTION ( 'NONE',  ( 0.000000000000000000, -1.000000000000000000, 3.469446951953611033E-15 ) ) ;
#8087 = CARTESIAN_POINT ( 'NONE',  ( -10.30302290646040575, -13.08520913973572419, -9.683996418299976483 ) ) ;
#8088 = CARTESIAN_POINT ( 'NONE',  ( 35.00000000000028422, 16.00000000000000000, -84.99999999999998579 ) ) ;
#8089 = ORIENTED_EDGE ( 'NONE', *, *, #1664, .F. ) ;
#8090 = CLOSED_SHELL ( 'NONE', ( #17781, #1511, #16443, #1412, #28219, #30596, #32262, #13065, #1406, #38290, #27511, #40150, #38230, #433, #20518, #44413, #46795, #30209 ) ) ;
#8091 = ORIENTED_EDGE ( 'NONE', *, *, #26570, .F. ) ;
#8092 = PLANE ( 'NONE',  #7892 ) ;
#8093 = LINE ( 'NONE', #49851, #15649 ) ;
#8094 = ORIENTED_EDGE ( 'NONE', *, *, #40299, .T. ) ;
#8095 = ORIENTED_EDGE ( 'NONE', *, *, #40998, .T. ) ;
#8096 = CARTESIAN_POINT ( 'NONE',  ( 210.0000000000000568, 0.000000000000000000, 122.5682875569279844 ) ) ;
#8097 = FACE_OUTER_BOUND ( 'NONE', #37955, .T. ) ;
#8098 = CARTESIAN_POINT ( 'NONE',  ( -5.000000000000000000, -175.0000000000000284, -353.7500000000001705 ) ) ;
#8099 = CARTESIAN_POINT ( 'NONE',  ( 181.0000000000000000, -174.9999999999999716, -358.0000000000001705 ) ) ;
#8100 = EDGE_LOOP ( 'NONE', ( #32067, #29360, #29865, #4785 ) ) ;
#8101 = ORIENTED_EDGE ( 'NONE', *, *, #38820, .T. ) ;
#8102 = EDGE_LOOP ( 'NONE', ( #42979, #18110, #18413, #46439 ) ) ;
#8103 = CARTESIAN_POINT ( 'NONE',  ( -6.695973446814940111, -1.750000000000023759, 40.81828755692798438 ) ) ;
#8104 = ORIENTED_EDGE ( 'NONE', *, *, #16854, .F. ) ;
#8105 = EDGE_CURVE ( 'NONE', #47659, #26079, #19557, .T. ) ;
#8106 = CARTESIAN_POINT ( 'NONE',  ( 3.229232847726260403, -16.57333684275945629, 9.178419661560148768 ) ) ;
#8107 = EDGE_CURVE ( 'NONE', #5904, #36298, #25241, .T. ) ;
#8108 = CARTESIAN_POINT ( 'NONE',  ( 31.55402655318503236, 0.000000000000000000, 165.0000000000000000 ) ) ;
#8109 = CARTESIAN_POINT ( 'NONE',  ( -49.46074318306825290, 9.578883844007165749, 8.807470649214879543 ) ) ;
#8110 = ORIENTED_EDGE ( 'NONE', *, *, #21721, .T. ) ;
#8111 = VERTEX_POINT ( 'NONE', #1897 ) ;
#8112 = DIRECTION ( 'NONE',  ( -0.000000000000000000, -0.000000000000000000, -1.000000000000000000 ) ) ;
#8113 = CARTESIAN_POINT ( 'NONE',  ( -6.695973446814940111, 0.000000000000000000, 165.0000000000000000 ) ) ;
#8114 = LINE ( 'NONE', #42477, #17528 ) ;
#8115 = ADVANCED_FACE ( 'NONE', ( #32690, #28840 ), #9343, .T. ) ;
#8116 = ORIENTED_EDGE ( 'NONE', *, *, #20542, .F. ) ;
#8117 = ORIENTED_EDGE ( 'NONE', *, *, #9951, .F. ) ;
#8118 = EDGE_CURVE ( 'NONE', #27665, #20648, #36054, .T. ) ;
#8119 = CARTESIAN_POINT ( 'NONE',  ( 193.3040265531851105, 1.750000000000010658, 120.8182875569279702 ) ) ;
#8120 = CARTESIAN_POINT ( 'NONE',  ( -165.6708471809677974, 1.750000000000010214, -80.20683870891910772 ) ) ;
#8122 = ORIENTED_EDGE ( 'NONE', *, *, #22908, .F. ) ;
#8121 = VECTOR ( 'NONE', #23458, 1000.000000000000000 ) ;
#8123 = ADVANCED_FACE ( 'NONE', ( #898 ), #29719, .T. ) ;
#8124 = LINE ( 'NONE', #39180, #48541 ) ;
#8125 = CARTESIAN_POINT ( 'NONE',  ( 340.0000000000000568, 169.0000000000000000, 343.9999999999998295 ) ) ;
#8126 = DIRECTION ( 'NONE',  ( 1.000000000000000000, 0.000000000000000000, 0.000000000000000000 ) ) ;
#8127 = VECTOR ( 'NONE', #27437, 1000.000000000000000 ) ;
#8128 = CARTESIAN_POINT ( 'NONE',  ( 2.210477865340801706, 37.43479381012853224, -9.422646554964178023 ) ) ;
#8129 = AXIS2_PLACEMENT_3D ( 'NONE', #19078, #12156, #3688 ) ;
#8130 = ORIENTED_EDGE ( 'NONE', *, *, #20197, .F. ) ;
#8131 = VECTOR ( 'NONE', #48179, 1000.000000000000000 ) ;
#8132 = CARTESIAN_POINT ( 'NONE',  ( 191.5540265531851105, 2.143131898507880377E-16, -160.9317124430720298 ) ) ;
#8133 = CARTESIAN_POINT ( 'NONE',  ( -47.72109971266203132, 1.750000000000010436, -80.20683870891910772 ) ) ;
#8134 = EDGE_CURVE ( 'NONE', #8840, #6226, #47999, .T. ) ;
#8135 = FACE_OUTER_BOUND ( 'NONE', #29371, .T. ) ;
#8136 = CIRCLE ( 'NONE', #47408, 8.000000000000000000 ) ;
#8137 = DIRECTION ( 'NONE',  ( -0.000000000000000000, -0.000000000000000000, -1.000000000000000000 ) ) ;
#8138 = AXIS2_PLACEMENT_3D ( 'NONE', #11867, #27527, #7514 ) ;
#8139 = LINE ( 'NONE', #44261, #14689 ) ;
#8140 = CARTESIAN_POINT ( 'NONE',  ( 113.3040265531850537, 1.749999999999997113, 40.81828755692798438 ) ) ;
#8141 = CARTESIAN_POINT ( 'NONE',  ( -0.9306598006161299619, -1.429916298923569862, 9.912102921405038458 ) ) ;
#8142 = ORIENTED_EDGE ( 'NONE', *, *, #30192, .T. ) ;
#8143 =( NAMED_UNIT ( * ) PLANE_ANGLE_UNIT ( ) SI_UNIT ( $, .RADIAN. ) );
#8144 = ORIENTED_EDGE ( 'NONE', *, *, #852, .F. ) ;
#8145 = CARTESIAN_POINT ( 'NONE',  ( -84.94597344681493212, -1.025126265847089435, -77.43171244307200141 ) ) ;
#8146 = CARTESIAN_POINT ( 'NONE',  ( -208.4459734468149463, 0.000000000000000000, 162.5682875569279702 ) ) ;
#8147 = CARTESIAN_POINT ( 'NONE',  ( -84.94597344681493212, -1.025126265847089435, 82.56828755692798438 ) ) ;
#8148 = ORIENTED_EDGE ( 'NONE', *, *, #5237, .F. ) ;
#8149 = PLANE ( 'NONE',  #11807 ) ;
#8150 = ORIENTED_EDGE ( 'NONE', *, *, #26022, .F. ) ;
#8151 = EDGE_LOOP ( 'NONE', ( #29381, #32027, #44052, #18604 ) ) ;
#8152 = CARTESIAN_POINT ( 'NONE',  ( 15.57957361750251302, 5.755602074545510760, 3.266473740018926541 ) ) ;
#8153 = ADVANCED_FACE ( 'NONE', ( #13436 ), #36571, .F. ) ;
#8154 = DIRECTION ( 'NONE',  ( 0.4740998230350172427, -0.3386427307392981811, -0.8127425537743158124 ) ) ;
#8155 = AXIS2_PLACEMENT_3D ( 'NONE', #8265, #35740, #27761 ) ;
#8156 = VECTOR ( 'NONE', #37117, 1000.000000000000000 ) ;
#8157 = ORIENTED_EDGE ( 'NONE', *, *, #46351, .F. ) ;
#8158 = DIRECTION ( 'NONE',  ( -0.000000000000000000, -0.000000000000000000, -1.000000000000000000 ) ) ;
#8159 = CARTESIAN_POINT ( 'NONE',  ( -114.9999999999981526, 17.00000000000000000, 65.00000000000000000 ) ) ;
#8160 = VECTOR ( 'NONE', #2967, 1000.000000000000000 ) ;
#8161 = CIRCLE ( 'NONE', #31085, 1.749999999999987566 ) ;
#8162 = LINE ( 'NONE', #46602, #40702 ) ;
#8163 = ORIENTED_EDGE ( 'NONE', *, *, #21130, .F. ) ;
#8164 = DIRECTION ( 'NONE',  ( 0.000000000000000000, -1.000000000000000000, 0.000000000000000000 ) ) ;
#8165 = CARTESIAN_POINT ( 'NONE',  ( -21.85563210430627024, -40.58578877481918568, 8.807470649214879543 ) ) ;
#8166 = DIRECTION ( 'NONE',  ( 0.000000000000000000, -1.000000000000000000, 0.000000000000000000 ) ) ;
#8167 = AXIS2_PLACEMENT_3D ( 'NONE', #11417, #637, #27592 ) ;
#8168 = ORIENTED_EDGE ( 'NONE', *, *, #31034, .T. ) ;
#8169 = DIRECTION ( 'NONE',  ( 1.000000000000000000, 0.000000000000000000, 7.793956916774525800E-48 ) ) ;
#8170 = LINE ( 'NONE', #19949, #43335 ) ;
#8171 = ORIENTED_EDGE ( 'NONE', *, *, #21153, .T. ) ;
#8172 = VERTEX_POINT ( 'NONE', #28336 ) ;
#8173 = ORIENTED_EDGE ( 'NONE', *, *, #5807, .F. ) ;
#8174 = LINE ( 'NONE', #38974, #41801 ) ;
#8175 = LINE ( 'NONE', #4806, #25023 ) ;
#8176 = VERTEX_POINT ( 'NONE', #1149 ) ;
#8177 = DIRECTION ( 'NONE',  ( -1.000000000000000000, 0.000000000000000000, 0.000000000000000000 ) ) ;
#8178 = DIRECTION ( 'NONE',  ( 0.000000000000000000, 0.000000000000000000, -1.000000000000000000 ) ) ;
#8179 = PLANE ( 'NONE',  #37093 ) ;
#8180 = CARTESIAN_POINT ( 'NONE',  ( -5.000000000000000000, -165.1999999999999602, 340.1999999999997044 ) ) ;
#8181 = CARTESIAN_POINT ( 'NONE',  ( 210.0000000000000568, 0.000000000000000000, -79.18171244307201562 ) ) ;
#8182 = CARTESIAN_POINT ( 'NONE',  ( 153.3040265531850537, -1.750000000000010658, 120.8182875569279702 ) ) ;
#8183 = CARTESIAN_POINT ( 'NONE',  ( -208.4459734468149463, 0.000000000000000000, 39.06828755692798438 ) ) ;
#8185 = EDGE_CURVE ( 'NONE', #10383, #26504, #17036, .T. ) ;
#8184 = CARTESIAN_POINT ( 'NONE',  ( -86.69597344681494633, -1.750000000000009992, 160.8182875569279702 ) ) ;
#8186 = CARTESIAN_POINT ( 'NONE',  ( 1.424123654779712922, 0.3625862473308184009, 9.958264684458541183 ) ) ;
#8187 = DIRECTION ( 'NONE',  ( 0.000000000000000000, 1.000000000000000000, 6.123233995736766036E-17 ) ) ;
#8188 = CARTESIAN_POINT ( 'NONE',  ( -225.0000000000000568, 164.9999999999999716, 132.0000000000000000 ) ) ;
#8189 = VECTOR ( 'NONE', #41024, 1000.000000000000000 ) ;
#8190 = VECTOR ( 'NONE', #21831, 1000.000000000000000 ) ;
#8191 = DIRECTION ( 'NONE',  ( -1.000000000000000000, -0.000000000000000000, -0.000000000000000000 ) ) ;
#8192 =( BOUNDED_CURVE ( )  B_SPLINE_CURVE ( 3, ( #38602, #30904, #42415, #34757 ),
 .UNSPECIFIED., .F., .F. ) 
 B_SPLINE_CURVE_WITH_KNOTS ( ( 4, 4 ),
 ( 4.712388980384689674, 6.283185307179586232 ),
 .UNSPECIFIED. ) 
 CURVE ( )  GEOMETRIC_REPRESENTATION_ITEM ( )  RATIONAL_B_SPLINE_CURVE ( ( 1.000000000000000000, 0.8047378541243649375, 0.8047378541243649375, 1.000000000000000000 ) ) 
 REPRESENTATION_ITEM ( '' )  );
#8193 = CARTESIAN_POINT ( 'NONE',  ( 153.3040265531850537, 1.750000000000009992, 0.8182875569279768335 ) ) ;
#8194 = AXIS2_PLACEMENT_3D ( 'NONE', #2869, #49030, #33947 ) ;
#8195 = CARTESIAN_POINT ( 'NONE',  ( 14.49999999999999822, -46.01315789473684248, 5.916985404131813731 ) ) ;
#8196 = LINE ( 'NONE', #39246, #33058 ) ;
#8197 = ORIENTED_EDGE ( 'NONE', *, *, #13591, .T. ) ;
#8198 = AXIS2_PLACEMENT_3D ( 'NONE', #36722, #1791, #13580 ) ;
#8199 = LINE ( 'NONE', #39504, #40105 ) ;
#8200 =( BOUNDED_CURVE ( )  B_SPLINE_CURVE ( 3, ( #40921, #10120, #9868, #6013 ),
 .UNSPECIFIED., .F., .F. ) 
 B_SPLINE_CURVE_WITH_KNOTS ( ( 4, 4 ),
 ( 0.000000000000000000, 1.570796326794896558 ),
 .UNSPECIFIED. ) 
 CURVE ( )  GEOMETRIC_REPRESENTATION_ITEM ( )  RATIONAL_B_SPLINE_CURVE ( ( 1.000000000000000000, 0.8047378541243649375, 0.8047378541243649375, 1.000000000000000000 ) ) 
 REPRESENTATION_ITEM ( '' )  );
#8201 = CARTESIAN_POINT ( 'NONE',  ( 0.8811857040074689840, 1.919576306124735510, 9.890170120223995553 ) ) ;
#8202 = CARTESIAN_POINT ( 'NONE',  ( 168.9999999999999716, -164.9999999999999432, -358.0000000000001705 ) ) ;
#8203 = DIRECTION ( 'NONE',  ( 1.000000000000000000, 0.000000000000000000, 0.000000000000000000 ) ) ;
#8204 = CIRCLE ( 'NONE', #27053, 6.000000000000000888 ) ;
#8205 = ORIENTED_EDGE ( 'NONE', *, *, #8923, .F. ) ;
#8206 = CARTESIAN_POINT ( 'NONE',  ( -0.9987333402973620489, -1.123935354445870338, 9.936141075690079205 ) ) ;
#8207 = VERTEX_POINT ( 'NONE', #21382 ) ;
#8208 = DIRECTION ( 'NONE',  ( -1.000000000000000000, 0.000000000000000000, -7.793956916774525800E-48 ) ) ;
#8209 = VERTEX_POINT ( 'NONE', #40651 ) ;
#8210 = PLANE ( 'NONE',  #32847 ) ;
#8211 = CARTESIAN_POINT ( 'NONE',  ( 115.0540265531850395, 2.143131898507847836E-16, -0.9317124430719969652 ) ) ;
#8212 =( BOUNDED_CURVE ( )  B_SPLINE_CURVE ( 3, ( #24221, #16261, #28563, #24474 ),
 .UNSPECIFIED., .F., .F. ) 
 B_SPLINE_CURVE_WITH_KNOTS ( ( 4, 4 ),
 ( 3.141592653589793116, 4.712388980384689674 ),
 .UNSPECIFIED. ) 
 CURVE ( )  GEOMETRIC_REPRESENTATION_ITEM ( )  RATIONAL_B_SPLINE_CURVE ( ( 1.000000000000000000, 0.8047378541243649375, 0.8047378541243649375, 1.000000000000000000 ) ) 
 REPRESENTATION_ITEM ( '' )  );
#8213 = EDGE_LOOP ( 'NONE', ( #40311, #17819, #47034, #17786 ) ) ;
#8214 = LINE ( 'NONE', #761, #32292 ) ;
#8215 = ORIENTED_EDGE ( 'NONE', *, *, #49247, .F. ) ;
#8216 = ADVANCED_FACE ( 'NONE', ( #5484 ), #34217, .T. ) ;
#8217 = ORIENTED_EDGE ( 'NONE', *, *, #36565, .F. ) ;
#8218 = CARTESIAN_POINT ( 'NONE',  ( -164.9459734468149463, 2.143131898507880377E-16, 159.0682875569279702 ) ) ;
#8219 = ORIENTED_EDGE ( 'NONE', *, *, #22109, .F. ) ;
#8220 = DIRECTION ( 'NONE',  ( -1.000000000000000000, 0.000000000000000000, 0.000000000000000000 ) ) ;
#8221 = CARTESIAN_POINT ( 'NONE',  ( -114.9999999999978542, 16.00000000000000000, 95.00000000000000000 ) ) ;
#8222 = DIRECTION ( 'NONE',  ( -0.000000000000000000, -1.000000000000000000, -0.000000000000000000 ) ) ;
#8223 = CARTESIAN_POINT ( 'NONE',  ( -54.99999999999997868, -52.50000000000000711, -5.000000000000000000 ) ) ;
#8224 = AXIS2_PLACEMENT_3D ( 'NONE', #33779, #18351, #41716 ) ;
#8225 = LINE ( 'NONE', #39785, #29672 ) ;
#8226 = VECTOR ( 'NONE', #28010, 1000.000000000000000 ) ;
#8227 = ORIENTED_EDGE ( 'NONE', *, *, #28048, .T. ) ;
#8228 = CARTESIAN_POINT ( 'NONE',  ( 0.000000000000000000, 169.0000000000000000, 341.9999999999997726 ) ) ;
#8229 = VECTOR ( 'NONE', #16574, 1000.000000000000000 ) ;
#8230 = CARTESIAN_POINT ( 'NONE',  ( 0.000000000000000000, 169.0000000000000000, -340.0000000000001705 ) ) ;
#8231 = VERTEX_POINT ( 'NONE', #33710 ) ;
#8232 = CARTESIAN_POINT ( 'NONE',  ( 1.637520033018233345, 0.1700351954323681691, 9.927568724237806563 ) ) ;
#8233 = AXIS2_PLACEMENT_3D ( 'NONE', #39734, #40734, #9423 ) ;
#8234 = AXIS2_PLACEMENT_3D ( 'NONE', #29245, #25150, #48690 ) ;
#8235 = DIRECTION ( 'NONE',  ( -0.000000000000000000, -1.000000000000000000, -0.000000000000000000 ) ) ;
#8236 = VERTEX_POINT ( 'NONE', #33954 ) ;
#8237 = CARTESIAN_POINT ( 'NONE',  ( 356.0000000000000000, 175.0000000000000284, -106.0000000000001990 ) ) ;
#8238 = DIRECTION ( 'NONE',  ( -0.000000000000000000, -0.000000000000000000, 1.000000000000000000 ) ) ;
#8239 = CARTESIAN_POINT ( 'NONE',  ( 154.1026953830863420, 103.9380105690400597, 22.84256005001721945 ) ) ;
#8240 = DIRECTION ( 'NONE',  ( 0.000000000000000000, 0.000000000000000000, 1.000000000000000000 ) ) ;
#8241 = VERTEX_POINT ( 'NONE', #22394 ) ;
#8242 = CARTESIAN_POINT ( 'NONE',  ( 350.0000000000000000, 181.0000000000000284, -344.0000000000001705 ) ) ;
#8244 = EDGE_CURVE ( 'NONE', #18475, #35109, #38066, .T. ) ;
#8243 = PLANE ( 'NONE',  #16892 ) ;
#8245 = DIRECTION ( 'NONE',  ( -1.000000000000000000, 0.000000000000000000, 0.000000000000000000 ) ) ;
#8246 = ORIENTED_EDGE ( 'NONE', *, *, #19219, .T. ) ;
#8247 = ORIENTED_EDGE ( 'NONE', *, *, #46136, .F. ) ;
#8248 = CARTESIAN_POINT ( 'NONE',  ( 5.505322767148756569, -37.09368438467003415, 8.914903342594564961 ) ) ;
#8249 = CARTESIAN_POINT ( 'NONE',  ( -1.133908876584336367, -0.5183204401656656968, 9.981352469109934233 ) ) ;
#8250 = CARTESIAN_POINT ( 'NONE',  ( -20.40054609052957701, 26.26366202847989229, -3.760136334089591248 ) ) ;
#8251 = CARTESIAN_POINT ( 'NONE',  ( 154.3291528190321458, -1.750000000000010436, -120.2068387089191219 ) ) ;
#8252 = EDGE_LOOP ( 'NONE', ( #20325, #2814, #50459, #9150 ) ) ;
#8253 = LINE ( 'NONE', #40066, #20633 ) ;
#8254 = EDGE_CURVE ( 'NONE', #10051, #10114, #26008, .T. ) ;
#8255 = EDGE_CURVE ( 'NONE', #24755, #50534, #32739, .T. ) ;
#8256 = CARTESIAN_POINT ( 'NONE',  ( 31.55402655318503236, 0.000000000000000000, 82.56828755692798438 ) ) ;
#8257 = DIRECTION ( 'NONE',  ( -1.000000000000000000, -0.000000000000000000, -0.000000000000000000 ) ) ;
#8258 = CARTESIAN_POINT ( 'NONE',  ( 358.0000000000000000, 174.9999999999996589, -344.0000000000002842 ) ) ;
#8259 = CIRCLE ( 'NONE', #45898, 2.000000000000001776 ) ;
#8260 = EDGE_CURVE ( 'NONE', #12550, #26328, #48195, .T. ) ;
#8261 = ORIENTED_EDGE ( 'NONE', *, *, #14011, .F. ) ;
#8262 = VECTOR ( 'NONE', #11617, 1000.000000000000000 ) ;
#8263 = CARTESIAN_POINT ( 'NONE',  ( -45.67084718096785423, -1.750000000000009548, -0.2068387089191121020 ) ) ;
#8264 = ORIENTED_EDGE ( 'NONE', *, *, #27156, .T. ) ;
#8265 = CARTESIAN_POINT ( 'NONE',  ( -206.6959734468149463, 0.000000000000000000, 165.0000000000000000 ) ) ;
#8266 = VERTEX_POINT ( 'NONE', #42139 ) ;
#8267 = CARTESIAN_POINT ( 'NONE',  ( 350.0000000000001137, 181.0000000000000284, 341.9999999999997726 ) ) ;
#8268 = CARTESIAN_POINT ( 'NONE',  ( 10.30302290646030627, 13.08520913973580058, -9.683996418299976483 ) ) ;
#8269 = VECTOR ( 'NONE', #50154, 1000.000000000000000 ) ;
#8270 = EDGE_CURVE ( 'NONE', #40331, #44892, #49793, .T. ) ;
#8271 = LINE ( 'NONE', #32632, #15020 ) ;
#8272 = CARTESIAN_POINT ( 'NONE',  ( -6.695973446814940111, -1.750000000000023315, -159.1817124430720298 ) ) ;
#8273 = EDGE_CURVE ( 'NONE', #42084, #26449, #22648, .T. ) ;
#8274 = ORIENTED_EDGE ( 'NONE', *, *, #33734, .F. ) ;
#8275 = EDGE_CURVE ( 'NONE', #17128, #5984, #10846, .T. ) ;
#8276 = EDGE_CURVE ( 'NONE', #45035, #269, #14449, .T. ) ;
#8277 = CYLINDRICAL_SURFACE ( 'NONE', #26978, 1.750000000000001554 ) ;
#8278 = CARTESIAN_POINT ( 'NONE',  ( 359.9999999999999432, -169.0000000000001705, 344.0000000000000000 ) ) ;
#8279 = ORIENTED_EDGE ( 'NONE', *, *, #17961, .F. ) ;
#8280 = LINE ( 'NONE', #15973, #8262 ) ;
#8281 = CARTESIAN_POINT ( 'NONE',  ( 181.0000000000000284, -9.999999999999953815, -99.00000000000014211 ) ) ;
#8282 = LINE ( 'NONE', #46721, #43416 ) ;
#8283 = FACE_OUTER_BOUND ( 'NONE', #47795, .T. ) ;
#8284 = EDGE_CURVE ( 'NONE', #38138, #21789, #2154, .T. ) ;
#8285 = ORIENTED_EDGE ( 'NONE', *, *, #5152, .F. ) ;
#8286 = ORIENTED_EDGE ( 'NONE', *, *, #35125, .T. ) ;
#8287 = CARTESIAN_POINT ( 'NONE',  ( 195.0540265531851105, 2.143131898507880377E-16, 165.0000000000000000 ) ) ;
#8288 = VERTEX_POINT ( 'NONE', #37822 ) ;
#8289 = CARTESIAN_POINT ( 'NONE',  ( -46.69597344681494633, -1.750000000000010658, -79.18171244307201562 ) ) ;
#8290 = CARTESIAN_POINT ( 'NONE',  ( 155.0540265531850537, -1.025126265847089435, 82.56828755692798438 ) ) ;
#8291 = PLANE ( 'NONE',  #28087 ) ;
#8292 =( BOUNDED_CURVE ( )  B_SPLINE_CURVE ( 3, ( #42673, #27033, #7548, #23185 ),
 .UNSPECIFIED., .F., .F. ) 
 B_SPLINE_CURVE_WITH_KNOTS ( ( 4, 4 ),
 ( 0.000000000000000000, 1.570796326794896558 ),
 .UNSPECIFIED. ) 
 CURVE ( )  GEOMETRIC_REPRESENTATION_ITEM ( )  RATIONAL_B_SPLINE_CURVE ( ( 1.000000000000000000, 0.8047378541243649375, 0.8047378541243649375, 1.000000000000000000 ) ) 
 REPRESENTATION_ITEM ( '' )  );
#8293 = VERTEX_POINT ( 'NONE', #45965 ) ;
#8294 = CARTESIAN_POINT ( 'NONE',  ( 1.011271242968688311, -0.7347315653655855927, 3.333333333333333481 ) ) ;
#8295 = EDGE_LOOP ( 'NONE', ( #17009, #9587, #45023, #474 ) ) ;
#8296 = VERTEX_POINT ( 'NONE', #7003 ) ;
#8297 = ADVANCED_FACE ( 'NONE', ( #45711 ), #29591, .T. ) ;
#8298 = CARTESIAN_POINT ( 'NONE',  ( 153.3040265531850537, -1.750000000000010214, -39.18171244307202983 ) ) ;
#8299 = VECTOR ( 'NONE', #40851, 1000.000000000000000 ) ;
#8300 = CARTESIAN_POINT ( 'NONE',  ( -1.249999999999999778, 0.000000000000000000, -10.00000000000000000 ) ) ;
#8301 = EDGE_CURVE ( 'NONE', #41260, #17360, #9836, .T. ) ;
#8302 = ORIENTED_EDGE ( 'NONE', *, *, #27093, .T. ) ;
#8303 = ADVANCED_FACE ( 'NONE', ( #25752 ), #48801, .T. ) ;
#8304 = VERTEX_POINT ( 'NONE', #18037 ) ;
#8305 =( REPRESENTATION_RELATIONSHIP ('NONE','NONE', #45699, #34661 ) REPRESENTATION_RELATIONSHIP_WITH_TRANSFORMATION ( #21548 )SHAPE_REPRESENTATION_RELATIONSHIP( ) );
#8306 = ORIENTED_EDGE ( 'NONE', *, *, #6971, .T. ) ;
#8307 = CARTESIAN_POINT ( 'NONE',  ( 210.0000000000000568, 0.000000000000000000, 120.8182875569279702 ) ) ;
#8308 = EDGE_CURVE ( 'NONE', #13701, #27139, #49040, .T. ) ;
#8309 = CYLINDRICAL_SURFACE ( 'NONE', #47774, 4.000000000000003553 ) ;
#8310 = PRODUCT_DEFINITION_CONTEXT ( 'detailed design', #6639, 'design' ) ;
#8311 = VERTEX_POINT ( 'NONE', #25489 ) ;
#8312 = CARTESIAN_POINT ( 'NONE',  ( -166.6959734468149463, -1.750000000000010214, -39.18171244307202983 ) ) ;
#8313 = AXIS2_PLACEMENT_3D ( 'NONE', #386, #31696, #7308 ) ;
#8314 = VERTEX_POINT ( 'NONE', #5987 ) ;
#8315 = ADVANCED_FACE ( 'NONE', ( #33459 ), #13927, .F. ) ;
#8316 = FACE_OUTER_BOUND ( 'NONE', #15406, .T. ) ;
#8317 = EDGE_LOOP ( 'NONE', ( #13925, #41557, #13560, #28285 ) ) ;
#8318 = CARTESIAN_POINT ( 'NONE',  ( 181.0000000000000000, -97.49999999999998579, -340.0000000000001137 ) ) ;
#8319 = CARTESIAN_POINT ( 'NONE',  ( -165.2900739183569954, 53.53801056904005407, -18.55102910462098365 ) ) ;
#8320 = FACE_OUTER_BOUND ( 'NONE', #3034, .T. ) ;
#8321 = CARTESIAN_POINT ( 'NONE',  ( -70.00000000000002842, 17.00000000000000000, -90.00000000000000000 ) ) ;
#8322 = CARTESIAN_POINT ( 'NONE',  ( -26.76431201374261093, 26.27596734087715902, 8.506357886886741326 ) ) ;
#8323 = ORIENTED_EDGE ( 'NONE', *, *, #34328, .F. ) ;
#8324 = VERTEX_POINT ( 'NONE', #21905 ) ;
#8325 = CARTESIAN_POINT ( 'NONE',  ( -47.72109971266203132, -1.750000000000009548, 1.843413822775065825 ) ) ;
#8326 = FACE_OUTER_BOUND ( 'NONE', #1770, .T. ) ;
#8327 = DIRECTION ( 'NONE',  ( -1.000000000000000000, 0.000000000000000000, 0.000000000000000000 ) ) ;
#8328 = ADVANCED_FACE ( 'NONE', ( #26760 ), #15976, .T. ) ;
#8329 = DIRECTION ( 'NONE',  ( 1.000000000000000000, 0.000000000000000000, 0.000000000000000000 ) ) ;
#8330 = ORIENTED_EDGE ( 'NONE', *, *, #35477, .T. ) ;
#8331 = LINE ( 'NONE', #23978, #3250 ) ;
#8332 = AXIS2_PLACEMENT_3D ( 'NONE', #26921, #42815, #10759 ) ;
#8333 = FACE_OUTER_BOUND ( 'NONE', #20543, .T. ) ;
#8334 = EDGE_CURVE ( 'NONE', #32609, #43847, #2487, .T. ) ;
#8335 = ORIENTED_EDGE ( 'NONE', *, *, #41760, .T. ) ;
#8336 = EDGE_CURVE ( 'NONE', #4263, #37483, #8282, .T. ) ;
#8337 = EDGE_CURVE ( 'NONE', #36323, #9039, #3657, .T. ) ;
#8338 = CARTESIAN_POINT ( 'NONE',  ( 1.249999999999999778, 0.000000000000000000, 10.00000000000000000 ) ) ;
#8339 = ADVANCED_FACE ( 'NONE', ( #50303 ), #19811, .F. ) ;
#8340 = CARTESIAN_POINT ( 'NONE',  ( -69.99999999999909051, 17.00000000000000000, -24.99999999999999289 ) ) ;
#8341 = ADVANCED_FACE ( 'NONE', ( #11355 ), #7782, .T. ) ;
#8342 = EDGE_LOOP ( 'NONE', ( #24557, #36009, #22961, #6138 ) ) ;
#8343 = VECTOR ( 'NONE', #37064, 1000.000000000000000 ) ;
#8344 = ORIENTED_EDGE ( 'NONE', *, *, #7544, .T. ) ;
#8345 = CYLINDRICAL_SURFACE ( 'NONE', #1335, 1.750000000000001554 ) ;
#8346 = EDGE_CURVE ( 'NONE', #16242, #27082, #3392, .T. ) ;
#8347 = CARTESIAN_POINT ( 'NONE',  ( 1.011271242968694084, -0.7347315653655782652, 10.00000000000000000 ) ) ;
#8348 =( BOUNDED_CURVE ( )  B_SPLINE_CURVE ( 3, ( #8940, #6348, #21237, #9692 ),
 .UNSPECIFIED., .F., .F. ) 
 B_SPLINE_CURVE_WITH_KNOTS ( ( 4, 4 ),
 ( 1.570796326794896558, 3.141592653589793116 ),
 .UNSPECIFIED. ) 
 CURVE ( )  GEOMETRIC_REPRESENTATION_ITEM ( )  RATIONAL_B_SPLINE_CURVE ( ( 1.000000000000000000, 0.8047378541243649375, 0.8047378541243649375, 1.000000000000000000 ) ) 
 REPRESENTATION_ITEM ( '' )  );
#8349 = B_SPLINE_CURVE_WITH_KNOTS ( 'NONE', 3,
 ( #38961, #213, #38458, #49925 ),
 .UNSPECIFIED., .F., .F.,
 ( 4, 4 ),
 ( 0.0006669682284780766154, 0.0007799402130919628204 ),
 .UNSPECIFIED. ) ;
#8350 = ORIENTED_EDGE ( 'NONE', *, *, #43073, .T. ) ;
#8351 = ORIENTED_EDGE ( 'NONE', *, *, #4439, .F. ) ;
#8352 = DIRECTION ( 'NONE',  ( 0.000000000000000000, 8.673617379884027583E-15, 1.000000000000000000 ) ) ;
#8353 = LINE ( 'NONE', #31713, #21496 ) ;
#8354 = CARTESIAN_POINT ( 'NONE',  ( -7.576114424932982594, 33.14742743729794938, 7.906207997025717304 ) ) ;
#8355 = CARTESIAN_POINT ( 'NONE',  ( 0.1287570809895660084, -0.3962735484563127408, 10.00000000000000000 ) ) ;
#8356 = FACE_OUTER_BOUND ( 'NONE', #34911, .T. ) ;
#8357 = ORIENTED_EDGE ( 'NONE', *, *, #4279, .F. ) ;
#8358 = ORIENTED_EDGE ( 'NONE', *, *, #46516, .F. ) ;
#8359 = ORIENTED_EDGE ( 'NONE', *, *, #28826, .F. ) ;
#8360 =( BOUNDED_CURVE ( )  B_SPLINE_CURVE ( 3, ( #24421, #4893, #20556, #1062 ),
 .UNSPECIFIED., .F., .F. ) 
 B_SPLINE_CURVE_WITH_KNOTS ( ( 4, 4 ),
 ( 3.141592653589793116, 4.712388980384689674 ),
 .UNSPECIFIED. ) 
 CURVE ( )  GEOMETRIC_REPRESENTATION_ITEM ( )  RATIONAL_B_SPLINE_CURVE ( ( 1.000000000000000000, 0.8047378541243649375, 0.8047378541243649375, 1.000000000000000000 ) ) 
 REPRESENTATION_ITEM ( '' )  );
#8361 = CARTESIAN_POINT ( 'NONE',  ( 85.00000000000090949, 17.00000000000000000, -24.99999999999999289 ) ) ;
#8362 = ORIENTED_EDGE ( 'NONE', *, *, #29139, .T. ) ;
#8363 = EDGE_CURVE ( 'NONE', #41009, #38609, #3833, .T. ) ;
#8364 = CARTESIAN_POINT ( 'NONE',  ( 72.27890028733797578, 1.750000000000010436, -120.2068387089191219 ) ) ;
#8365 = ORIENTED_EDGE ( 'NONE', *, *, #7332, .T. ) ;
#8366 = ORIENTED_EDGE ( 'NONE', *, *, #10815, .T. ) ;
#8367 = CARTESIAN_POINT ( 'NONE',  ( 1.810969182959398571, -3.505385724216245169, 6.494306115488114983 ) ) ;
#8368 =( LENGTH_UNIT ( ) NAMED_UNIT ( * ) SI_UNIT ( .MILLI., .METRE. ) );
#8369 = AXIS2_PLACEMENT_3D ( 'NONE', #6214, #5439, #21093 ) ;
#8370 = CARTESIAN_POINT ( 'NONE',  ( 210.0000000000000568, 0.000000000000000000, 80.81828755692798438 ) ) ;
#8371 = ORIENTED_EDGE ( 'NONE', *, *, #20884, .F. ) ;
#8372 = PRODUCT_DEFINITION ( 'UNKNOWN', '', #22553, #16005 ) ;
#8373 = EDGE_LOOP ( 'NONE', ( #41061, #28074, #33523, #19635 ) ) ;
#8374 = CARTESIAN_POINT ( 'NONE',  ( 17.23491422248386584, -0.5912720620000816441, 8.727788335465566760 ) ) ;
#8375 = CARTESIAN_POINT ( 'NONE',  ( 34.32915281903212446, 1.750000000000009548, -158.1565861772249377 ) ) ;
#8376 = ORIENTED_EDGE ( 'NONE', *, *, #14890, .F. ) ;
#8377 = PLANE ( 'NONE',  #968 ) ;
#8378 = CARTESIAN_POINT ( 'NONE',  ( 151.5540265531850537, 1.025126265847089435, 122.5682875569280128 ) ) ;
#8379 = DIRECTION ( 'NONE',  ( 1.132880637372608740E-16, 4.718402560806925739E-50, 1.000000000000000000 ) ) ;
#8380 = CARTESIAN_POINT ( 'NONE',  ( 3.630679331413954714, 37.33064849398144958, -8.600750091277037157 ) ) ;
#8381 = ORIENTED_EDGE ( 'NONE', *, *, #7158, .F. ) ;
#8382 = EDGE_CURVE ( 'NONE', #2039, #16293, #33963, .T. ) ;
#8383 = CARTESIAN_POINT ( 'NONE',  ( 164.9999999999999716, -164.9999999999999432, -344.0000000000001137 ) ) ;
#8384 = LINE ( 'NONE', #43261, #46105 ) ;
#8385 = CARTESIAN_POINT ( 'NONE',  ( -4.412346620047150836, -9.007664521157030535, 9.516222621873129839 ) ) ;
#8386 = DIRECTION ( 'NONE',  ( 4.755310728521421461E-16, 0.000000000000000000, 1.000000000000000000 ) ) ;
#8387 = LINE ( 'NONE', #9134, #44164 ) ;
#8388 = VECTOR ( 'NONE', #33968, 1000.000000000000000 ) ;
#8389 = CARTESIAN_POINT ( 'NONE',  ( -0.6126904405382037622, -1.085824959725731231, 9.981352469109934233 ) ) ;
#8390 = VERTEX_POINT ( 'NONE', #22900 ) ;
#8391 = DIRECTION ( 'NONE',  ( -1.000000000000000000, 0.000000000000000000, -0.000000000000000000 ) ) ;
#8392 = EDGE_CURVE ( 'NONE', #48110, #9081, #39090, .T. ) ;
#8393 = EDGE_CURVE ( 'NONE', #34818, #35344, #11874, .T. ) ;
#8394 = CARTESIAN_POINT ( 'NONE',  ( -86.69597344681494633, 1.750000000000009992, 160.8182875569279702 ) ) ;
#8395 = VECTOR ( 'NONE', #40986, 1000.000000000000114 ) ;
#8396 = ORIENTED_EDGE ( 'NONE', *, *, #46363, .T. ) ;
#8397 = CARTESIAN_POINT ( 'NONE',  ( -175.0000000000000000, 15.00000000000000000, 122.5000000000000142 ) ) ;
#8398 = DIRECTION ( 'NONE',  ( 0.000000000000000000, 0.000000000000000000, -1.000000000000000000 ) ) ;
#8399 = CARTESIAN_POINT ( 'NONE',  ( -64.99999999999940314, 17.00000000000000000, -30.00000000000000000 ) ) ;
#8400 = AXIS2_PLACEMENT_3D ( 'NONE', #50720, #35396, #28186 ) ;
#8401 = ADVANCED_FACE ( 'NONE', ( #11108 ), #27532, .F. ) ;
#8402 = EDGE_LOOP ( 'NONE', ( #48506, #22576, #41484 ) ) ;
#8403 = CARTESIAN_POINT ( 'NONE',  ( -126.6959734468149321, -1.749999999999997113, -39.18171244307202983 ) ) ;
#8404 = ORIENTED_EDGE ( 'NONE', *, *, #23196, .T. ) ;
#8405 = ORIENTED_EDGE ( 'NONE', *, *, #2412, .F. ) ;
#8406 = DIRECTION ( 'NONE',  ( -1.000000000000000000, -0.000000000000000000, -0.000000000000000000 ) ) ;
#8407 = AXIS2_PLACEMENT_3D ( 'NONE', #16644, #35162, #43084 ) ;
#8408 = EDGE_CURVE ( 'NONE', #5803, #24755, #336, .T. ) ;
#8409 = CARTESIAN_POINT ( 'NONE',  ( 73.30402655318508209, -1.750000000000009992, -159.1817124430720298 ) ) ;
#8410 = EDGE_CURVE ( 'NONE', #37272, #36401, #12129, .T. ) ;
#8411 = EDGE_LOOP ( 'NONE', ( #32390, #1352, #5238, #6441, #29699, #9781 ) ) ;
#8412 = VECTOR ( 'NONE', #44971, 1000.000000000000000 ) ;
#8413 = CARTESIAN_POINT ( 'NONE',  ( 168.9999999999999716, 165.0000000000000000, -358.0000000000001705 ) ) ;
#8414 = DIRECTION ( 'NONE',  ( 1.000000000000000000, 0.000000000000000000, -1.586032892321652482E-16 ) ) ;
#8415 = ORIENTED_EDGE ( 'NONE', *, *, #11779, .F. ) ;
#8416 = EDGE_CURVE ( 'NONE', #12918, #28229, #15215, .T. ) ;
#8417 = CARTESIAN_POINT ( 'NONE',  ( 357.9999999999999432, -181.0000000000001421, -349.9999999999999432 ) ) ;
#8418 = ORIENTED_EDGE ( 'NONE', *, *, #45999, .F. ) ;
#8419 = PLANE ( 'NONE',  #18444 ) ;
#8420 = DIRECTION ( 'NONE',  ( 1.333906992743555050E-23, -1.000000000000000000, 0.000000000000000000 ) ) ;
#8421 = LINE ( 'NONE', #7920, #4579 ) ;
#8422 = ORIENTED_EDGE ( 'NONE', *, *, #1983, .T. ) ;
#8423 = FACE_OUTER_BOUND ( 'NONE', #49059, .T. ) ;
#8424 = CARTESIAN_POINT ( 'NONE',  ( 164.9999999999999716, 175.0000000000000284, -344.0000000000001137 ) ) ;
#8425 = ORIENTED_EDGE ( 'NONE', *, *, #42446, .T. ) ;
#8426 = ORIENTED_EDGE ( 'NONE', *, *, #9952, .T. ) ;
#8427 = EDGE_LOOP ( 'NONE', ( #44341, #48561, #17065, #32635, #35333 ) ) ;
#8428 = CARTESIAN_POINT ( 'NONE',  ( 340.0000000000000568, 167.0000000000000000, 343.9999999999997726 ) ) ;
#8429 = CIRCLE ( 'NONE', #32195, 4.000000000000003553 ) ;
#8430 = DIRECTION ( 'NONE',  ( 0.000000000000000000, -2.537652627714643577E-15, -1.000000000000000000 ) ) ;
#8431 = ORIENTED_EDGE ( 'NONE', *, *, #24961, .F. ) ;
#8432 = CARTESIAN_POINT ( 'NONE',  ( 210.0000000000000568, 0.000000000000000000, 40.81828755692798438 ) ) ;
#8433 = DIRECTION ( 'NONE',  ( 0.000000000000000000, 0.000000000000000000, 1.000000000000000000 ) ) ;
#8434 = CARTESIAN_POINT ( 'NONE',  ( -29.39982726364978660, -16.78152490921149109, 8.356839323120299312 ) ) ;
#8435 = CARTESIAN_POINT ( 'NONE',  ( 355.9999999999999432, -183.0000000000000000, 357.9999999999998295 ) ) ;
#8436 = DIRECTION ( 'NONE',  ( -1.000000000000000000, 0.000000000000000000, 0.000000000000000000 ) ) ;
#8437 = CARTESIAN_POINT ( 'NONE',  ( 4.763548243873389154, -16.57409059453848599, 8.727788335465566760 ) ) ;
#8438 = SHAPE_REPRESENTATION ( 'tire 1', ( #45486 ), #38984 ) ;
#8439 =( GEOMETRIC_REPRESENTATION_CONTEXT ( 3 ) GLOBAL_UNCERTAINTY_ASSIGNED_CONTEXT ( ( #36415 ) ) GLOBAL_UNIT_ASSIGNED_CONTEXT ( ( #26535, #13963, #21932 ) ) REPRESENTATION_CONTEXT ( 'NONE', 'WORKASPACE' ) );
#8440 = CARTESIAN_POINT ( 'NONE',  ( -10.49999999999999467, -46.01315789473684248, 5.916985404131814619 ) ) ;
#8441 = LINE ( 'NONE', #35902, #38224 ) ;
#8442 = VECTOR ( 'NONE', #11219, 1000.000000000000000 ) ;
#8443 = CARTESIAN_POINT ( 'NONE',  ( 210.0000000000000568, 2.143131898507881856E-16, -80.93171244307202983 ) ) ;
#8444 = DIRECTION ( 'NONE',  ( -0.000000000000000000, -1.000000000000000000, -0.000000000000000000 ) ) ;
#8445 = CARTESIAN_POINT ( 'NONE',  ( -1.738880908827836524, -0.9455076376091113843, 9.897807938190497978 ) ) ;
#8446 = ADVANCED_FACE ( 'NONE', ( #42646 ), #37944, .T. ) ;
#8447 = CARTESIAN_POINT ( 'NONE',  ( 355.9999999999999432, -165.0000000000001137, -106.0000000000001990 ) ) ;
#8448 = DIRECTION ( 'NONE',  ( 3.469446951953616950E-15, 0.000000000000000000, -1.000000000000000000 ) ) ;
#8449 = DIRECTION ( 'NONE',  ( 3.172065745548403743E-16, 1.000000000000000000, 0.000000000000000000 ) ) ;
#8450 = ORIENTED_EDGE ( 'NONE', *, *, #39309, .T. ) ;
#8451 = DIRECTION ( 'NONE',  ( -1.156482317317871478E-16, 1.000000000000000000, -0.000000000000000000 ) ) ;
#8452 = DIRECTION ( 'NONE',  ( -1.000000000000000000, -0.000000000000000000, -0.000000000000000000 ) ) ;
#8453 = LINE ( 'NONE', #28201, #34461 ) ;
#8454 = ORIENTED_EDGE ( 'NONE', *, *, #12863, .T. ) ;
#8455 = DIRECTION ( 'NONE',  ( -0.000000000000000000, -0.000000000000000000, 1.000000000000000000 ) ) ;
#8456 = ADVANCED_FACE ( 'NONE', ( #1588 ), #17235, .T. ) ;
#8457 = EDGE_CURVE ( 'NONE', #7083, #49071, #9526, .T. ) ;
#8458 = VECTOR ( 'NONE', #2296, 1000.000000000000000 ) ;
#8459 = LINE ( 'NONE', #48404, #28649 ) ;
#8460 = EDGE_LOOP ( 'NONE', ( #47594, #1711, #45817, #14173 ) ) ;
#8461 = CARTESIAN_POINT ( 'NONE',  ( -31.44259251615275019, -38.95901822126145220, -9.367992836599951190 ) ) ;
#8462 = LINE ( 'NONE', #23857, #8472 ) ;
#8463 = DIRECTION ( 'NONE',  ( 0.000000000000000000, 0.000000000000000000, 1.000000000000000000 ) ) ;
#8464 = VERTEX_POINT ( 'NONE', #31890 ) ;
#8465 = CARTESIAN_POINT ( 'NONE',  ( -88.44597344681497475, 0.000000000000000000, 165.0000000000000000 ) ) ;
#8466 = EDGE_LOOP ( 'NONE', ( #37845, #32161, #6115, #21510 ) ) ;
#8467 = EDGE_CURVE ( 'NONE', #37272, #21250, #8535, .T. ) ;
#8468 = EDGE_CURVE ( 'NONE', #2419, #41044, #1084, .T. ) ;
#8469 = VERTEX_POINT ( 'NONE', #32900 ) ;
#8470 = DIRECTION ( 'NONE',  ( 0.000000000000000000, 0.000000000000000000, 1.000000000000000000 ) ) ;
#8471 = CARTESIAN_POINT ( 'NONE',  ( -4.945973446814917018, -1.025126265847097207, 162.5682875569279986 ) ) ;
#8472 = VECTOR ( 'NONE', #39516, 1000.000000000000000 ) ;
#8473 = EDGE_LOOP ( 'NONE', ( #2104, #35133, #16095, #20960, #8205 ) ) ;
#8474 = DIRECTION ( 'NONE',  ( -0.000000000000000000, -1.000000000000000000, -0.000000000000000000 ) ) ;
#8475 = LINE ( 'NONE', #8733, #11970 ) ;
#8476 = EDGE_CURVE ( 'NONE', #43115, #13598, #44159, .T. ) ;
#8477 = VECTOR ( 'NONE', #25850, 1000.000000000000000 ) ;
#8478 = FACE_OUTER_BOUND ( 'NONE', #15897, .T. ) ;
#8479 = CARTESIAN_POINT ( 'NONE',  ( -1.011271242968683426, -0.7347315653655928092, -10.00000000000000000 ) ) ;
#8480 = ORIENTED_EDGE ( 'NONE', *, *, #46007, .T. ) ;
#8481 = VECTOR ( 'NONE', #46139, 1000.000000000000000 ) ;
#8482 = CARTESIAN_POINT ( 'NONE',  ( -85.67084718096784002, -1.750000000000009548, -118.1565861772249519 ) ) ;
#8483 = VERTEX_POINT ( 'NONE', #47485 ) ;
#8484 = CIRCLE ( 'NONE', #2708, 1.750000000000001554 ) ;
#8485 = PLANE ( 'NONE',  #14444 ) ;
#8486 = DIRECTION ( 'NONE',  ( 0.000000000000000000, 7.004339610132985974E-48, 1.000000000000000000 ) ) ;
#8487 = ORIENTED_EDGE ( 'NONE', *, *, #37699, .T. ) ;
#8488 = CARTESIAN_POINT ( 'NONE',  ( 135.0000000000012790, 17.00000000000000000, 5.000000000000004441 ) ) ;
#8489 = CYLINDRICAL_SURFACE ( 'NONE', #25125, 2.000000000000001776 ) ;
#8490 = B_SPLINE_SURFACE_WITH_KNOTS ( 'NONE', 3, 3, ( 
 ( #5332, #20991, #17384, #36672 ),
 ( #17137, #32798, #48387, #28934 ),
 ( #25340, #14026, #49647, #29950 ),
 ( #10691, #45806, #15052, #26605 ) ),
 .UNSPECIFIED., .F., .F., .F.,
 ( 4, 4 ),
 ( 4, 4 ),
 ( 0.000000000000000000, 1.000000000000000000 ),
 ( 0.000000000000000000, 1.000000000000000000 ),
 .UNSPECIFIED. ) ;
#8491 = ORIENTED_EDGE ( 'NONE', *, *, #3088, .T. ) ;
#8492 = CARTESIAN_POINT ( 'NONE',  ( -14.99999999999845812, 17.00000000000000000, 35.00000000000000000 ) ) ;
#8493 = CARTESIAN_POINT ( 'NONE',  ( -32.65539107884902847, -7.204654279305827913, -8.917361510505369182 ) ) ;
#8494 = DIRECTION ( 'NONE',  ( 0.000000000000000000, 0.000000000000000000, -1.000000000000000000 ) ) ;
#8495 =( BOUNDED_CURVE ( )  B_SPLINE_CURVE ( 3, ( #10371, #49309, #14193, #26021 ),
 .UNSPECIFIED., .F., .F. ) 
 B_SPLINE_CURVE_WITH_KNOTS ( ( 4, 4 ),
 ( 3.141592653589793116, 4.712388980384689674 ),
 .UNSPECIFIED. ) 
 CURVE ( )  GEOMETRIC_REPRESENTATION_ITEM ( )  RATIONAL_B_SPLINE_CURVE ( ( 1.000000000000000000, 0.8047378541243649375, 0.8047378541243649375, 1.000000000000000000 ) ) 
 REPRESENTATION_ITEM ( '' )  );
#8496 = LINE ( 'NONE', #32349, #36249 ) ;
#8497 = AXIS2_PLACEMENT_3D ( 'NONE', #30640, #42671, #27800 ) ;
#8498 = ORIENTED_EDGE ( 'NONE', *, *, #34484, .F. ) ;
#8499 = CARTESIAN_POINT ( 'NONE',  ( 349.9999999999999432, -166.9999999999999432, 343.9999999999997726 ) ) ;
#8500 = DIRECTION ( 'NONE',  ( 1.368455531567204171E-48, -1.000000000000000000, -2.265761274745217480E-16 ) ) ;
#8501 =( BOUNDED_CURVE ( )  B_SPLINE_CURVE ( 3, ( #3887, #34202, #49776, #6983 ),
 .UNSPECIFIED., .F., .F. ) 
 B_SPLINE_CURVE_WITH_KNOTS ( ( 4, 4 ),
 ( 1.570796326794896558, 3.141592653589793116 ),
 .UNSPECIFIED. ) 
 CURVE ( )  GEOMETRIC_REPRESENTATION_ITEM ( )  RATIONAL_B_SPLINE_CURVE ( ( 1.000000000000000000, 0.8047378541243649375, 0.8047378541243649375, 1.000000000000000000 ) ) 
 REPRESENTATION_ITEM ( '' )  );
#8502 = CARTESIAN_POINT ( 'NONE',  ( 29.18392875402930997, 17.44843138996603216, 7.906207997025717304 ) ) ;
#8503 = ORIENTED_EDGE ( 'NONE', *, *, #31244, .T. ) ;
#8504 = EDGE_CURVE ( 'NONE', #12400, #26840, #1646, .T. ) ;
#8505 = EDGE_LOOP ( 'NONE', ( #4303, #28064, #30740, #1772, #41018, #49478, #50576, #36324, #14338, #7286, #5257, #21628 ) ) ;
#8506 = APPLICATION_PROTOCOL_DEFINITION ( 'draft international standard', 'automotive_design', 1998, #23656 ) ;
#8507 = CYLINDRICAL_SURFACE ( 'NONE', #5242, 2.000000000000001776 ) ;
#8508 = CARTESIAN_POINT ( 'NONE',  ( 193.3040265531851105, -1.750000000000010658, -119.1817124430720440 ) ) ;
#8509 = CARTESIAN_POINT ( 'NONE',  ( -36.08557433729205144, 35.58569447144795816, 7.455576670931136185 ) ) ;
#8510 = AXIS2_PLACEMENT_3D ( 'NONE', #18220, #7199, #38007 ) ;
#8511 = CARTESIAN_POINT ( 'NONE',  ( -1.011271242968693862, 0.7347315653655780432, 3.333333333333333481 ) ) ;
#8512 = ORIENTED_EDGE ( 'NONE', *, *, #21185, .T. ) ;
#8513 = LINE ( 'NONE', #32616, #976 ) ;
#8514 = CIRCLE ( 'NONE', #15903, 0.5000000000000004441 ) ;
#8515 =( BOUNDED_CURVE ( )  B_SPLINE_CURVE ( 3, ( #49278, #38561, #41381, #41881 ),
 .UNSPECIFIED., .F., .F. ) 
 B_SPLINE_CURVE_WITH_KNOTS ( ( 4, 4 ),
 ( 1.570796326794896558, 3.141592653589793116 ),
 .UNSPECIFIED. ) 
 CURVE ( )  GEOMETRIC_REPRESENTATION_ITEM ( )  RATIONAL_B_SPLINE_CURVE ( ( 1.000000000000000000, 0.8047378541243649375, 0.8047378541243649375, 1.000000000000000000 ) ) 
 REPRESENTATION_ITEM ( '' )  );
#8516 = FACE_OUTER_BOUND ( 'NONE', #34229, .T. ) ;
#8517 = DIRECTION ( 'NONE',  ( -0.000000000000000000, -1.000000000000000000, -0.000000000000000000 ) ) ;
#8518 = CARTESIAN_POINT ( 'NONE',  ( -6.695973446814940111, 0.000000000000000000, 165.0000000000000000 ) ) ;
#8519 = ORIENTED_EDGE ( 'NONE', *, *, #6765, .T. ) ;
#8520 = PLANE ( 'NONE',  #47681 ) ;
#8521 = VERTEX_POINT ( 'NONE', #24689 ) ;
#8522 = DIRECTION ( 'NONE',  ( -1.586032880504786307E-16, 1.654361225106055350E-24, -1.000000000000000000 ) ) ;
#8523 = VERTEX_POINT ( 'NONE', #20322 ) ;
#8524 = LINE ( 'NONE', #27516, #4953 ) ;
#8525 = FACE_OUTER_BOUND ( 'NONE', #48560, .T. ) ;
#8526 = CARTESIAN_POINT ( 'NONE',  ( 210.0000000000000568, 0.000000000000000000, -119.1817124430720440 ) ) ;
#8527 = FACE_OUTER_BOUND ( 'NONE', #12146, .T. ) ;
#8528 = ORIENTED_EDGE ( 'NONE', *, *, #20326, .T. ) ;
#8529 = VECTOR ( 'NONE', #27631, 1000.000000000000000 ) ;
#8530 = FACE_OUTER_BOUND ( 'NONE', #16618, .T. ) ;
#8531 = LINE ( 'NONE', #4678, #46670 ) ;
#8532 = ORIENTED_EDGE ( 'NONE', *, *, #16861, .T. ) ;
#8533 = CARTESIAN_POINT ( 'NONE',  ( -69.99999999999847944, 17.00000000000000000, 60.00000000000000000 ) ) ;
#8534 = LINE ( 'NONE', #39847, #16691 ) ;
#8535 = LINE ( 'NONE', #44406, #13093 ) ;
#8536 = CARTESIAN_POINT ( 'NONE',  ( -5.000000000000000000, -165.1999999999999602, -340.2000000000001592 ) ) ;
#8537 = ADVANCED_FACE ( 'NONE', ( #16724 ), #20820, .T. ) ;
#8538 = ORIENTED_EDGE ( 'NONE', *, *, #37613, .F. ) ;
#8539 = ORIENTED_EDGE ( 'NONE', *, *, #1410, .F. ) ;
#8540 = CYLINDRICAL_SURFACE ( 'NONE', #11181, 1.750000000000015543 ) ;
#8541 = ORIENTED_EDGE ( 'NONE', *, *, #8691, .T. ) ;
#8542 = DIRECTION ( 'NONE',  ( -0.000000000000000000, -1.000000000000000000, -0.000000000000000000 ) ) ;
#8543 = CARTESIAN_POINT ( 'NONE',  ( -5.000000000000000000, -165.1999999999999602, -359.8000000000002387 ) ) ;
#8544 = AXIS2_PLACEMENT_3D ( 'NONE', #13061, #28478, #48423 ) ;
#8545 = VECTOR ( 'NONE', #39467, 1000.000000000000000 ) ;
#8546 = CARTESIAN_POINT ( 'NONE',  ( -14.99999999999937472, 16.00000000000000000, -54.99999999999999289 ) ) ;
#8547 = ORIENTED_EDGE ( 'NONE', *, *, #24632, .T. ) ;
#8548 = DIRECTION ( 'NONE',  ( 0.000000000000000000, 0.000000000000000000, -1.000000000000000000 ) ) ;
#8549 = VECTOR ( 'NONE', #43646, 1000.000000000000000 ) ;
#8550 = B_SPLINE_CURVE_WITH_KNOTS ( 'NONE', 3,
 ( #45515, #40505, #34259, #25107 ),
 .UNSPECIFIED., .F., .F.,
 ( 4, 4 ),
 ( 1.734723475976807094E-18, 2.804146970186756761E-05 ),
 .UNSPECIFIED. ) ;
#8551 = VECTOR ( 'NONE', #11805, 1000.000000000000000 ) ;
#8552 = EDGE_CURVE ( 'NONE', #28177, #7812, #35997, .T. ) ;
#8553 = DIRECTION ( 'NONE',  ( 1.000000000000000000, 0.000000000000000000, -0.000000000000000000 ) ) ;
#8554 = DIRECTION ( 'NONE',  ( -1.000000000000000000, 0.000000000000000000, 0.000000000000000000 ) ) ;
#8555 = ORIENTED_EDGE ( 'NONE', *, *, #46158, .F. ) ;
#8556 = ORIENTED_EDGE ( 'NONE', *, *, #8308, .F. ) ;
#8557 = ORIENTED_EDGE ( 'NONE', *, *, #35287, .F. ) ;
#8558 = CARTESIAN_POINT ( 'NONE',  ( -1.249999999999999778, 0.000000000000000000, 10.00000000000000000 ) ) ;
#8559 = CARTESIAN_POINT ( 'NONE',  ( -0.5000000000000000000, -0.5000000000000000000, 1000.000000000000000 ) ) ;
#8560 = CARTESIAN_POINT ( 'NONE',  ( -7.721099712662037540, -1.750000000000023537, 81.84341382277507648 ) ) ;
#8561 = ORIENTED_EDGE ( 'NONE', *, *, #21222, .T. ) ;
#8562 = CARTESIAN_POINT ( 'NONE',  ( 339.9999999999998863, -168.9999999999999432, 341.9999999999997726 ) ) ;
#8563 = ORIENTED_EDGE ( 'NONE', *, *, #41926, .T. ) ;
#8564 = CARTESIAN_POINT ( 'NONE',  ( 240.0000000000000000, -164.9999999999999716, 474.9999999999998863 ) ) ;
#8565 = ORIENTED_EDGE ( 'NONE', *, *, #26877, .F. ) ;
#8566 = DIRECTION ( 'NONE',  ( -0.000000000000000000, -0.000000000000000000, 1.000000000000000000 ) ) ;
#8567 = CARTESIAN_POINT ( 'NONE',  ( -1.011271242968683426, -0.7347315653655928092, 10.00000000000000000 ) ) ;
#8568 = FACE_OUTER_BOUND ( 'NONE', #33740, .T. ) ;
#8569 = VECTOR ( 'NONE', #10192, 1000.000000000000000 ) ;
#8570 = CARTESIAN_POINT ( 'NONE',  ( -5.000000000000000000, 175.0000000000000284, -346.2500000000002274 ) ) ;
#8571 = DIRECTION ( 'NONE',  ( 1.000000000000000000, 0.000000000000000000, -0.000000000000000000 ) ) ;
#8572 = CARTESIAN_POINT ( 'NONE',  ( -88.44597344681497475, 0.000000000000000000, 165.0000000000000000 ) ) ;
#8573 = ORIENTED_EDGE ( 'NONE', *, *, #31944, .T. ) ;
#8574 = EDGE_LOOP ( 'NONE', ( #24485, #28154, #49555, #41710, #41523, #20240 ) ) ;
#8575 = DIRECTION ( 'NONE',  ( -1.000000000000000000, 3.172065784643302499E-16, 1.942330104924128867E-32 ) ) ;
#8576 = CARTESIAN_POINT ( 'NONE',  ( -48.44597344681496054, -1.025126265847089657, 79.06828755692797017 ) ) ;
#8577 = CARTESIAN_POINT ( 'NONE',  ( 210.0000000000000568, 0.000000000000000000, 160.8182875569279702 ) ) ;
#8578 = DIRECTION ( 'NONE',  ( 0.000000000000000000, 0.000000000000000000, 1.000000000000000000 ) ) ;
#8579 = VECTOR ( 'NONE', #44415, 1000.000000000000000 ) ;
#8580 = CARTESIAN_POINT ( 'NONE',  ( 360.0000000000000000, 166.6568542494925964, -341.6568542494925396 ) ) ;
#8581 = VERTEX_POINT ( 'NONE', #24189 ) ;
#8582 = DIRECTION ( 'NONE',  ( 6.765175596986471882E-16, -0.9749645535258953943, -0.2223603367690637489 ) ) ;
#8583 = DIRECTION ( 'NONE',  ( 1.000000000000000000, 0.000000000000000000, 0.000000000000000000 ) ) ;
#8584 = CIRCLE ( 'NONE', #2809, 1.749999999999987566 ) ;
#8585 = ORIENTED_EDGE ( 'NONE', *, *, #42131, .T. ) ;
#8586 = EDGE_CURVE ( 'NONE', #26976, #25838, #9043, .T. ) ;
#8587 = CARTESIAN_POINT ( 'NONE',  ( 0.000000000000000000, 165.0000000000000000, -344.0000000000001705 ) ) ;
#8588 = CARTESIAN_POINT ( 'NONE',  ( 3.239037401336969602, 50.00000000000000711, -8.917361510505369182 ) ) ;
#8589 = CARTESIAN_POINT ( 'NONE',  ( 194.9999999999999432, 173.0000000000000000, 352.0000000000000000 ) ) ;
#8590 = DIRECTION ( 'NONE',  ( 1.000000000000000000, 0.000000000000000000, 0.000000000000000000 ) ) ;
#8591 = ADVANCED_FACE ( 'NONE', ( #16484 ), #36503, .T. ) ;
#8592 = ORIENTED_EDGE ( 'NONE', *, *, #12028, .T. ) ;
#8593 = EDGE_LOOP ( 'NONE', ( #33643, #26143, #11702, #30168 ) ) ;
#8594 = CARTESIAN_POINT ( 'NONE',  ( 195.0540265531851105, -1.025126265847089435, -77.43171244307200141 ) ) ;
#8595 = EDGE_CURVE ( 'NONE', #4376, #47214, #30524, .T. ) ;
#8596 = DIRECTION ( 'NONE',  ( -1.586032892321652236E-16, -1.000000000000000000, -6.853681917100419162E-49 ) ) ;
#8597 = EDGE_CURVE ( 'NONE', #9976, #18218, #18870, .T. ) ;
#8598 = VECTOR ( 'NONE', #38869, 1000.000000000000000 ) ;
#8599 = ORIENTED_EDGE ( 'NONE', *, *, #45662, .F. ) ;
#8600 = ORIENTED_EDGE ( 'NONE', *, *, #25887, .F. ) ;
#8601 = CARTESIAN_POINT ( 'NONE',  ( -9.999999999999994671, 2.168404344971008375E-16, 8.340239149799208107 ) ) ;
#8602 = DIRECTION ( 'NONE',  ( -0.000000000000000000, -0.000000000000000000, -1.000000000000000000 ) ) ;
#8603 = CARTESIAN_POINT ( 'NONE',  ( 29.39982726364966581, 16.78152490921169360, 8.356839323120299312 ) ) ;
#8604 = DIRECTION ( 'NONE',  ( 0.000000000000000000, -1.000000000000000000, 0.000000000000000000 ) ) ;
#8605 = ORIENTED_EDGE ( 'NONE', *, *, #19335, .F. ) ;
#8606 = VECTOR ( 'NONE', #30336, 1000.000000000000000 ) ;
#8607 = ORIENTED_EDGE ( 'NONE', *, *, #376, .T. ) ;
#8608 = ORIENTED_EDGE ( 'NONE', *, *, #44516, .T. ) ;
#8609 = CARTESIAN_POINT ( 'NONE',  ( -16.99749102614300966, 1.320765928724422222, 8.953103998512858652 ) ) ;
#8610 = VERTEX_POINT ( 'NONE', #8789 ) ;
#8611 = CARTESIAN_POINT ( 'NONE',  ( -126.6959734468149321, 1.749999999999996891, 0.8182875569279768335 ) ) ;
#8612 = AXIS2_PLACEMENT_3D ( 'NONE', #16871, #48114, #36901 ) ;
#8613 = ORIENTED_EDGE ( 'NONE', *, *, #16112, .F. ) ;
#8614 = ORIENTED_EDGE ( 'NONE', *, *, #46158, .T. ) ;
#8615 = CARTESIAN_POINT ( 'NONE',  ( -4.999999999999948486, -214.9999999999999716, -230.2499999999999716 ) ) ;
#8616 = CARTESIAN_POINT ( 'NONE',  ( 45.42829307628542779, 21.98948915213303579, 8.356839323120299312 ) ) ;
#8617 = ORIENTED_EDGE ( 'NONE', *, *, #4192, .T. ) ;
#8618 = EDGE_CURVE ( 'NONE', #32935, #50040, #45405, .T. ) ;
#8619 = ADVANCED_FACE ( 'NONE', ( #41588 ), #33836, .T. ) ;
#8620 = ORIENTED_EDGE ( 'NONE', *, *, #1170, .T. ) ;
#8621 = VECTOR ( 'NONE', #26035, 1000.000000000000000 ) ;
#8622 = CARTESIAN_POINT ( 'NONE',  ( 0.3862712429686727678, 1.188820645368945605, 10.00000000000000000 ) ) ;
#8623 = LINE ( 'NONE', #39931, #42801 ) ;
#8624 = EDGE_LOOP ( 'NONE', ( #43173, #11443, #44184, #37020, #16233, #13090 ) ) ;
#8625 = EDGE_CURVE ( 'NONE', #14767, #6332, #39218, .T. ) ;
#8626 = LINE ( 'NONE', #4008, #31394 ) ;
#8627 = DIRECTION ( 'NONE',  ( 1.000000000000000000, -5.326388832052271710E-25, 1.587271980518778491E-16 ) ) ;
#8628 = PLANE ( 'NONE',  #32685 ) ;
#8629 = EDGE_CURVE ( 'NONE', #16858, #5180, #49642, .T. ) ;
#8630 = CARTESIAN_POINT ( 'NONE',  ( -166.6959734468149463, -1.750000000000010658, 80.81828755692798438 ) ) ;
#8631 = ORIENTED_EDGE ( 'NONE', *, *, #9250, .T. ) ;
#8632 = EDGE_CURVE ( 'NONE', #11677, #1108, #14389, .T. ) ;
#8633 = FACE_OUTER_BOUND ( 'NONE', #9362, .T. ) ;
#8634 = EDGE_CURVE ( 'NONE', #25941, #9086, #34167, .T. ) ;
#8635 = DIRECTION ( 'NONE',  ( 1.000000000000000000, -1.331116318405244905E-23, -4.759647537211363479E-16 ) ) ;
#8636 = CARTESIAN_POINT ( 'NONE',  ( -166.6959734468149463, 1.750000000000010658, -119.1817124430720440 ) ) ;
#8637 = CARTESIAN_POINT ( 'NONE',  ( 193.3040265531851105, -1.750000000000010214, -39.18171244307202983 ) ) ;
#8638 = AXIS2_PLACEMENT_3D ( 'NONE', #42271, #11734, #49913 ) ;
#8639 = AXIS2_PLACEMENT_3D ( 'NONE', #1004, #2001, #49896 ) ;
#8640 = FACE_OUTER_BOUND ( 'NONE', #18034, .T. ) ;
#8641 = AXIS2_PLACEMENT_3D ( 'NONE', #21359, #32940, #9808 ) ;
#8642 = CARTESIAN_POINT ( 'NONE',  ( 0.9494396179258391966, -9.954826186926261755, 9.646707543097345905 ) ) ;
#8643 = EDGE_CURVE ( 'NONE', #40814, #47093, #21329, .T. ) ;
#8644 = CARTESIAN_POINT ( 'NONE',  ( 47.87295225382209907, 14.46560184742433641, -2.408242355805840784 ) ) ;
#8645 = VERTEX_POINT ( 'NONE', #30053 ) ;
#8646 = CARTESIAN_POINT ( 'NONE',  ( 350.0000000000000000, -164.9999999999999432, -356.0000000000002274 ) ) ;
#8647 =( BOUNDED_CURVE ( )  B_SPLINE_CURVE ( 3, ( #50529, #46183, #46441, #3625 ),
 .UNSPECIFIED., .F., .F. ) 
 B_SPLINE_CURVE_WITH_KNOTS ( ( 4, 4 ),
 ( 0.000000000000000000, 1.570796326794896558 ),
 .UNSPECIFIED. ) 
 CURVE ( )  GEOMETRIC_REPRESENTATION_ITEM ( )  RATIONAL_B_SPLINE_CURVE ( ( 1.000000000000000000, 0.8047378541243649375, 0.8047378541243649375, 1.000000000000000000 ) ) 
 REPRESENTATION_ITEM ( '' )  );
#8648 =( GEOMETRIC_REPRESENTATION_CONTEXT ( 3 ) GLOBAL_UNCERTAINTY_ASSIGNED_CONTEXT ( ( #46553 ) ) GLOBAL_UNIT_ASSIGNED_CONTEXT ( ( #52, #34965, #46188 ) ) REPRESENTATION_CONTEXT ( 'NONE', 'WORKASPACE' ) );
#8649 = EDGE_CURVE ( 'NONE', #23178, #37052, #25408, .T. ) ;
#8650 = ADVANCED_FACE ( 'NONE', ( #45657 ), #17481, .T. ) ;
#8651 = CARTESIAN_POINT ( 'NONE',  ( -34.10310225234756132, -15.68274378628470345, 1.982731392810465287 ) ) ;
#8652 = AXIS2_PLACEMENT_3D ( 'NONE', #21934, #49328, #10626 ) ;
#8653 = VECTOR ( 'NONE', #40226, 1000.000000000000000 ) ;
#8654 = ORIENTED_EDGE ( 'NONE', *, *, #50555, .F. ) ;
#8655 = CARTESIAN_POINT ( 'NONE',  ( -128.4459734468149179, 0.000000000000000000, -80.93171244307201562 ) ) ;
#8656 = DIRECTION ( 'NONE',  ( 0.000000000000000000, 0.000000000000000000, -1.000000000000000000 ) ) ;
#8657 =( BOUNDED_CURVE ( )  B_SPLINE_CURVE ( 3, ( #32555, #1500, #16898, #44069 ),
 .UNSPECIFIED., .F., .F. ) 
 B_SPLINE_CURVE_WITH_KNOTS ( ( 4, 4 ),
 ( 4.712388980384689674, 6.283185307179586232 ),
 .UNSPECIFIED. ) 
 CURVE ( )  GEOMETRIC_REPRESENTATION_ITEM ( )  RATIONAL_B_SPLINE_CURVE ( ( 1.000000000000000000, 0.8047378541243649375, 0.8047378541243649375, 1.000000000000000000 ) ) 
 REPRESENTATION_ITEM ( '' )  );
#8658 = ORIENTED_EDGE ( 'NONE', *, *, #48813, .F. ) ;
#8659 = AXIS2_PLACEMENT_3D ( 'NONE', #3364, #43375, #34959 ) ;
#8660 = CARTESIAN_POINT ( 'NONE',  ( 113.3040265531850537, 1.749999999999997335, -79.18171244307201562 ) ) ;
#8661 = ORIENTED_EDGE ( 'NONE', *, *, #17382, .T. ) ;
#8662 = ORIENTED_EDGE ( 'NONE', *, *, #39685, .T. ) ;
#8663 = VECTOR ( 'NONE', #37044, 1000.000000000000000 ) ;
#8664 = CARTESIAN_POINT ( 'NONE',  ( -0.2458784654125698022, 0.3384226744270473208, 9.992713367193012175 ) ) ;
#8665 = ORIENTED_EDGE ( 'NONE', *, *, #11415, .T. ) ;
#8666 = FACE_OUTER_BOUND ( 'NONE', #3621, .T. ) ;
#8667 = DIRECTION ( 'NONE',  ( -0.4374820812098793033, -0.3178493372392781624, -0.8411784753765542133 ) ) ;
#8668 = ORIENTED_EDGE ( 'NONE', *, *, #20027, .F. ) ;
#8669 = ADVANCED_FACE ( 'NONE', ( #29285 ), #44897, .F. ) ;
#8670 = CARTESIAN_POINT ( 'NONE',  ( 210.0000000000000568, 0.000000000000000000, 82.56828755692799859 ) ) ;
#8671 = ORIENTED_EDGE ( 'NONE', *, *, #28628, .F. ) ;
#8672 = CARTESIAN_POINT ( 'NONE',  ( 181.0000000000000568, 165.0000000000000000, 343.9999999999998863 ) ) ;
#8673 = FACE_OUTER_BOUND ( 'NONE', #36897, .T. ) ;
#8674 = LINE ( 'NONE', #20449, #14421 ) ;
#8675 = VECTOR ( 'NONE', #12424, 1000.000000000000000 ) ;
#8676 = VERTEX_POINT ( 'NONE', #25435 ) ;
#8677 = LINE ( 'NONE', #4316, #21855 ) ;
#8678 = DIRECTION ( 'NONE',  ( 0.000000000000000000, 0.2223603367690656640, 0.9749645535258950613 ) ) ;
#8679 = ORIENTED_EDGE ( 'NONE', *, *, #48703, .T. ) ;
#8680 = EDGE_CURVE ( 'NONE', #25250, #34536, #4144, .T. ) ;
#8681 = AXIS2_PLACEMENT_3D ( 'NONE', #28105, #43741, #16556 ) ;
#8682 = VERTEX_POINT ( 'NONE', #5925 ) ;
#8683 = ORIENTED_EDGE ( 'NONE', *, *, #22103, .T. ) ;
#8684 = DIRECTION ( 'NONE',  ( 0.000000000000000000, 0.000000000000000000, 1.000000000000000000 ) ) ;
#8685 = VECTOR ( 'NONE', #31298, 1000.000000000000000 ) ;
#8686 = CARTESIAN_POINT ( 'NONE',  ( 355.9999999999999432, -183.0000000000001421, 358.0000000000001705 ) ) ;
#8687 = ORIENTED_EDGE ( 'NONE', *, *, #22439, .F. ) ;
#8688 = DIRECTION ( 'NONE',  ( -1.000000000000000000, 0.000000000000000000, -0.000000000000000000 ) ) ;
#8689 = CARTESIAN_POINT ( 'NONE',  ( -568.6915979970481203, 47.50000000000000000, -173.6700166912652890 ) ) ;
#8690 = CIRCLE ( 'NONE', #11130, 2.000000000000001776 ) ;
#8691 = EDGE_CURVE ( 'NONE', #14822, #32061, #17739, .T. ) ;
#8692 = CARTESIAN_POINT ( 'NONE',  ( 0.7601424845489945792, -1.297311920616997627, 9.927319414211225990 ) ) ;
#8693 = EDGE_CURVE ( 'NONE', #22974, #35388, #13861, .T. ) ;
#8694 = COLOUR_RGB ( '',0.7921568627450980005, 0.8196078431372548767, 0.9333333333333333481 ) ;
#8695 = DIRECTION ( 'NONE',  ( 0.000000000000000000, 1.000000000000000000, 0.000000000000000000 ) ) ;
#8696 = CARTESIAN_POINT ( 'NONE',  ( -6.695973446814940111, 0.000000000000000000, 165.0000000000000000 ) ) ;
#8697 = CARTESIAN_POINT ( 'NONE',  ( 32.27890028733795447, 1.750000000000009548, 41.84341382277508359 ) ) ;
#8698 = EDGE_CURVE ( 'NONE', #45670, #35747, #8204, .T. ) ;
#8699 = CARTESIAN_POINT ( 'NONE',  ( -64.99999999999971578, 17.00000000000000000, -84.99999999999998579 ) ) ;
#8700 = AXIS2_PLACEMENT_3D ( 'NONE', #23877, #11828, #43613 ) ;
#8701 = LINE ( 'NONE', #32301, #44886 ) ;
#8702 = VECTOR ( 'NONE', #13933, 1000.000000000000000 ) ;
#8703 = EDGE_CURVE ( 'NONE', #16759, #12798, #21427, .T. ) ;
#8704 = EDGE_CURVE ( 'NONE', #19705, #48470, #30366, .T. ) ;
#8705 = LINE ( 'NONE', #39499, #14236 ) ;
#8706 = UNCERTAINTY_MEASURE_WITH_UNIT (LENGTH_MEASURE( 1.000000000000000082E-05 ), #5214, 'distance_accuracy_value', 'NONE');
#8707 = LINE ( 'NONE', #20737, #46988 ) ;
#8708 = ORIENTED_EDGE ( 'NONE', *, *, #48405, .T. ) ;
#8709 = FACE_OUTER_BOUND ( 'NONE', #48185, .T. ) ;
#8710 = EDGE_CURVE ( 'NONE', #45864, #17776, #38765, .T. ) ;
#8711 = CARTESIAN_POINT ( 'NONE',  ( 0.8282505383454039638, 1.889063466747038289, 9.894754715216722118 ) ) ;
#8712 = DIRECTION ( 'NONE',  ( 1.132880637372608740E-16, 4.718402560806925739E-50, 1.000000000000000000 ) ) ;
#8713 = CARTESIAN_POINT ( 'NONE',  ( -50.11058929355266400, 7.578863168071933387, 7.455576670931136185 ) ) ;
#8714 = ORIENTED_EDGE ( 'NONE', *, *, #9844, .T. ) ;
#8715 = AXIS2_PLACEMENT_3D ( 'NONE', #21023, #21270, #13060 ) ;
#8716 = LINE ( 'NONE', #4604, #2669 ) ;
#8717 = AXIS2_PLACEMENT_3D ( 'NONE', #16423, #15924, #28233 ) ;
#8718 = DIRECTION ( 'NONE',  ( 0.000000000000000000, -2.265761274745217480E-16, 1.000000000000000000 ) ) ;
#8719 = VERTEX_POINT ( 'NONE', #35434 ) ;
#8720 = CARTESIAN_POINT ( 'NONE',  ( 0.3862712429686727678, 1.188820645368945605, 3.333333333333333481 ) ) ;
#8721 = CYLINDRICAL_SURFACE ( 'NONE', #29852, 3.749999999999975575 ) ;
#8722 = CARTESIAN_POINT ( 'NONE',  ( -126.6959734468149321, 1.749999999999996891, 160.8182875569279702 ) ) ;
#8723 = ORIENTED_EDGE ( 'NONE', *, *, #42189, .F. ) ;
#8724 =( LENGTH_UNIT ( ) NAMED_UNIT ( * ) SI_UNIT ( .MILLI., .METRE. ) );
#8725 = VERTEX_POINT ( 'NONE', #31582 ) ;
#8726 = ORIENTED_EDGE ( 'NONE', *, *, #41819, .T. ) ;
#8727 = CIRCLE ( 'NONE', #25934, 4.000000000000003553 ) ;
#8728 = ORIENTED_EDGE ( 'NONE', *, *, #48562, .T. ) ;
#8729 = FACE_OUTER_BOUND ( 'NONE', #45215, .T. ) ;
#8730 = VECTOR ( 'NONE', #24841, 1000.000000000000000 ) ;
#8731 = VERTEX_POINT ( 'NONE', #11045 ) ;
#8732 = CARTESIAN_POINT ( 'NONE',  ( 80.00000000000153477, 17.00000000000000000, 35.00000000000000000 ) ) ;
#8733 = CARTESIAN_POINT ( 'NONE',  ( 35.00000000000091660, 17.00000000000000000, 0.000000000000000000 ) ) ;
#8734 = CARTESIAN_POINT ( 'NONE',  ( -206.6959734468149463, -1.750000000000010658, -119.1817124430720440 ) ) ;
#8735 = CARTESIAN_POINT ( 'NONE',  ( 5.551115123125782702E-14, -164.9999999999999432, 343.9999999999997726 ) ) ;
#8736 = EDGE_LOOP ( 'NONE', ( #24943, #33909, #5087, #14298 ) ) ;
#8737 = AXIS2_PLACEMENT_3D ( 'NONE', #21080, #4686, #5428 ) ;
#8738 = CARTESIAN_POINT ( 'NONE',  ( 7.574282714737766931, -6.549555713337890772, 3.092310436554633224 ) ) ;
#8739 = ORIENTED_EDGE ( 'NONE', *, *, #32485, .T. ) ;
#8740 = CARTESIAN_POINT ( 'NONE',  ( -9.643172164747307207, 6.123233995736766282E-16, 5.000000000000000000 ) ) ;
#8741 = CARTESIAN_POINT ( 'NONE',  ( -165.4943081650521037, -61.66198943095990614, -93.79675437945473959 ) ) ;
#8742 = SHAPE_REPRESENTATION ( 'solar panel', ( #45486 ), #32386 ) ;
#8743 = EDGE_LOOP ( 'NONE', ( #16432, #14192, #6879, #5546 ) ) ;
#8744 = CARTESIAN_POINT ( 'NONE',  ( 195.0540265531851105, 1.025126265847089879, 82.56828755692798438 ) ) ;
#8745 = LINE ( 'NONE', #31074, #2979 ) ;
#8746 = ORIENTED_EDGE ( 'NONE', *, *, #20317, .T. ) ;
#8747 = CARTESIAN_POINT ( 'NONE',  ( -11.73320209285699889, 11.96063479729179768, 9.403735324607438884 ) ) ;
#8748 = LINE ( 'NONE', #32603, #38572 ) ;
#8749 = FACE_OUTER_BOUND ( 'NONE', #17973, .T. ) ;
#8750 = EDGE_CURVE ( 'NONE', #33652, #40759, #18722, .T. ) ;
#8751 = EDGE_CURVE ( 'NONE', #32061, #14517, #2, .T. ) ;
#8752 = ORIENTED_EDGE ( 'NONE', *, *, #38823, .T. ) ;
#8753 = DIRECTION ( 'NONE',  ( -1.000000000000000000, 0.000000000000000000, -2.958228394578794270E-31 ) ) ;
#8754 = AXIS2_PLACEMENT_3D ( 'NONE', #39926, #48317, #4756 ) ;
#8755 = DIRECTION ( 'NONE',  ( -1.586032892321652236E-16, -1.000000000000000000, -2.288264760618012091E-48 ) ) ;
#8756 = ADVANCED_FACE ( 'NONE', ( #42582 ), #25622, .T. ) ;
#8757 = FACE_OUTER_BOUND ( 'NONE', #28923, .T. ) ;
#8758 = ORIENTED_EDGE ( 'NONE', *, *, #12442, .T. ) ;
#8759 = ORIENTED_EDGE ( 'NONE', *, *, #50350, .F. ) ;
#8760 = ADVANCED_FACE ( 'NONE', ( #42081 ), #39024, .T. ) ;
#8761 = PRODUCT_CONTEXT ( 'NONE', #49814, 'mechanical' ) ;
#8762 = EDGE_CURVE ( 'NONE', #18285, #22723, #7463, .T. ) ;
#8763 = PLANE ( 'NONE',  #30229 ) ;
#8764 = CARTESIAN_POINT ( 'NONE',  ( 191.5540265531851105, 0.000000000000000000, -120.9317124430720156 ) ) ;
#8765 = CARTESIAN_POINT ( 'NONE',  ( 214.9999999999999432, -175.0000000000000000, 10.00000000000000000 ) ) ;
#8766 = CARTESIAN_POINT ( 'NONE',  ( 181.0000000000000000, -81.49999999999995737, -115.0000000000001563 ) ) ;
#8767 = CARTESIAN_POINT ( 'NONE',  ( 71.55402655318505367, 0.000000000000000000, 165.0000000000000000 ) ) ;
#8768 = ORIENTED_EDGE ( 'NONE', *, *, #35761, .F. ) ;
#8769 = EDGE_CURVE ( 'NONE', #9583, #8296, #27209, .T. ) ;
#8770 = PLANE ( 'NONE',  #49258 ) ;
#8771 = EDGE_CURVE ( 'NONE', #23064, #35976, #7715, .T. ) ;
#8772 = DIRECTION ( 'NONE',  ( -2.220446049250312588E-16, -0.7071067811865475727, 0.7071067811865474617 ) ) ;
#8773 = FACE_BOUND ( 'NONE', #2397, .T. ) ;
#8774 = CARTESIAN_POINT ( 'NONE',  ( 75.05402655318509630, 2.143131898507880377E-16, 82.56828755692799859 ) ) ;
#8775 = VECTOR ( 'NONE', #20707, 1000.000000000000000 ) ;
#8776 = ORIENTED_EDGE ( 'NONE', *, *, #25370, .T. ) ;
#8777 = LINE ( 'NONE', #322, #49325 ) ;
#8778 = VERTEX_POINT ( 'NONE', #43105 ) ;
#8779 = CARTESIAN_POINT ( 'NONE',  ( -1.011271242968677875, -0.7347315653656004697, 10.00000000000000000 ) ) ;
#8780 = ORIENTED_EDGE ( 'NONE', *, *, #3194, .T. ) ;
#8781 = CARTESIAN_POINT ( 'NONE',  ( 154.3291528190321458, 1.750000000000010214, 119.7931612910808781 ) ) ;
#8782 = CARTESIAN_POINT ( 'NONE',  ( 342.8284271247460993, -183.0000000000001137, -358.0000000000003411 ) ) ;
#8783 = CARTESIAN_POINT ( 'NONE',  ( -84.94597344681494633, 2.143131898507880377E-16, -80.93171244307201562 ) ) ;
#8784 = DIRECTION ( 'NONE',  ( -1.000000000000000000, -0.000000000000000000, -0.000000000000000000 ) ) ;
#8785 = ORIENTED_EDGE ( 'NONE', *, *, #40244, .F. ) ;
#8786 = CARTESIAN_POINT ( 'NONE',  ( -114.9999999999994031, 16.00000000000000000, -30.00000000000000000 ) ) ;
#8787 = ORIENTED_EDGE ( 'NONE', *, *, #36574, .F. ) ;
#8788 = LINE ( 'NONE', #40583, #44306 ) ;
#8789 = CARTESIAN_POINT ( 'NONE',  ( -19.99999999999846523, 17.00000000000000000, 35.00000000000000000 ) ) ;
#8790 = DIRECTION ( 'NONE',  ( 1.132880637372608740E-16, 4.718402560806925739E-50, 1.000000000000000000 ) ) ;
#8791 = EDGE_CURVE ( 'NONE', #13767, #42432, #7971, .T. ) ;
#8792 = ORIENTED_EDGE ( 'NONE', *, *, #24456, .F. ) ;
#8793 = ORIENTED_EDGE ( 'NONE', *, *, #9890, .T. ) ;
#8794 = DIRECTION ( 'NONE',  ( -0.000000000000000000, -1.000000000000000000, -0.000000000000000000 ) ) ;
#8795 = EDGE_CURVE ( 'NONE', #6842, #50107, #30550, .T. ) ;
#8796 =( BOUNDED_CURVE ( )  B_SPLINE_CURVE ( 3, ( #13615, #43642, #40321, #12861 ),
 .UNSPECIFIED., .F., .F. ) 
 B_SPLINE_CURVE_WITH_KNOTS ( ( 4, 4 ),
 ( 4.712388980384689674, 6.283185307179586232 ),
 .UNSPECIFIED. ) 
 CURVE ( )  GEOMETRIC_REPRESENTATION_ITEM ( )  RATIONAL_B_SPLINE_CURVE ( ( 1.000000000000000000, 0.8047378541243649375, 0.8047378541243649375, 1.000000000000000000 ) ) 
 REPRESENTATION_ITEM ( '' )  );
#8797 = ORIENTED_EDGE ( 'NONE', *, *, #46791, .F. ) ;
#8798 = DIRECTION ( 'NONE',  ( 1.000000000000000000, 0.000000000000000000, 0.000000000000000000 ) ) ;
#8799 = CARTESIAN_POINT ( 'NONE',  ( 35.05402655318504657, 2.143131898507880377E-16, -157.4317124430720014 ) ) ;
#8800 = FACE_OUTER_BOUND ( 'NONE', #21296, .T. ) ;
#8801 = ORIENTED_EDGE ( 'NONE', *, *, #45266, .T. ) ;
#8802 = CARTESIAN_POINT ( 'NONE',  ( 181.0000000000000568, 175.0000000000000284, 355.9999999999998863 ) ) ;
#8803 =( BOUNDED_CURVE ( )  B_SPLINE_CURVE ( 3, ( #20866, #35796, #28565, #43696 ),
 .UNSPECIFIED., .F., .F. ) 
 B_SPLINE_CURVE_WITH_KNOTS ( ( 4, 4 ),
 ( 0.000000000000000000, 1.570796326794896558 ),
 .UNSPECIFIED. ) 
 CURVE ( )  GEOMETRIC_REPRESENTATION_ITEM ( )  RATIONAL_B_SPLINE_CURVE ( ( 1.000000000000000000, 0.8047378541243649375, 0.8047378541243649375, 1.000000000000000000 ) ) 
 REPRESENTATION_ITEM ( '' )  );
#8804 = CYLINDRICAL_SURFACE ( 'NONE', #15276, 1.750000000000008438 ) ;
#8805 = CARTESIAN_POINT ( 'NONE',  ( -0.7849184246622071814, 1.242376769534369041, 9.958264684458713489 ) ) ;
#8806 = CARTESIAN_POINT ( 'NONE',  ( -2.961022939495062900, 16.59676755884084187, 2.590526750877053086 ) ) ;
#8807 = ORIENTED_EDGE ( 'NONE', *, *, #44670, .F. ) ;
#8808 = ORIENTED_EDGE ( 'NONE', *, *, #1667, .T. ) ;
#8809 = ORIENTED_EDGE ( 'NONE', *, *, #28158, .T. ) ;
#8810 = FACE_OUTER_BOUND ( 'NONE', #10918, .T. ) ;
#8811 = LINE ( 'NONE', #28554, #19979 ) ;
#8812 =( BOUNDED_CURVE ( )  B_SPLINE_CURVE ( 3, ( #10265, #29508, #49962, #33624 ),
 .UNSPECIFIED., .F., .F. ) 
 B_SPLINE_CURVE_WITH_KNOTS ( ( 4, 4 ),
 ( 0.000000000000000000, 1.570796326794896558 ),
 .UNSPECIFIED. ) 
 CURVE ( )  GEOMETRIC_REPRESENTATION_ITEM ( )  RATIONAL_B_SPLINE_CURVE ( ( 1.000000000000000000, 0.8047378541243649375, 0.8047378541243649375, 1.000000000000000000 ) ) 
 REPRESENTATION_ITEM ( '' )  );
#8813 = VERTEX_POINT ( 'NONE', #8732 ) ;
#8814 = DIRECTION ( 'NONE',  ( 0.000000000000000000, 0.000000000000000000, 1.000000000000000000 ) ) ;
#8815 = VERTEX_POINT ( 'NONE', #1281 ) ;
#8816 = VERTEX_POINT ( 'NONE', #20760 ) ;
#8817 = CARTESIAN_POINT ( 'NONE',  ( -124.9459734468149463, 2.143131898507847836E-16, 79.06828755692798438 ) ) ;
#8818 = CARTESIAN_POINT ( 'NONE',  ( 1.512516825103249918, -0.5229758018505162864, 9.919954280166518146 ) ) ;
#8819 = DIRECTION ( 'NONE',  ( 0.000000000000000000, -2.537652627714643577E-15, -1.000000000000000000 ) ) ;
#8820 = AXIS2_PLACEMENT_3D ( 'NONE', #13722, #44754, #5773 ) ;
#8821 = CARTESIAN_POINT ( 'NONE',  ( -119.9999999999984652, 17.00000000000000000, 35.00000000000000000 ) ) ;
#8822 = LINE ( 'NONE', #36032, #6096 ) ;
#8823 = CARTESIAN_POINT ( 'NONE',  ( 8.277096487746778308, -33.14818118907697198, 7.455576670931136185 ) ) ;
#8824 = ORIENTED_EDGE ( 'NONE', *, *, #21778, .T. ) ;
#8825 = EDGE_CURVE ( 'NONE', #32291, #10429, #24381, .T. ) ;
#8826 = FACE_OUTER_BOUND ( 'NONE', #21803, .T. ) ;
#8827 = CARTESIAN_POINT ( 'NONE',  ( 30.00000000000062172, 17.00000000000000000, -54.99999999999999289 ) ) ;
#8828 = CARTESIAN_POINT ( 'NONE',  ( -0.1475726264153620626, -1.496347932843211215, 9.927319414211227766 ) ) ;
#8829 = DIRECTION ( 'NONE',  ( -1.000000000000000000, 0.000000000000000000, 0.000000000000000000 ) ) ;
#8830 = ORIENTED_EDGE ( 'NONE', *, *, #48203, .F. ) ;
#8831 = DIRECTION ( 'NONE',  ( -4.758098676964957447E-16, -1.000000000000000000, 7.143884938411937192E-48 ) ) ;
#8832 = ORIENTED_EDGE ( 'NONE', *, *, #9531, .T. ) ;
#8833 = CARTESIAN_POINT ( 'NONE',  ( -6.695973446814940111, 1.750000000000024203, -79.18171244307201562 ) ) ;
#8834 = DIRECTION ( 'NONE',  ( -0.000000000000000000, -0.000000000000000000, -1.000000000000000000 ) ) ;
#8835 = ORIENTED_EDGE ( 'NONE', *, *, #33042, .T. ) ;
#8836 = CARTESIAN_POINT ( 'NONE',  ( -127.7210997126620242, 1.749999999999996669, -38.15658617722495194 ) ) ;
#8837 = CARTESIAN_POINT ( 'NONE',  ( -177.4999999999999716, 112.5000000000000000, -10.00000000000000178 ) ) ;
#8838 = CARTESIAN_POINT ( 'NONE',  ( 360.0000000000000000, -166.6568542494924543, -341.6568542494926533 ) ) ;
#8839 = CARTESIAN_POINT ( 'NONE',  ( -114.9999999999981526, 16.00000000000000000, 65.00000000000000000 ) ) ;
#8840 = VERTEX_POINT ( 'NONE', #36442 ) ;
#8841 = VERTEX_POINT ( 'NONE', #16410 ) ;
#8842 = CARTESIAN_POINT ( 'NONE',  ( -3.239037401336969602, -50.00000000000000711, -8.917361510505369182 ) ) ;
#8843 = CARTESIAN_POINT ( 'NONE',  ( 16.52264463346132572, -2.779753662172757878, 9.403735324607438884 ) ) ;
#8844 = ADVANCED_FACE ( 'NONE', ( #17171 ), #16171, .F. ) ;
#8845 = VECTOR ( 'NONE', #6093, 1000.000000000000000 ) ;
#8846 = EDGE_LOOP ( 'NONE', ( #29349, #46, #33778, #18756 ) ) ;
#8847 = ORIENTED_EDGE ( 'NONE', *, *, #18399, .F. ) ;
#8848 = CARTESIAN_POINT ( 'NONE',  ( -0.1287570809895658697, 0.3962735484563123523, 10.00000000000000000 ) ) ;
#8849 = CARTESIAN_POINT ( 'NONE',  ( -114.9999999999978542, 17.00000000000000000, 115.0000000000000142 ) ) ;
#8850 = PLANE ( 'NONE',  #14113 ) ;
#8851 = ORIENTED_EDGE ( 'NONE', *, *, #6207, .T. ) ;
#8852 = VERTEX_POINT ( 'NONE', #24132 ) ;
#8853 = ORIENTED_EDGE ( 'NONE', *, *, #21343, .F. ) ;
#8854 = CARTESIAN_POINT ( 'NONE',  ( -49.89397392339119364, 8.245536726717011433, 7.906207997025717304 ) ) ;
#8855 = CARTESIAN_POINT ( 'NONE',  ( 356.0000000000000000, 174.9999999999996589, -340.0000000000002842 ) ) ;
#8856 = ORIENTED_EDGE ( 'NONE', *, *, #45880, .F. ) ;
#8857 = VERTEX_POINT ( 'NONE', #40030 ) ;
#8858 = CARTESIAN_POINT ( 'NONE',  ( -2.945500763482279627, -16.64098165802040086, -9.008049429158100807 ) ) ;
#8859 = CYLINDRICAL_SURFACE ( 'NONE', #38825, 4.000000000000003553 ) ;
#8860 = ORIENTED_EDGE ( 'NONE', *, *, #43388, .F. ) ;
#8861 = ORIENTED_EDGE ( 'NONE', *, *, #45295, .F. ) ;
#8862 = CARTESIAN_POINT ( 'NONE',  ( 181.0000000000000000, -184.9999999999999716, -358.0000000000001705 ) ) ;
#8863 = CARTESIAN_POINT ( 'NONE',  ( -14.91630425054805187, 7.943683830272226132, -9.008049429158102583 ) ) ;
#8864 = ORIENTED_EDGE ( 'NONE', *, *, #2475, .T. ) ;
#8865 = CARTESIAN_POINT ( 'NONE',  ( 181.0000000000000284, -174.9999999999999716, -99.00000000000014211 ) ) ;
#8866 = DIRECTION ( 'NONE',  ( 0.000000000000000000, 0.000000000000000000, 1.000000000000000000 ) ) ;
#8867 = DIRECTION ( 'NONE',  ( 0.000000000000000000, 1.000000000000000000, 0.000000000000000000 ) ) ;
#8868 = DIRECTION ( 'NONE',  ( 0.000000000000000000, 0.000000000000000000, -1.000000000000000000 ) ) ;
#8869 = ORIENTED_EDGE ( 'NONE', *, *, #24926, .F. ) ;
#8870 = ADVANCED_FACE ( 'NONE', ( #32839 ), #36181, .F. ) ;
#8871 = CARTESIAN_POINT ( 'NONE',  ( -0.3862712429686809279, -1.188820645368943163, 10.00000000000000000 ) ) ;
#8872 = CARTESIAN_POINT ( 'NONE',  ( 350.0000000000000000, 169.0000000000000000, -344.0000000000001705 ) ) ;
#8873 = CYLINDRICAL_SURFACE ( 'NONE', #46562, 1.750000000000015543 ) ;
#8874 = EDGE_CURVE ( 'NONE', #3623, #44566, #28476, .T. ) ;
#8875 = LINE ( 'NONE', #24033, #2568 ) ;
#8876 = ADVANCED_FACE ( 'NONE', ( #20512 ), #48421, .F. ) ;
#8877 = B_SPLINE_CURVE_WITH_KNOTS ( 'NONE', 3,
 ( #15988, #46731, #43181, #16496 ),
 .UNSPECIFIED., .F., .F.,
 ( 4, 4 ),
 ( 0.9895749839358303213, 1.000000000000000000 ),
 .UNSPECIFIED. ) ;
#8878 = DIRECTION ( 'NONE',  ( -1.612977847700450206E-50, 0.000000000000000000, -1.000000000000000000 ) ) ;
#8879 = ADVANCED_FACE ( 'NONE', ( #27714 ), #31832, .F. ) ;
#8880 = EDGE_CURVE ( 'NONE', #31952, #34755, #39343, .T. ) ;
#8881 = CARTESIAN_POINT ( 'NONE',  ( 129.9999999999999432, 17.00000000000000000, -90.00000000000000000 ) ) ;
#8882 = LINE ( 'NONE', #21187, #14850 ) ;
#8883 = ADVANCED_FACE ( 'NONE', ( #1023 ), #12818, .T. ) ;
#8884 = ORIENTED_EDGE ( 'NONE', *, *, #22024, .F. ) ;
#8885 = CARTESIAN_POINT ( 'NONE',  ( 135.0000000000006253, 16.00000000000000000, -30.00000000000000000 ) ) ;
#8886 = DIRECTION ( 'NONE',  ( 0.000000000000000000, 0.000000000000000000, 1.000000000000000000 ) ) ;
#8887 = EDGE_LOOP ( 'NONE', ( #38105, #24327, #36526, #40885 ) ) ;
#8888 = DIRECTION ( 'NONE',  ( 0.000000000000000000, 0.000000000000000000, 1.000000000000000000 ) ) ;
#8889 = CARTESIAN_POINT ( 'NONE',  ( -128.4459734468149463, 1.025126265847081886, -40.93171244307202272 ) ) ;
#8890 = CARTESIAN_POINT ( 'NONE',  ( 31.55402655318503236, -1.025126265847089879, -77.43171244307200141 ) ) ;
#8891 = ORIENTED_EDGE ( 'NONE', *, *, #3186, .F. ) ;
#8892 = CARTESIAN_POINT ( 'NONE',  ( 1.011271242968683648, 0.7347315653655930312, 10.00000000000000000 ) ) ;
#8893 = B_SPLINE_SURFACE_WITH_KNOTS ( 'NONE', 3, 3, ( 
 ( #31987, #178, #12463, #50661 ),
 ( #11458, #42736, #23246, #22989 ),
 ( #39436, #672, #27362, #27114 ),
 ( #38666, #4519, #46564, #39183 ) ),
 .UNSPECIFIED., .F., .F., .F.,
 ( 4, 4 ),
 ( 4, 4 ),
 ( 0.000000000000000000, 1.000000000000000000 ),
 ( 0.000000000000000000, 1.000000000000000000 ),
 .UNSPECIFIED. ) ;
#8894 = EDGE_CURVE ( 'NONE', #17600, #41530, #24626, .T. ) ;
#8896 = ORIENTED_EDGE ( 'NONE', *, *, #39529, .F. ) ;
#8895 = ADVANCED_FACE ( 'NONE', ( #32074, #35691 ), #9214, .T. ) ;
#8897 = EDGE_LOOP ( 'NONE', ( #27285, #31828, #17440, #29243 ) ) ;
#8898 = CARTESIAN_POINT ( 'NONE',  ( -0.3862712429686809279, -1.188820645368943163, 10.00000000000000000 ) ) ;
#8899 = EDGE_CURVE ( 'NONE', #36068, #2414, #44097, .T. ) ;
#8900 = EDGE_CURVE ( 'NONE', #19122, #42389, #8970, .T. ) ;
#8901 = ORIENTED_EDGE ( 'NONE', *, *, #2950, .T. ) ;
#8902 = CARTESIAN_POINT ( 'NONE',  ( 356.0000000000000568, 175.0000000000000284, -94.00000000000019895 ) ) ;
#8903 = FACE_OUTER_BOUND ( 'NONE', #49303, .T. ) ;
#8904 = EDGE_LOOP ( 'NONE', ( #50306, #32455 ) ) ;
#8905 = ORIENTED_EDGE ( 'NONE', *, *, #17405, .T. ) ;
#8906 = EDGE_CURVE ( 'NONE', #33474, #41151, #26255, .T. ) ;
#8907 = CARTESIAN_POINT ( 'NONE',  ( 5.083187235775197266, 8.611690166631179366, 9.646707543097347681 ) ) ;
#8908 = EDGE_LOOP ( 'NONE', ( #47312, #39129, #6170, #41664, #27842 ) ) ;
#8909 = CARTESIAN_POINT ( 'NONE',  ( 168.9999999999997158, -164.9999999999999432, 341.9999999999998863 ) ) ;
#8910 = DIRECTION ( 'NONE',  ( 1.000000000000000000, 0.000000000000000000, 0.000000000000000000 ) ) ;
#8911 = CIRCLE ( 'NONE', #44128, 4.000000000000003553 ) ;
#8912 = CARTESIAN_POINT ( 'NONE',  ( -48.44597344681495343, 0.000000000000000000, 165.0000000000000000 ) ) ;
#8913 = ORIENTED_EDGE ( 'NONE', *, *, #10025, .F. ) ;
#8914 = VECTOR ( 'NONE', #26803, 1000.000000000000000 ) ;
#8915 = FACE_OUTER_BOUND ( 'NONE', #12822, .T. ) ;
#8916 = CARTESIAN_POINT ( 'NONE',  ( 38.83576208387761142, 2.688010569040066411, 741.9425600500172777 ) ) ;
#8917 = ORIENTED_EDGE ( 'NONE', *, *, #28731, .T. ) ;
#8918 = VERTEX_POINT ( 'NONE', #39527 ) ;
#8919 = ORIENTED_EDGE ( 'NONE', *, *, #18737, .F. ) ;
#8920 = DIRECTION ( 'NONE',  ( 0.000000000000000000, 0.000000000000000000, 1.000000000000000000 ) ) ;
#8921 = LINE ( 'NONE', #32290, #37352 ) ;
#8922 = ORIENTED_EDGE ( 'NONE', *, *, #27708, .F. ) ;
#8923 = EDGE_CURVE ( 'NONE', #42464, #3579, #35634, .T. ) ;
#8924 = B_SPLINE_CURVE_WITH_KNOTS ( 'NONE', 3,
 ( #27366, #15324, #27882, #11713 ),
 .UNSPECIFIED., .F., .F.,
 ( 4, 4 ),
 ( 0.001403500796105017863, 0.001586656765098935253 ),
 .UNSPECIFIED. ) ;
#8925 = CARTESIAN_POINT ( 'NONE',  ( 0.9602803029231544718, -0.8490247040095941777, 9.976582533991681601 ) ) ;
#8926 = CARTESIAN_POINT ( 'NONE',  ( 195.0540265531851105, 1.025126265847089657, -80.93171244307201562 ) ) ;
#8927 = LINE ( 'NONE', #32295, #21492 ) ;
#8928 = VECTOR ( 'NONE', #39085, 1000.000000000000000 ) ;
#8929 = EDGE_CURVE ( 'NONE', #17047, #50635, #5104, .T. ) ;
#8930 = CARTESIAN_POINT ( 'NONE',  ( -0.3522231071495601773, 1.258647432227772534, 9.945465957785110334 ) ) ;
#8931 = DIRECTION ( 'NONE',  ( 1.000000000000000000, 0.000000000000000000, 0.000000000000000000 ) ) ;
#8932 = EDGE_CURVE ( 'NONE', #11488, #43863, #40845, .T. ) ;
#8933 = CARTESIAN_POINT ( 'NONE',  ( 0.000000000000000000, -165.1999999999999602, -340.2000000000001592 ) ) ;
#8934 = CARTESIAN_POINT ( 'NONE',  ( -64.99999999999815259, 16.00000000000000000, 90.00000000000000000 ) ) ;
#8935 = EDGE_CURVE ( 'NONE', #34164, #7228, #2269, .T. ) ;
#8936 = DIRECTION ( 'NONE',  ( 0.000000000000000000, 0.000000000000000000, 1.000000000000000000 ) ) ;
#8937 = CARTESIAN_POINT ( 'NONE',  ( 0.9989200098981507736, 1.123829893718967687, 9.927319414211233095 ) ) ;
#8938 = DIRECTION ( 'NONE',  ( 1.000000000000000000, 0.000000000000000000, 0.000000000000000000 ) ) ;
#8939 = ADVANCED_FACE ( 'NONE', ( #49177 ), #25631, .F. ) ;
#8940 = CARTESIAN_POINT ( 'NONE',  ( -6.695973446814940111, 1.750000000000023315, 0.8182875569279768335 ) ) ;
#8941 = CARTESIAN_POINT ( 'NONE',  ( 10.50000000000000178, -46.01315789473684248, -5.916985404131818171 ) ) ;
#8942 = VERTEX_POINT ( 'NONE', #41027 ) ;
#8943 = DIRECTION ( 'NONE',  ( 0.000000000000000000, 2.537652627714642000E-15, 1.000000000000000000 ) ) ;
#8944 =( BOUNDED_CURVE ( )  B_SPLINE_CURVE ( 3, ( #21258, #1765, #6615, #10467 ),
 .UNSPECIFIED., .F., .F. ) 
 B_SPLINE_CURVE_WITH_KNOTS ( ( 4, 4 ),
 ( 4.712388980384689674, 6.283185307179586232 ),
 .UNSPECIFIED. ) 
 CURVE ( )  GEOMETRIC_REPRESENTATION_ITEM ( )  RATIONAL_B_SPLINE_CURVE ( ( 1.000000000000000000, 0.8047378541243649375, 0.8047378541243649375, 1.000000000000000000 ) ) 
 REPRESENTATION_ITEM ( '' )  );
#8945 = PLANE ( 'NONE',  #25321 ) ;
#8946 = FACE_OUTER_BOUND ( 'NONE', #24191, .T. ) ;
#8947 = DIRECTION ( 'NONE',  ( -3.172065784643302499E-16, -1.000000000000000000, 2.537652627714642000E-15 ) ) ;
#8948 = EDGE_CURVE ( 'NONE', #35933, #34629, #29228, .T. ) ;
#8949 = AXIS2_PLACEMENT_3D ( 'NONE', #47468, #28008, #8021 ) ;
#8950 = ORIENTED_EDGE ( 'NONE', *, *, #32185, .F. ) ;
#8951 = CARTESIAN_POINT ( 'NONE',  ( -5.670847180967843570, 1.750000000000023537, 119.7931612910808781 ) ) ;
#8952 = CARTESIAN_POINT ( 'NONE',  ( -46.69597344681494633, 1.750000000000009992, -159.1817124430720298 ) ) ;
#8953 = EDGE_CURVE ( 'NONE', #46082, #3725, #25376, .T. ) ;
#8954 = ORIENTED_EDGE ( 'NONE', *, *, #30646, .F. ) ;
#8955 = AXIS2_PLACEMENT_3D ( 'NONE', #1032, #11826, #23616 ) ;
#8956 = CARTESIAN_POINT ( 'NONE',  ( 15.62858259096121216, -5.755205073598614440, -9.683996418299976483 ) ) ;
#8957 = DIRECTION ( 'NONE',  ( 0.000000000000000000, -0.000000000000000000, -1.000000000000000000 ) ) ;
#8958 = AXIS2_PLACEMENT_3D ( 'NONE', #44076, #8943, #19983 ) ;
#8959 = CARTESIAN_POINT ( 'NONE',  ( 0.9489147763962141324, -2.465022012281490760, 9.847478953136988622 ) ) ;
#8960 = ORIENTED_EDGE ( 'NONE', *, *, #41855, .F. ) ;
#8961 = ORIENTED_EDGE ( 'NONE', *, *, #7697, .F. ) ;
#8962 = EDGE_LOOP ( 'NONE', ( #24262, #42024, #22097 ) ) ;
#8963 = VECTOR ( 'NONE', #33505, 1000.000000000000000 ) ;
#8964 = EDGE_CURVE ( 'NONE', #36804, #34812, #46051, .T. ) ;
#8965 = ADVANCED_FACE ( 'NONE', ( #37451 ), #17907, .F. ) ;
#8966 = VERTEX_POINT ( 'NONE', #33588 ) ;
#8967 = DIRECTION ( 'NONE',  ( 0.000000000000000000, 1.000000000000000000, -0.000000000000000000 ) ) ;
#8968 = CARTESIAN_POINT ( 'NONE',  ( -0.3370904143228963812, 0.2449105217885287067, 10.00000000000000000 ) ) ;
#8969 = ORIENTED_EDGE ( 'NONE', *, *, #30339, .T. ) ;
#8970 = LINE ( 'NONE', #40274, #10673 ) ;
#8971 = CYLINDRICAL_SURFACE ( 'NONE', #25880, 1.750000000000015543 ) ;
#8972 = ADVANCED_FACE ( 'NONE', ( #18419 ), #25886, .T. ) ;
#8973 = CARTESIAN_POINT ( 'NONE',  ( 168.9999999999999716, -180.9999999999999716, -350.0000000000001705 ) ) ;
#8974 = EDGE_CURVE ( 'NONE', #34532, #36302, #41526, .T. ) ;
#8975 = CARTESIAN_POINT ( 'NONE',  ( -15.80799809827351154, 29.65358618225718956, -8.016098858316205167 ) ) ;
#8976 = EDGE_LOOP ( 'NONE', ( #44232, #3834, #6777, #10085 ) ) ;
#8977 = ADVANCED_FACE ( 'NONE', ( #6371, #21515 ), #22019, .T. ) ;
#8978 = DIRECTION ( 'NONE',  ( 0.000000000000000000, -0.000000000000000000, -1.000000000000000000 ) ) ;
#8979 = ORIENTED_EDGE ( 'NONE', *, *, #27450, .F. ) ;
#8980 = B_SPLINE_CURVE_WITH_KNOTS ( 'NONE', 3,
 ( #1089, #37022, #13633, #28789 ),
 .UNSPECIFIED., .F., .F.,
 ( 4, 4 ),
 ( 0.8097120833243712790, 0.9322955464062560038 ),
 .UNSPECIFIED. ) ;
#8981 = PLANE ( 'NONE',  #23473 ) ;
#8982 = CARTESIAN_POINT ( 'NONE',  ( 155.0540265531850537, -1.025126265847089213, 42.56828755692799149 ) ) ;
#8983 = ORIENTED_EDGE ( 'NONE', *, *, #1571, .F. ) ;
#8984 = CARTESIAN_POINT ( 'NONE',  ( 193.3040265531851105, 1.750000000000010658, 80.81828755692798438 ) ) ;
#8985 = CARTESIAN_POINT ( 'NONE',  ( 85.00000000000029843, 17.00000000000000000, -60.00000000000000000 ) ) ;
#8986 = VERTEX_POINT ( 'NONE', #49432 ) ;
#8987 = AXIS2_PLACEMENT_3D ( 'NONE', #29225, #47662, #4849 ) ;
#8988 = CARTESIAN_POINT ( 'NONE',  ( -0.3862712429686809279, -1.188820645368943163, 3.333333333333333481 ) ) ;
#8989 = AXIS2_PLACEMENT_3D ( 'NONE', #12054, #11290, #31566 ) ;
#8990 = CARTESIAN_POINT ( 'NONE',  ( 33.30402655318503946, 0.000000000000000000, 165.0000000000000000 ) ) ;
#8991 = LINE ( 'NONE', #35453, #46678 ) ;
#8992 = DIRECTION ( 'NONE',  ( 0.000000000000000000, 0.000000000000000000, 1.000000000000000000 ) ) ;
#8993 = AXIS2_PLACEMENT_3D ( 'NONE', #50356, #15270, #18833 ) ;
#8994 = ADVANCED_FACE ( 'NONE', ( #14319 ), #26045, .T. ) ;
#8995 = ORIENTED_EDGE ( 'NONE', *, *, #3857, .F. ) ;
#8996 = CARTESIAN_POINT ( 'NONE',  ( -4.945973446814903696, 2.143131898507912917E-16, -40.93171244307205825 ) ) ;
#8997 = LINE ( 'NONE', #24653, #41452 ) ;
#8998 = CARTESIAN_POINT ( 'NONE',  ( -12.97493236725075683, 11.05939663307000664, 8.953103998512858652 ) ) ;
#8999 = PRODUCT_RELATED_PRODUCT_CATEGORY ( 'part', '', ( #1545 ) ) ;
#9000 = ORIENTED_EDGE ( 'NONE', *, *, #32402, .T. ) ;
#9001 = ORIENTED_EDGE ( 'NONE', *, *, #21786, .T. ) ;
#9002 = CONTEXT_DEPENDENT_SHAPE_REPRESENTATION ( #3033, #50717 ) ;
#9004 = CARTESIAN_POINT ( 'NONE',  ( 210.0000000000000568, 0.000000000000000000, -39.18171244307202983 ) ) ;
#9003 = AXIS2_PLACEMENT_3D ( 'NONE', #31247, #43526, #30993 ) ;
#9005 = FACE_OUTER_BOUND ( 'NONE', #29151, .T. ) ;
#9006 = CARTESIAN_POINT ( 'NONE',  ( 111.5540265531850679, 0.000000000000000000, 165.0000000000000000 ) ) ;
#9007 = CARTESIAN_POINT ( 'NONE',  ( 169.0000000000000000, 2.775557561562891351E-14, -99.00000000000014211 ) ) ;
#9008 = VERTEX_POINT ( 'NONE', #22526 ) ;
#9009 = LINE ( 'NONE', #36222, #4271 ) ;
#9010 = EDGE_CURVE ( 'NONE', #13545, #6749, #15351, .T. ) ;
#9011 = CARTESIAN_POINT ( 'NONE',  ( 360.0000000000000000, -166.6568542494925396, -341.6568542494927101 ) ) ;
#9012 = CARTESIAN_POINT ( 'NONE',  ( -178.1763882397827672, -62.49999999999998579, -120.5992382549688529 ) ) ;
#9013 = CARTESIAN_POINT ( 'NONE',  ( 35.00000000000122213, 16.00000000000000000, 5.000000000000004441 ) ) ;
#9014 = ORIENTED_EDGE ( 'NONE', *, *, #19160, .F. ) ;
#9015 = FACE_OUTER_BOUND ( 'NONE', #26441, .T. ) ;
#9016 = ORIENTED_EDGE ( 'NONE', *, *, #11598, .T. ) ;
#9017 = DIRECTION ( 'NONE',  ( -4.758098676964957447E-16, -1.000000000000000000, 7.143884938411937192E-48 ) ) ;
#9018 = ORIENTED_EDGE ( 'NONE', *, *, #36200, .F. ) ;
#9019 = CARTESIAN_POINT ( 'NONE',  ( 350.0000000000000000, -182.9999999999999716, -356.0000000000002274 ) ) ;
#9020 = DIRECTION ( 'NONE',  ( 0.000000000000000000, -1.000000000000000000, 0.000000000000000000 ) ) ;
#9021 = CARTESIAN_POINT ( 'NONE',  ( 350.0000000000000000, 181.0000000000000284, -360.0000000000002274 ) ) ;
#9022 = VECTOR ( 'NONE', #9407, 1000.000000000000000 ) ;
#9023 = ORIENTED_EDGE ( 'NONE', *, *, #29806, .T. ) ;
#9024 = VECTOR ( 'NONE', #29222, 1000.000000000000000 ) ;
#9025 = EDGE_CURVE ( 'NONE', #42729, #3038, #10721, .T. ) ;
#9026 = VECTOR ( 'NONE', #32442, 1000.000000000000000 ) ;
#9027 = CARTESIAN_POINT ( 'NONE',  ( -5.781580041793970004, 8.177378108131215129, 3.215106848023555397 ) ) ;
#9028 = EDGE_CURVE ( 'NONE', #16183, #21718, #24447, .T. ) ;
#9029 = VERTEX_POINT ( 'NONE', #18918 ) ;
#9030 = DIRECTION ( 'NONE',  ( -0.000000000000000000, -1.000000000000000000, -0.000000000000000000 ) ) ;
#9031 = CARTESIAN_POINT ( 'NONE',  ( 31.55402655318503236, -1.025126265847089657, 42.56828755692799149 ) ) ;
#9032 =( BOUNDED_CURVE ( )  B_SPLINE_CURVE ( 3, ( #34397, #49485, #30538, #11034 ),
 .UNSPECIFIED., .F., .F. ) 
 B_SPLINE_CURVE_WITH_KNOTS ( ( 4, 4 ),
 ( 3.141592653589793116, 4.712388980384689674 ),
 .UNSPECIFIED. ) 
 CURVE ( )  GEOMETRIC_REPRESENTATION_ITEM ( )  RATIONAL_B_SPLINE_CURVE ( ( 1.000000000000000000, 0.8047378541243649375, 0.8047378541243649375, 1.000000000000000000 ) ) 
 REPRESENTATION_ITEM ( '' )  );
#9033 = DIRECTION ( 'NONE',  ( -1.542934785277601468E-15, -0.9749645535258959494, 0.2223603367690620558 ) ) ;
#9034 = PLANE ( 'NONE',  #32404 ) ;
#9035 = CARTESIAN_POINT ( 'NONE',  ( 31.28234235046230793, 11.28615439405779064, -3.760136334089591248 ) ) ;
#9036 = VECTOR ( 'NONE', #484, 1000.000000000000114 ) ;
#9037 = EDGE_LOOP ( 'NONE', ( #25071, #39852, #6769, #38512 ) ) ;
#9038 = EDGE_CURVE ( 'NONE', #28813, #31501, #34593, .T. ) ;
#9039 = VERTEX_POINT ( 'NONE', #646 ) ;
#9040 = CARTESIAN_POINT ( 'NONE',  ( 14.49999999999999822, 12.98684210526315930, -19.87312575500900280 ) ) ;
#9041 = EDGE_CURVE ( 'NONE', #20654, #43794, #16295, .T. ) ;
#9042 = EDGE_CURVE ( 'NONE', #9839, #835, #47300, .T. ) ;
#9043 = CIRCLE ( 'NONE', #6543, 1.880036658038868991 ) ;
#9044 = ORIENTED_EDGE ( 'NONE', *, *, #16272, .T. ) ;
#9045 = CARTESIAN_POINT ( 'NONE',  ( 1.019713130072856355, 3.848720492505100843, 4.370690007832189750E-16 ) ) ;
#9046 = CARTESIAN_POINT ( 'NONE',  ( 183.0000000000000000, -256.5000000000000568, -114.9999999999999574 ) ) ;
#9047 = DIRECTION ( 'NONE',  ( -1.000000000000000000, 0.000000000000000000, -1.612977847700450206E-50 ) ) ;
#9048 = ORIENTED_EDGE ( 'NONE', *, *, #38680, .T. ) ;
#9049 = CARTESIAN_POINT ( 'NONE',  ( 130.0000000000015064, 17.00000000000000000, 35.00000000000000000 ) ) ;
#9050 = EDGE_CURVE ( 'NONE', #47864, #5399, #7141, .T. ) ;
#9051 = DIRECTION ( 'NONE',  ( -0.000000000000000000, -0.000000000000000000, -1.000000000000000000 ) ) ;
#9052 = FACE_OUTER_BOUND ( 'NONE', #18429, .T. ) ;
#9053 = DIRECTION ( 'NONE',  ( -1.000000000000000000, -0.000000000000000000, -0.000000000000000000 ) ) ;
#9054 = DIRECTION ( 'NONE',  ( -0.000000000000000000, -1.000000000000000000, -0.000000000000000000 ) ) ;
#9055 = CARTESIAN_POINT ( 'NONE',  ( 356.0000000000000000, -169.0000000000001137, -349.9999999999999432 ) ) ;
#9056 = ORIENTED_EDGE ( 'NONE', *, *, #2878, .T. ) ;
#9057 = ORIENTED_EDGE ( 'NONE', *, *, #4527, .T. ) ;
#9058 = EDGE_LOOP ( 'NONE', ( #13653, #11756, #9966, #7204 ) ) ;
#9059 = CARTESIAN_POINT ( 'NONE',  ( -42.99990394833793061, 47.95759300784327905, -5.000000000000000000 ) ) ;
#9060 = CARTESIAN_POINT ( 'NONE',  ( 167.4999999999999716, 102.9547873477646647, -7.018571579996165433 ) ) ;
#9061 = CARTESIAN_POINT ( 'NONE',  ( 135.0000000000000000, 16.00000000000000000, -114.9999999999999858 ) ) ;
#9062 = CARTESIAN_POINT ( 'NONE',  ( -164.9459734468149463, 2.143131898507880377E-16, 79.06828755692797017 ) ) ;
#9063 = VERTEX_POINT ( 'NONE', #3019 ) ;
#9064 = LINE ( 'NONE', #32163, #17650 ) ;
#9065 = ORIENTED_EDGE ( 'NONE', *, *, #2594, .T. ) ;
#9066 = DIRECTION ( 'NONE',  ( -0.000000000000000000, -1.000000000000000000, -0.000000000000000000 ) ) ;
#9067 = CARTESIAN_POINT ( 'NONE',  ( 35.05402655318503946, 0.000000000000000000, 162.5682875569279702 ) ) ;
#9068 = FACE_OUTER_BOUND ( 'NONE', #43190, .T. ) ;
#9069 = AXIS2_PLACEMENT_3D ( 'NONE', #47158, #3839, #7958 ) ;
#9070 = FACE_OUTER_BOUND ( 'NONE', #42932, .T. ) ;
#9071 = CARTESIAN_POINT ( 'NONE',  ( 167.0000000000000000, 2.775557561562891351E-14, -99.00000000000014211 ) ) ;
#9072 = DIRECTION ( 'NONE',  ( 1.000000000000000000, -4.996003610813203446E-16, -7.930164450086814785E-16 ) ) ;
#9073 = ORIENTED_EDGE ( 'NONE', *, *, #42945, .T. ) ;
#9074 = CARTESIAN_POINT ( 'NONE',  ( -206.6959734468149463, -1.750000000000009992, 160.8182875569279702 ) ) ;
#9075 = VECTOR ( 'NONE', #40164, 1000.000000000000000 ) ;
#9077 = CIRCLE ( 'NONE', #38573, 3.749999999999975575 ) ;
#9076 = DIRECTION ( 'NONE',  ( 0.000000000000000000, 0.000000000000000000, 1.000000000000000000 ) ) ;
#9078 = CARTESIAN_POINT ( 'NONE',  ( 356.0000000000000000, 165.0000000000000000, -108.0000000000002132 ) ) ;
#9079 = EDGE_CURVE ( 'NONE', #39109, #20342, #38701, .T. ) ;
#9080 = FILL_AREA_STYLE ('',( #48025 ) ) ;
#9081 = VERTEX_POINT ( 'NONE', #39652 ) ;
#9082 = FACE_OUTER_BOUND ( 'NONE', #42973, .T. ) ;
#9083 = VERTEX_POINT ( 'NONE', #22780 ) ;
#9084 = CARTESIAN_POINT ( 'NONE',  ( 1.841192853132477492, 1.035021892307843583, 9.890170120223997330 ) ) ;
#9085 = CARTESIAN_POINT ( 'NONE',  ( -9.998889670239194061, -0.1490146381531308739, 9.282506307616474217 ) ) ;
#9086 = VERTEX_POINT ( 'NONE', #34340 ) ;
#9087 = EDGE_LOOP ( 'NONE', ( #15471, #43522 ) ) ;
#9088 =( BOUNDED_CURVE ( )  B_SPLINE_CURVE ( 3, ( #38924, #928, #8120, #12207 ),
 .UNSPECIFIED., .F., .F. ) 
 B_SPLINE_CURVE_WITH_KNOTS ( ( 4, 4 ),
 ( 0.000000000000000000, 1.570796326794896558 ),
 .UNSPECIFIED. ) 
 CURVE ( )  GEOMETRIC_REPRESENTATION_ITEM ( )  RATIONAL_B_SPLINE_CURVE ( ( 1.000000000000000000, 0.8047378541243649375, 0.8047378541243649375, 1.000000000000000000 ) ) 
 REPRESENTATION_ITEM ( '' )  );
#9089 = EDGE_CURVE ( 'NONE', #921, #33108, #18667, .T. ) ;
#9090 = PLANE ( 'NONE',  #33641 ) ;
#9091 = DIRECTION ( 'NONE',  ( 1.000000000000000000, 0.000000000000000000, -0.000000000000000000 ) ) ;
#9092 = CARTESIAN_POINT ( 'NONE',  ( -44.99506233596264337, -23.32283626942287214, 7.455576670931136185 ) ) ;
#9093 = FACE_OUTER_BOUND ( 'NONE', #32831, .T. ) ;
#9094 =( BOUNDED_CURVE ( )  B_SPLINE_CURVE ( 3, ( #18467, #15129, #2563, #10768 ),
 .UNSPECIFIED., .F., .F. ) 
 B_SPLINE_CURVE_WITH_KNOTS ( ( 4, 4 ),
 ( 1.570796326794896558, 3.141592653589793116 ),
 .UNSPECIFIED. ) 
 CURVE ( )  GEOMETRIC_REPRESENTATION_ITEM ( )  RATIONAL_B_SPLINE_CURVE ( ( 1.000000000000000000, 0.8047378541243649375, 0.8047378541243649375, 1.000000000000000000 ) ) 
 REPRESENTATION_ITEM ( '' )  );
#9095 = ORIENTED_EDGE ( 'NONE', *, *, #26122, .F. ) ;
#9096 = VERTEX_POINT ( 'NONE', #30749 ) ;
#9097 = FACE_OUTER_BOUND ( 'NONE', #2647, .T. ) ;
#9098 = VECTOR ( 'NONE', #25248, 1000.000000000000000 ) ;
#9099 = EDGE_CURVE ( 'NONE', #40964, #19479, #37659, .T. ) ;
#9100 = EDGE_CURVE ( 'NONE', #576, #5426, #31909, .T. ) ;
#9101 = AXIS2_PLACEMENT_3D ( 'NONE', #48542, #21637, #16788 ) ;
#9102 = ORIENTED_EDGE ( 'NONE', *, *, #33479, .F. ) ;
#9103 = ORIENTED_EDGE ( 'NONE', *, *, #33702, .F. ) ;
#9104 = DIRECTION ( 'NONE',  ( 0.000000000000000000, 0.000000000000000000, 1.000000000000000000 ) ) ;
#9105 = DIRECTION ( 'NONE',  ( -0.000000000000000000, -1.000000000000000000, -0.000000000000000000 ) ) ;
#9106 = CARTESIAN_POINT ( 'NONE',  ( -0.1287570809895658697, 0.3962735484563123523, 10.00000000000000000 ) ) ;
#9107 = CARTESIAN_POINT ( 'NONE',  ( 358.3431457505075741, 185.0000000000000568, 359.9999999999998295 ) ) ;
#9108 = ORIENTED_EDGE ( 'NONE', *, *, #3916, .F. ) ;
#9109 = ORIENTED_EDGE ( 'NONE', *, *, #13729, .T. ) ;
#9110 = EDGE_CURVE ( 'NONE', #44276, #10712, #27848, .T. ) ;
#9111 = ORIENTED_EDGE ( 'NONE', *, *, #23050, .T. ) ;
#9112 = AXIS2_PLACEMENT_3D ( 'NONE', #41445, #6037, #37378 ) ;
#9113 = CARTESIAN_POINT ( 'NONE',  ( -33.64889274059387958, 3.704246042440976439, 8.356839323120299312 ) ) ;
#9114 = CARTESIAN_POINT ( 'NONE',  ( 1.011271242968683648, 0.7347315653655930312, -3.333333333333333481 ) ) ;
#9115 = ORIENTED_EDGE ( 'NONE', *, *, #3523, .T. ) ;
#9116 = ORIENTED_EDGE ( 'NONE', *, *, #17628, .F. ) ;
#9117 = CARTESIAN_POINT ( 'NONE',  ( 14.52758583651987223, 8.922352469211173087, 8.953103998512858652 ) ) ;
#9118 = VERTEX_POINT ( 'NONE', #42284 ) ;
#9119 = VERTEX_POINT ( 'NONE', #23995 ) ;
#9120 = DIRECTION ( 'NONE',  ( 0.000000000000000000, 0.000000000000000000, 1.000000000000000000 ) ) ;
#9121 = CARTESIAN_POINT ( 'NONE',  ( 130.0000000000015064, 17.00000000000000000, 60.00000000000000000 ) ) ;
#9122 = EDGE_LOOP ( 'NONE', ( #12637, #17179 ) ) ;
#9123 = CARTESIAN_POINT ( 'NONE',  ( 210.0000000000000568, 2.143131898507881856E-16, 119.0682875569279560 ) ) ;
#9124 = PLANE ( 'NONE',  #27676 ) ;
#9125 = CARTESIAN_POINT ( 'NONE',  ( 154.3291528190321458, 1.750000000000009548, -158.1565861772249377 ) ) ;
#9126 = CARTESIAN_POINT ( 'NONE',  ( 191.5540265531851105, 0.000000000000000000, 165.0000000000000000 ) ) ;
#9127 = VERTEX_POINT ( 'NONE', #30483 ) ;
#9128 = CARTESIAN_POINT ( 'NONE',  ( 130.0000000000005684, 17.00000000000000000, -54.99999999999999289 ) ) ;
#9129 = CARTESIAN_POINT ( 'NONE',  ( 33.01266944765062306, -5.813986777101467496, 1.847720168420772691 ) ) ;
#9130 = DIRECTION ( 'NONE',  ( -0.000000000000000000, 1.000000000000000000, 1.224646799147353207E-16 ) ) ;
#9131 = CARTESIAN_POINT ( 'NONE',  ( -34.91952936320829792, 13.67027684621028349, -9.422646554964178023 ) ) ;
#9132 = EDGE_CURVE ( 'NONE', #9194, #24608, #11027, .T. ) ;
#9133 = AXIS2_PLACEMENT_3D ( 'NONE', #989, #32297, #8931 ) ;
#9134 = CARTESIAN_POINT ( 'NONE',  ( 185.0000000000000000, -174.9999999999999716, -344.0000000000001137 ) ) ;
#9135 = DIRECTION ( 'NONE',  ( -1.000000000000000000, -0.000000000000000000, -0.000000000000000000 ) ) ;
#9136 = FACE_OUTER_BOUND ( 'NONE', #16855, .T. ) ;
#9137 = CARTESIAN_POINT ( 'NONE',  ( -44.94597344681493922, -1.025126265847089657, 79.06828755692797017 ) ) ;
#9138 = ORIENTED_EDGE ( 'NONE', *, *, #4842, .F. ) ;
#9139 = CARTESIAN_POINT ( 'NONE',  ( -23.82716369509181575, -44.49195112875988656, 8.356839323120299312 ) ) ;
#9140 = CARTESIAN_POINT ( 'NONE',  ( 0.3522231071503528765, -1.258647432227843588, 9.945465957785078359 ) ) ;
#9141 = ORIENTED_EDGE ( 'NONE', *, *, #28449, .F. ) ;
#9142 = CARTESIAN_POINT ( 'NONE',  ( -4.641001526964561030, -50.00000000000000000, -8.016098858316205167 ) ) ;
#9143 = PLANE ( 'NONE',  #35510 ) ;
#9144 = CARTESIAN_POINT ( 'NONE',  ( -86.69597344681494633, -1.750000000000010658, 80.81828755692798438 ) ) ;
#9145 = ORIENTED_EDGE ( 'NONE', *, *, #14539, .F. ) ;
#9146 = CARTESIAN_POINT ( 'NONE',  ( -208.4459734468149463, 0.000000000000000000, 2.568287556927978166 ) ) ;
#9147 = VERTEX_POINT ( 'NONE', #42027 ) ;
#9148 = CYLINDRICAL_SURFACE ( 'NONE', #32474, 1.750000000000010214 ) ;
#9149 = CARTESIAN_POINT ( 'NONE',  ( 358.0000000000001137, 180.9999999999999716, 355.9999999999997726 ) ) ;
#9150 = ORIENTED_EDGE ( 'NONE', *, *, #43382, .T. ) ;
#9151 = CARTESIAN_POINT ( 'NONE',  ( -206.6959734468149463, 0.000000000000000000, 165.0000000000000000 ) ) ;
#9152 = DIRECTION ( 'NONE',  ( -1.000000000000000000, 0.000000000000000000, 0.000000000000000000 ) ) ;
#9153 = VERTEX_POINT ( 'NONE', #6030 ) ;
#9154 = ORIENTED_EDGE ( 'NONE', *, *, #48665, .F. ) ;
#9155 = EDGE_CURVE ( 'NONE', #16392, #17311, #563, .T. ) ;
#9156 = VECTOR ( 'NONE', #7177, 1000.000000000000000 ) ;
#9157 = DIRECTION ( 'NONE',  ( 1.000000000000000000, -7.930164457481157120E-16, 1.587271980518778491E-16 ) ) ;
#9158 = ORIENTED_EDGE ( 'NONE', *, *, #306, .F. ) ;
#9159 = LINE ( 'NONE', #1967, #44610 ) ;
#9160 = CARTESIAN_POINT ( 'NONE',  ( -17.34922095635781147, -33.24536858281880569, 8.914903342594564961 ) ) ;
#9161 = LINE ( 'NONE', #33031, #12812 ) ;
#9162 = VERTEX_POINT ( 'NONE', #48844 ) ;
#9163 = DIRECTION ( 'NONE',  ( 1.000000000000000000, 0.000000000000000000, 0.000000000000000000 ) ) ;
#9164 = AXIS2_PLACEMENT_3D ( 'NONE', #15191, #30853, #30334 ) ;
#9165 = CARTESIAN_POINT ( 'NONE',  ( 1.011271242968694084, -0.7347315653655782652, 10.00000000000000000 ) ) ;
#9166 = VERTEX_POINT ( 'NONE', #44767 ) ;
#9167 = ORIENTED_EDGE ( 'NONE', *, *, #10781, .F. ) ;
#9168 = ORIENTED_EDGE ( 'NONE', *, *, #35375, .T. ) ;
#9169 = DIRECTION ( 'NONE',  ( 1.000000000000000000, 0.000000000000000000, -0.000000000000000000 ) ) ;
#9170 = ADVANCED_FACE ( 'NONE', ( #37114 ), #1942, .F. ) ;
#9171 = LINE ( 'NONE', #48125, #31594 ) ;
#9172 = ORIENTED_EDGE ( 'NONE', *, *, #41912, .T. ) ;
#9173 = ADVANCED_FACE ( 'NONE', ( #34008 ), #6796, .T. ) ;
#9174 = CARTESIAN_POINT ( 'NONE',  ( 0.9599924130074096729, -0.8495346730527926216, 9.948547179989617462 ) ) ;
#9175 = CARTESIAN_POINT ( 'NONE',  ( 35.00000000000186162, 17.00000000000000000, 65.00000000000000000 ) ) ;
#9176 = CARTESIAN_POINT ( 'NONE',  ( -128.4459734468149179, 0.000000000000000000, 159.0682875569279986 ) ) ;
#9177 = DIRECTION ( 'NONE',  ( 0.000000000000000000, 0.000000000000000000, 1.000000000000000000 ) ) ;
#9178 = CARTESIAN_POINT ( 'NONE',  ( -175.0000000000000000, 0.000000000000000000, -122.5000000000000000 ) ) ;
#9179 = CARTESIAN_POINT ( 'NONE',  ( 0.000000000000000000, 165.2000000000000171, -359.8000000000002387 ) ) ;
#9180 = CARTESIAN_POINT ( 'NONE',  ( 33.30402655318503946, 1.750000000000010214, 40.81828755692798438 ) ) ;
#9181 = FACE_OUTER_BOUND ( 'NONE', #40669, .T. ) ;
#9182 = EDGE_CURVE ( 'NONE', #5824, #26840, #26050, .T. ) ;
#9183 = CARTESIAN_POINT ( 'NONE',  ( 130.0000000000005684, 17.00000000000000000, -54.99999999999999289 ) ) ;
#9184 = CARTESIAN_POINT ( 'NONE',  ( -42.99990394833793061, 47.95759300784327905, 5.000000000000000000 ) ) ;
#9185 = EDGE_CURVE ( 'NONE', #18651, #22117, #6545, .T. ) ;
#9186 = CARTESIAN_POINT ( 'NONE',  ( 115.0540265531850679, 0.000000000000000000, 162.5682875569279702 ) ) ;
#9187 = VECTOR ( 'NONE', #2182, 1000.000000000000000 ) ;
#9188 = VERTEX_POINT ( 'NONE', #3639 ) ;
#9189 = CARTESIAN_POINT ( 'NONE',  ( -44.94597344681493922, 2.143131898507880377E-16, -0.9317124430720247208 ) ) ;
#9190 = VECTOR ( 'NONE', #44606, 1000.000000000000000 ) ;
#9191 = CARTESIAN_POINT ( 'NONE',  ( 185.0000000000000000, -268.4999999999999432, -349.9999999999999432 ) ) ;
#9192 = DIRECTION ( 'NONE',  ( -1.000000000000000000, -0.000000000000000000, -0.000000000000000000 ) ) ;
#9193 = CARTESIAN_POINT ( 'NONE',  ( 232.4999999999999716, -169.9999999999999716, 32.29650858650035161 ) ) ;
#9194 = VERTEX_POINT ( 'NONE', #41441 ) ;
#9195 = DIRECTION ( 'NONE',  ( -1.224646799147352468E-16, 0.000000000000000000, -1.000000000000000000 ) ) ;
#9196 = AXIS2_PLACEMENT_3D ( 'NONE', #1536, #40780, #21028 ) ;
#9197 = CARTESIAN_POINT ( 'NONE',  ( -127.7210997126620242, -1.749999999999996669, 39.79316129108089228 ) ) ;
#9198 = ORIENTED_EDGE ( 'NONE', *, *, #16194, .F. ) ;
#9199 = CARTESIAN_POINT ( 'NONE',  ( 168.9999999999999716, -164.9999999999999432, -360.0000000000002274 ) ) ;
#9200 = DIRECTION ( 'NONE',  ( 0.000000000000000000, 1.000000000000000000, 4.687818848539279227E-49 ) ) ;
#9201 = CARTESIAN_POINT ( 'NONE',  ( -127.7210997126620242, 1.749999999999996669, 159.7931612910809065 ) ) ;
#9202 = EDGE_LOOP ( 'NONE', ( #25961, #12881, #32664, #49823 ) ) ;
#9203 = CARTESIAN_POINT ( 'NONE',  ( 32.27890028733795447, -1.750000000000010214, -118.1565861772249519 ) ) ;
#9204 = B_SPLINE_SURFACE_WITH_KNOTS ( 'NONE', 3, 3, ( 
 ( #41583, #456, #4039, #39964 ),
 ( #16097, #47095, #47856, #4300 ),
 ( #27652, #23549, #8152, #43284 ),
 ( #4786, #19691, #11998, #3075 ) ),
 .UNSPECIFIED., .F., .F., .F.,
 ( 4, 4 ),
 ( 4, 4 ),
 ( 0.000000000000000000, 1.000000000000000000 ),
 ( 0.000000000000000000, 1.000000000000000000 ),
 .UNSPECIFIED. ) ;
#9205 = EDGE_CURVE ( 'NONE', #44495, #920, #21509, .T. ) ;
#9206 = VERTEX_POINT ( 'NONE', #19284 ) ;
#9207 = VERTEX_POINT ( 'NONE', #41948 ) ;
#9208 = EDGE_CURVE ( 'NONE', #45429, #47093, #9639, .T. ) ;
#9209 = EDGE_CURVE ( 'NONE', #15492, #38770, #29639, .T. ) ;
#9210 = ORIENTED_EDGE ( 'NONE', *, *, #25817, .T. ) ;
#9211 = SPHERICAL_SURFACE ( 'NONE', #29493, 0.5000000000000000000 ) ;
#9212 = CARTESIAN_POINT ( 'NONE',  ( -6.508636631827791064, -15.75743548351446854, 8.953103998512858652 ) ) ;
#9213 = VERTEX_POINT ( 'NONE', #13733 ) ;
#9214 = PLANE ( 'NONE',  #41805 ) ;
#9215 = DIRECTION ( 'NONE',  ( -0.000000000000000000, -1.000000000000000000, -0.000000000000000000 ) ) ;
#9216 = EDGE_CURVE ( 'NONE', #4735, #20088, #10137, .T. ) ;
#9217 = DIRECTION ( 'NONE',  ( 0.000000000000000000, 0.000000000000000000, 1.000000000000000000 ) ) ;
#9218 = AXIS2_PLACEMENT_3D ( 'NONE', #3021, #26382, #46786 ) ;
#9219 = ORIENTED_EDGE ( 'NONE', *, *, #14281, .F. ) ;
#9220 = ADVANCED_FACE ( 'NONE', ( #49094 ), #40899, .T. ) ;
#9221 = CARTESIAN_POINT ( 'NONE',  ( -194.9999999999999432, -173.0000000000000000, 352.0000000000000568 ) ) ;
#9222 =( BOUNDED_CURVE ( )  B_SPLINE_CURVE ( 3, ( #8764, #16689, #28507, #8508 ),
 .UNSPECIFIED., .F., .F. ) 
 B_SPLINE_CURVE_WITH_KNOTS ( ( 4, 4 ),
 ( 0.000000000000000000, 1.570796326794896558 ),
 .UNSPECIFIED. ) 
 CURVE ( )  GEOMETRIC_REPRESENTATION_ITEM ( )  RATIONAL_B_SPLINE_CURVE ( ( 1.000000000000000000, 0.8047378541243649375, 0.8047378541243649375, 1.000000000000000000 ) ) 
 REPRESENTATION_ITEM ( '' )  );
#9223 = VERTEX_POINT ( 'NONE', #25540 ) ;
#9224 = DIRECTION ( 'NONE',  ( -0.000000000000000000, -1.000000000000000000, 2.537652627714643577E-15 ) ) ;
#9225 = LINE ( 'NONE', #17432, #32692 ) ;
#9226 = ORIENTED_EDGE ( 'NONE', *, *, #26386, .T. ) ;
#9227 = VECTOR ( 'NONE', #14477, 1000.000000000000000 ) ;
#9228 = EDGE_LOOP ( 'NONE', ( #40039, #10659, #18039, #29670 ) ) ;
#9229 = ORIENTED_EDGE ( 'NONE', *, *, #47227, .F. ) ;
#9230 = DIRECTION ( 'NONE',  ( -0.000000000000000000, -0.000000000000000000, -1.000000000000000000 ) ) ;
#9231 = AXIS2_PLACEMENT_3D ( 'NONE', #18812, #42171, #46493 ) ;
#9232 = CARTESIAN_POINT ( 'NONE',  ( -114.9999999999991047, 17.00000000000000000, -24.99999999999999289 ) ) ;
#9233 = VERTEX_POINT ( 'NONE', #49345 ) ;
#9234 = AXIS2_PLACEMENT_3D ( 'NONE', #6930, #26177, #34646 ) ;
#9235 = LINE ( 'NONE', #13588, #25757 ) ;
#9236 = FILL_AREA_STYLE ('',( #44366 ) ) ;
#9237 = LINE ( 'NONE', #37228, #38691 ) ;
#9238 = VECTOR ( 'NONE', #43633, 1000.000000000000000 ) ;
#9239 = VERTEX_POINT ( 'NONE', #29388 ) ;
#9240 = CARTESIAN_POINT ( 'NONE',  ( -46.69597344681494633, 1.750000000000010658, 120.8182875569279702 ) ) ;
#9241 = CARTESIAN_POINT ( 'NONE',  ( 168.9999999999999716, 8.000000000000062172, 339.9999999999998295 ) ) ;
#9242 =( BOUNDED_CURVE ( )  B_SPLINE_CURVE ( 3, ( #27246, #8007, #39061, #46694 ),
 .UNSPECIFIED., .F., .F. ) 
 B_SPLINE_CURVE_WITH_KNOTS ( ( 4, 4 ),
 ( 3.141592653589793116, 4.712388980384689674 ),
 .UNSPECIFIED. ) 
 CURVE ( )  GEOMETRIC_REPRESENTATION_ITEM ( )  RATIONAL_B_SPLINE_CURVE ( ( 1.000000000000000000, 0.8047378541243649375, 0.8047378541243649375, 1.000000000000000000 ) ) 
 REPRESENTATION_ITEM ( '' )  );
#9243 = LINE ( 'NONE', #41555, #38767 ) ;
#9244 = EDGE_CURVE ( 'NONE', #28645, #41417, #21683, .T. ) ;
#9245 = ORIENTED_EDGE ( 'NONE', *, *, #22385, .T. ) ;
#9246 = ADVANCED_FACE ( 'NONE', ( #13977 ), #45258, .T. ) ;
#9247 = ORIENTED_EDGE ( 'NONE', *, *, #25155, .T. ) ;
#9248 = APPLICATION_PROTOCOL_DEFINITION ( 'draft international standard', 'automotive_design', 1998, #37166 ) ;
#9249 = CARTESIAN_POINT ( 'NONE',  ( -88.44597344681497475, 0.000000000000000000, 82.56828755692801280 ) ) ;
#9250 = EDGE_CURVE ( 'NONE', #18218, #12217, #29343, .T. ) ;
#9251 = EDGE_CURVE ( 'NONE', #43110, #12379, #46716, .T. ) ;
#9252 = B_SPLINE_CURVE_WITH_KNOTS ( 'NONE', 3,
 ( #10639, #34007, #26049, #5785 ),
 .UNSPECIFIED., .F., .F.,
 ( 4, 4 ),
 ( 0.000000000000000000, 0.009762429722931321996 ),
 .UNSPECIFIED. ) ;
#9253 = AXIS2_PLACEMENT_3D ( 'NONE', #40798, #17448, #33119 ) ;
#9254 = CARTESIAN_POINT ( 'NONE',  ( -14.76429217231967428, -8.192625680377590314, 9.178419661560148768 ) ) ;
#9255 = FACE_OUTER_BOUND ( 'NONE', #28715, .T. ) ;
#9256 = VERTEX_POINT ( 'NONE', #39331 ) ;
#9257 = ADVANCED_FACE ( 'NONE', ( #3387 ), #8277, .T. ) ;
#9258 = CARTESIAN_POINT ( 'NONE',  ( -69.99999999999909051, 16.00000000000000000, -24.99999999999999289 ) ) ;
#9259 = ADVANCED_FACE ( 'NONE', ( #38826 ), #43164, .F. ) ;
#9260 = CARTESIAN_POINT ( 'NONE',  ( -15.44803555374685189, -6.237487519713257100, -3.546734833711462365 ) ) ;
#9261 = CARTESIAN_POINT ( 'NONE',  ( -128.4459734468149179, 0.000000000000000000, 122.5682875569279418 ) ) ;
#9262 = DIRECTION ( 'NONE',  ( 0.000000000000000000, 1.000000000000000000, 3.186989995019654210E-49 ) ) ;
#9263 = VERTEX_POINT ( 'NONE', #23418 ) ;
#9264 = CARTESIAN_POINT ( 'NONE',  ( 0.02889939370645888336, -1.394750214494760110, 9.955131761384823363 ) ) ;
#9265 = ORIENTED_EDGE ( 'NONE', *, *, #486, .T. ) ;
#9266 = B_SPLINE_CURVE_WITH_KNOTS ( 'NONE', 3,
 ( #33570, #26102, #14301, #26368 ),
 .UNSPECIFIED., .F., .F.,
 ( 4, 4 ),
 ( 0.001403500796105015260, 0.001586656765099030012 ),
 .UNSPECIFIED. ) ;
#9267 = CARTESIAN_POINT ( 'NONE',  ( -208.4459734468148611, -1.025126265847089657, -37.43171244307202272 ) ) ;
#9268 = CIRCLE ( 'NONE', #28932, 0.5000000000000004441 ) ;
#9269 = VERTEX_POINT ( 'NONE', #7776 ) ;
#9270 = CARTESIAN_POINT ( 'NONE',  ( -204.9459734468149463, 2.143131898507880377E-16, 159.0682875569279702 ) ) ;
#9271 = AXIS2_PLACEMENT_3D ( 'NONE', #31293, #495, #24353 ) ;
#9272 = DIRECTION ( 'NONE',  ( 0.000000000000000000, 0.000000000000000000, -1.000000000000000000 ) ) ;
#9273 = EDGE_CURVE ( 'NONE', #43883, #22983, #23915, .T. ) ;
#9274 = ORIENTED_EDGE ( 'NONE', *, *, #24265, .F. ) ;
#9275 = AXIS2_PLACEMENT_3D ( 'NONE', #14499, #49100, #23414 ) ;
#9276 = EDGE_CURVE ( 'NONE', #26090, #7778, #4419, .T. ) ;
#9277 = CARTESIAN_POINT ( 'NONE',  ( 0.6108107228405675881, -1.056024183042613140, 9.963925895596188909 ) ) ;
#9278 = ADVANCED_FACE ( 'NONE', ( #30607 ), #46207, .T. ) ;
#9279 = ORIENTED_EDGE ( 'NONE', *, *, #49476, .F. ) ;
#9280 = LINE ( 'NONE', #29032, #16381 ) ;
#9281 = CARTESIAN_POINT ( 'NONE',  ( -128.4459734468149179, 0.000000000000000000, 2.568287556927950632 ) ) ;
#9282 = DIRECTION ( 'NONE',  ( -1.000000000000000000, 0.000000000000000000, 0.000000000000000000 ) ) ;
#9283 = CARTESIAN_POINT ( 'NONE',  ( -0.4426377647354682865, -1.666766018367764834, 9.928159647716134018 ) ) ;
#9284 = CARTESIAN_POINT ( 'NONE',  ( 71.55402655318505367, 1.025126265847089435, -40.93171244307204404 ) ) ;
#9285 = ORIENTED_EDGE ( 'NONE', *, *, #16717, .F. ) ;
#9286 = VERTEX_POINT ( 'NONE', #3904 ) ;
#9287 = DIRECTION ( 'NONE',  ( 0.000000000000000000, -2.265761274745217480E-16, 1.000000000000000000 ) ) ;
#9288 = ORIENTED_EDGE ( 'NONE', *, *, #31216, .F. ) ;
#9289 = CARTESIAN_POINT ( 'NONE',  ( 115.0540265531850395, -1.025126265847081664, 82.56828755692798438 ) ) ;
#9290 = DIRECTION ( 'NONE',  ( 1.000000000000000000, 0.000000000000000000, 7.793956916774525800E-48 ) ) ;
#9291 = VERTEX_POINT ( 'NONE', #23662 ) ;
#9292 = CARTESIAN_POINT ( 'NONE',  ( 75.05402655318509630, 2.143131898507873721E-16, -165.0000000000000000 ) ) ;
#9293 = EDGE_CURVE ( 'NONE', #46541, #12229, #26766, .T. ) ;
#9294 = DIRECTION ( 'NONE',  ( -7.793956916774524585E-48, 0.000000000000000000, -1.000000000000000000 ) ) ;
#9295 = FACE_OUTER_BOUND ( 'NONE', #4957, .T. ) ;
#9296 = DIRECTION ( 'NONE',  ( -1.000000000000000000, 0.000000000000000000, -0.000000000000000000 ) ) ;
#9297 = CARTESIAN_POINT ( 'NONE',  ( 356.0000000000001137, 181.0000000000000284, 349.9999999999998863 ) ) ;
#9298 = PLANE ( 'NONE',  #30473 ) ;
#9299 = VERTEX_POINT ( 'NONE', #35231 ) ;
#9300 = ORIENTED_EDGE ( 'NONE', *, *, #26782, .T. ) ;
#9301 = VECTOR ( 'NONE', #272, 1000.000000000000000 ) ;
#9302 = EDGE_CURVE ( 'NONE', #14628, #1211, #26754, .T. ) ;
#9303 = ORIENTED_EDGE ( 'NONE', *, *, #25020, .F. ) ;
#9304 = DIRECTION ( 'NONE',  ( 0.000000000000000000, -1.224646799147353207E-16, 1.000000000000000000 ) ) ;
#9305 = CARTESIAN_POINT ( 'NONE',  ( 47.23269937569327226, -16.43609759007049931, -2.408242355805840784 ) ) ;
#9306 = AXIS2_PLACEMENT_3D ( 'NONE', #20675, #44502, #13728 ) ;
#9307 = CARTESIAN_POINT ( 'NONE',  ( 191.5540265531851105, 0.000000000000000000, 39.06828755692798438 ) ) ;
#9308 = CARTESIAN_POINT ( 'NONE',  ( 350.0000000000000000, -168.9999999999999432, -358.0000000000002274 ) ) ;
#9309 = ORIENTED_EDGE ( 'NONE', *, *, #45252, .F. ) ;
#9310 =( GEOMETRIC_REPRESENTATION_CONTEXT ( 3 ) GLOBAL_UNCERTAINTY_ASSIGNED_CONTEXT ( ( #4002 ) ) GLOBAL_UNIT_ASSIGNED_CONTEXT ( ( #34161, #27203, #11553 ) ) REPRESENTATION_CONTEXT ( 'NONE', 'WORKASPACE' ) );
#9311 = CARTESIAN_POINT ( 'NONE',  ( 359.9999999999999432, 174.9999999999996589, -356.0000000000003411 ) ) ;
#9312 = ORIENTED_EDGE ( 'NONE', *, *, #29658, .F. ) ;
#9313 = CARTESIAN_POINT ( 'NONE',  ( -0.4166666666666664631, 0.000000000000000000, 10.00000000000000000 ) ) ;
#9314 = CARTESIAN_POINT ( 'NONE',  ( -208.4459734468149463, 0.000000000000000000, 2.568287556927978166 ) ) ;
#9315 = CARTESIAN_POINT ( 'NONE',  ( -5.000000000000000000, 0.000000000000000000, 0.000000000000000000 ) ) ;
#9316 = EDGE_CURVE ( 'NONE', #27141, #30805, #42387, .T. ) ;
#9317 = EDGE_CURVE ( 'NONE', #31951, #34191, #15708, .T. ) ;
#9318 = PLANE ( 'NONE',  #11909 ) ;
#9319 = FACE_OUTER_BOUND ( 'NONE', #17798, .T. ) ;
#9320 = DIRECTION ( 'NONE',  ( 0.000000000000000000, 1.000000000000000000, -2.969158215481698263E-48 ) ) ;
#9321 = ORIENTED_EDGE ( 'NONE', *, *, #43183, .F. ) ;
#9322 = DIRECTION ( 'NONE',  ( 0.000000000000000000, 0.000000000000000000, 1.000000000000000000 ) ) ;
#9323 = ADVANCED_FACE ( 'NONE', ( #22896 ), #34986, .F. ) ;
#9324 = PRODUCT ( 'wire', 'wire', '', ( #44619 ) ) ;
#9325 = DIRECTION ( 'NONE',  ( 0.000000000000000000, 0.000000000000000000, -1.000000000000000000 ) ) ;
#9326 = CYLINDRICAL_SURFACE ( 'NONE', #15146, 1.749999999999973799 ) ;
#9327 = EDGE_CURVE ( 'NONE', #11298, #14780, #19299, .T. ) ;
#9328 = ADVANCED_FACE ( 'NONE', ( #15452 ), #15970, .F. ) ;
#9329 = AXIS2_PLACEMENT_3D ( 'NONE', #47753, #23947, #5450 ) ;
#9330 = LINE ( 'NONE', #24986, #29666 ) ;
#9331 = ORIENTED_EDGE ( 'NONE', *, *, #24960, .F. ) ;
#9332 =( BOUNDED_CURVE ( )  B_SPLINE_CURVE ( 3, ( #45329, #22266, #34582, #49911 ),
 .UNSPECIFIED., .F., .F. ) 
 B_SPLINE_CURVE_WITH_KNOTS ( ( 4, 4 ),
 ( 3.141592653589793116, 4.712388980384689674 ),
 .UNSPECIFIED. ) 
 CURVE ( )  GEOMETRIC_REPRESENTATION_ITEM ( )  RATIONAL_B_SPLINE_CURVE ( ( 1.000000000000000000, 0.8047378541243649375, 0.8047378541243649375, 1.000000000000000000 ) ) 
 REPRESENTATION_ITEM ( '' )  );
#9333 = CARTESIAN_POINT ( 'NONE',  ( -69.99999999999783995, 16.00000000000000000, 95.00000000000000000 ) ) ;
#9334 = EDGE_LOOP ( 'NONE', ( #18121, #13690, #6387, #16671 ) ) ;
#9335 = DIRECTION ( 'NONE',  ( -0.000000000000000000, -0.000000000000000000, -1.000000000000000000 ) ) ;
#9336 = CARTESIAN_POINT ( 'NONE',  ( 130.0000000000005684, 16.00000000000000000, -54.99999999999999289 ) ) ;
#9337 = ADVANCED_FACE ( 'NONE', ( #38577 ), #19041, .F. ) ;
#9338 = DIRECTION ( 'NONE',  ( 0.000000000000000000, 0.000000000000000000, -1.000000000000000000 ) ) ;
#9339 = EDGE_LOOP ( 'NONE', ( #36894, #6607, #27198, #40819 ) ) ;
#9340 = CARTESIAN_POINT ( 'NONE',  ( -2.595273106918313033, -2.906811120256372671, 9.741991644047246268 ) ) ;
#9341 = VECTOR ( 'NONE', #15656, 1000.000000000000000 ) ;
#9342 = DIRECTION ( 'NONE',  ( -0.000000000000000000, -1.000000000000000000, -0.000000000000000000 ) ) ;
#9343 = PLANE ( 'NONE',  #4057 ) ;
#9344 = CARTESIAN_POINT ( 'NONE',  ( 16.76006782980217125, -2.050259795448531541, 9.178419661560148768 ) ) ;
#9345 = ORIENTED_EDGE ( 'NONE', *, *, #28107, .F. ) ;
#9346 = ORIENTED_EDGE ( 'NONE', *, *, #42207, .F. ) ;
#9347 = CARTESIAN_POINT ( 'NONE',  ( 9.358026734184097251, 0.000000000000000000, 0.000000000000000000 ) ) ;
#9348 = AXIS2_PLACEMENT_3D ( 'NONE', #32521, #13744, #40710 ) ;
#9349 = CARTESIAN_POINT ( 'NONE',  ( 73.30402655318508209, 0.000000000000000000, 165.0000000000000000 ) ) ;
#9350 = EDGE_LOOP ( 'NONE', ( #45241, #15611, #45527, #27875 ) ) ;
#9351 = ORIENTED_EDGE ( 'NONE', *, *, #13688, .F. ) ;
#9352 = DIRECTION ( 'NONE',  ( -0.000000000000000000, -0.000000000000000000, -1.000000000000000000 ) ) ;
#9353 = CARTESIAN_POINT ( 'NONE',  ( -4.999999999999948486, -204.9999999999999716, -234.7500000000000000 ) ) ;
#9354 = FACE_OUTER_BOUND ( 'NONE', #22221, .T. ) ;
#9355 = CARTESIAN_POINT ( 'NONE',  ( 210.0000000000000568, 0.000000000000000000, -77.43171244307200141 ) ) ;
#9356 = ORIENTED_EDGE ( 'NONE', *, *, #49111, .F. ) ;
#9357 = VERTEX_POINT ( 'NONE', #8786 ) ;
#9358 = ORIENTED_EDGE ( 'NONE', *, *, #6264, .T. ) ;
#9359 = EDGE_CURVE ( 'NONE', #22541, #156, #5669, .T. ) ;
#9360 = LINE ( 'NONE', #25017, #25885 ) ;
#9361 = EDGE_LOOP ( 'NONE', ( #48661, #23097, #22922, #12239, #36221, #37777, #5611, #8853 ) ) ;
#9362 = EDGE_LOOP ( 'NONE', ( #32478, #49995, #34131, #9285 ) ) ;
#9363 = CARTESIAN_POINT ( 'NONE',  ( 45.21167770612395742, 22.65616271077811206, 7.906207997025717304 ) ) ;
#9364 = ORIENTED_EDGE ( 'NONE', *, *, #21761, .F. ) ;
#9365 = B_SPLINE_CURVE_WITH_KNOTS ( 'NONE', 3,
 ( #29010, #48950, #6411, #5400 ),
 .UNSPECIFIED., .F., .F.,
 ( 4, 4 ),
 ( 0.000000000000000000, 0.2545280377015988749 ),
 .UNSPECIFIED. ) ;
#9366 = VERTEX_POINT ( 'NONE', #17229 ) ;
#9367 = CARTESIAN_POINT ( 'NONE',  ( 1.377594142017867673, -0.6023266041008059624, 9.944962737616616977 ) ) ;
#9368 = CARTESIAN_POINT ( 'NONE',  ( -165.0000000000000284, 16.00000000000000000, 35.00000000000000000 ) ) ;
#9369 = ORIENTED_EDGE ( 'NONE', *, *, #31964, .F. ) ;
#9370 = CARTESIAN_POINT ( 'NONE',  ( 0.4166666666666664631, 0.000000000000000000, 10.00000000000000000 ) ) ;
#9371 = PLANE ( 'NONE',  #17504 ) ;
#9372 = FACE_BOUND ( 'NONE', #47219, .T. ) ;
#9373 = CARTESIAN_POINT ( 'NONE',  ( 169.0000000000000284, 175.0000000000000284, 355.9999999999998863 ) ) ;
#9374 = ADVANCED_FACE ( 'NONE', ( #35750 ), #582, .T. ) ;
#9375 = EDGE_CURVE ( 'NONE', #48546, #45606, #36243, .T. ) ;
#9376 = CARTESIAN_POINT ( 'NONE',  ( 26.25702031264353664, -26.77347351953840615, 8.914903342594564961 ) ) ;
#9377 = ORIENTED_EDGE ( 'NONE', *, *, #50589, .T. ) ;
#9378 = AXIS2_PLACEMENT_3D ( 'NONE', #33147, #48723, #13620 ) ;
#9379 = FACE_OUTER_BOUND ( 'NONE', #34440, .T. ) ;
#9380 = CARTESIAN_POINT ( 'NONE',  ( 16.69947034530964913, -2.312583065866261389, 2.590526750877053086 ) ) ;
#9381 = DIRECTION ( 'NONE',  ( 0.000000000000000000, 0.000000000000000000, 1.000000000000000000 ) ) ;
#9382 = CARTESIAN_POINT ( 'NONE',  ( 25.45361382821543828, -27.58774327458490916, 1.982731392810412441 ) ) ;
#9383 = VECTOR ( 'NONE', #27732, 1000.000000000000000 ) ;
#9384 = ADVANCED_FACE ( 'NONE', ( #4913 ), #24685, .F. ) ;
#9385 = EDGE_CURVE ( 'NONE', #8942, #47543, #48190, .T. ) ;
#9386 =( BOUNDED_CURVE ( )  B_SPLINE_CURVE ( 3, ( #16461, #47709, #32114, #4895 ),
 .UNSPECIFIED., .F., .F. ) 
 B_SPLINE_CURVE_WITH_KNOTS ( ( 4, 4 ),
 ( 4.712388980384689674, 6.283185307179586232 ),
 .UNSPECIFIED. ) 
 CURVE ( )  GEOMETRIC_REPRESENTATION_ITEM ( )  RATIONAL_B_SPLINE_CURVE ( ( 1.000000000000000000, 0.8047378541243649375, 0.8047378541243649375, 1.000000000000000000 ) ) 
 REPRESENTATION_ITEM ( '' )  );
#9387 = FACE_OUTER_BOUND ( 'NONE', #15657, .T. ) ;
#9388 = ADVANCED_FACE ( 'NONE', ( #8530 ), #25178, .T. ) ;
#9389 = CARTESIAN_POINT ( 'NONE',  ( -0.4166666666666669072, 0.000000000000000000, 10.00000000000000000 ) ) ;
#9390 = FACE_OUTER_BOUND ( 'NONE', #40343, .T. ) ;
#9391 =( BOUNDED_CURVE ( )  B_SPLINE_CURVE ( 3, ( #12968, #40700, #36622, #44262 ),
 .UNSPECIFIED., .F., .F. ) 
 B_SPLINE_CURVE_WITH_KNOTS ( ( 4, 4 ),
 ( 4.712388980384689674, 6.283185307179586232 ),
 .UNSPECIFIED. ) 
 CURVE ( )  GEOMETRIC_REPRESENTATION_ITEM ( )  RATIONAL_B_SPLINE_CURVE ( ( 1.000000000000000000, 0.8047378541243649375, 0.8047378541243649375, 1.000000000000000000 ) ) 
 REPRESENTATION_ITEM ( '' )  );
#9392 = CARTESIAN_POINT ( 'NONE',  ( 1.540526284687965264, -1.371707213411490267, 9.886433018048071730 ) ) ;
#9393 = ORIENTED_EDGE ( 'NONE', *, *, #28688, .T. ) ;
#9394 = CARTESIAN_POINT ( 'NONE',  ( 111.5540265531850679, 0.000000000000000000, 122.5682875569279560 ) ) ;
#9395 = AXIS2_PLACEMENT_3D ( 'NONE', #22191, #9876, #22433 ) ;
#9396 = CARTESIAN_POINT ( 'NONE',  ( 0.3862712429686894766, -1.188820645368940276, 10.00000000000000000 ) ) ;
#9397 = VECTOR ( 'NONE', #22567, 1000.000000000000000 ) ;
#9398 = CARTESIAN_POINT ( 'NONE',  ( -20.21530556545279111, 31.58467066308232063, -9.422646554964174470 ) ) ;
#9399 = CARTESIAN_POINT ( 'NONE',  ( 210.0000000000000568, 0.000000000000000000, 160.8182875569279702 ) ) ;
#9400 = CARTESIAN_POINT ( 'NONE',  ( 350.0000000000000000, -168.9999999999999432, -344.0000000000001705 ) ) ;
#9401 = ORIENTED_EDGE ( 'NONE', *, *, #39108, .F. ) ;
#9402 = CARTESIAN_POINT ( 'NONE',  ( -124.9459734468149463, 2.143131898507847836E-16, 165.0000000000000000 ) ) ;
#9403 = EDGE_LOOP ( 'NONE', ( #33604, #10684, #10255, #2026 ) ) ;
#9404 = CARTESIAN_POINT ( 'NONE',  ( -50.11058929355266400, 7.578863168071933387, 7.455576670931136185 ) ) ;
#9405 = CARTESIAN_POINT ( 'NONE',  ( -167.7210997126620384, -1.750000000000010214, 121.8434138227750623 ) ) ;
#9406 = ORIENTED_EDGE ( 'NONE', *, *, #29481, .T. ) ;
#9407 = DIRECTION ( 'NONE',  ( 0.000000000000000000, -1.000000000000000000, 0.000000000000000000 ) ) ;
#9408 = LINE ( 'NONE', #17358, #30664 ) ;
#9409 = AXIS2_PLACEMENT_3D ( 'NONE', #23557, #39215, #19702 ) ;
#9410 = EDGE_LOOP ( 'NONE', ( #18706, #38084, #1019 ) ) ;
#9411 = EDGE_LOOP ( 'NONE', ( #2883, #23134, #14206, #21008, #1950 ) ) ;
#9412 = EDGE_CURVE ( 'NONE', #40195, #16306, #44401, .T. ) ;
#9413 = AXIS2_PLACEMENT_3D ( 'NONE', #43306, #23048, #38978 ) ;
#9414 = EDGE_CURVE ( 'NONE', #26571, #50487, #6609, .T. ) ;
#9415 = CARTESIAN_POINT ( 'NONE',  ( 15.00000000000000000, 12.98684210526315752, 19.37312575500900280 ) ) ;
#9416 = CARTESIAN_POINT ( 'NONE',  ( 17.23491422248386584, -0.5912720620000816441, 8.727788335465566760 ) ) ;
#9417 = CARTESIAN_POINT ( 'NONE',  ( -165.0000000000000284, 16.00000000000000000, -114.9999999999999858 ) ) ;
#9418 = ORIENTED_EDGE ( 'NONE', *, *, #35720, .T. ) ;
#9419 = DIRECTION ( 'NONE',  ( 0.000000000000000000, 0.000000000000000000, 1.000000000000000000 ) ) ;
#9420 = EDGE_LOOP ( 'NONE', ( #2564, #38195, #33601, #14464, #46246, #32992 ) ) ;
#9421 = EDGE_LOOP ( 'NONE', ( #22636, #11887, #27217, #7354 ) ) ;
#9422 = VERTEX_POINT ( 'NONE', #24435 ) ;
#9423 = DIRECTION ( 'NONE',  ( 1.000000000000000000, 0.000000000000000000, 0.000000000000000000 ) ) ;
#9424 = CARTESIAN_POINT ( 'NONE',  ( -1.275927284277175167, 0.1224368140627496299, 9.976582533991679824 ) ) ;
#9425 = ORIENTED_EDGE ( 'NONE', *, *, #48039, .F. ) ;
#9426 = CARTESIAN_POINT ( 'NONE',  ( -30.25247992116029394, 39.82368563463828792, -3.760136334089591248 ) ) ;
#9427 = CARTESIAN_POINT ( 'NONE',  ( -36.97942854200451990, 6.226705766838657397, 8.914903342594564961 ) ) ;
#9428 = VECTOR ( 'NONE', #22877, 1000.000000000000000 ) ;
#9429 = DIRECTION ( 'NONE',  ( -1.000000000000000000, -0.000000000000000000, -0.000000000000000000 ) ) ;
#9430 = PLANE ( 'NONE',  #32919 ) ;
#9431 = CYLINDRICAL_SURFACE ( 'NONE', #38867, 0.5000000000000004441 ) ;
#9432 = VECTOR ( 'NONE', #12970, 1000.000000000000000 ) ;
#9433 = CARTESIAN_POINT ( 'NONE',  ( -205.6708471809678827, -1.750000000000010436, -80.20683870891910772 ) ) ;
#9434 = DIRECTION ( 'NONE',  ( 1.000000000000000000, 0.000000000000000000, 0.000000000000000000 ) ) ;
#9435 = CARTESIAN_POINT ( 'NONE',  ( 135.0000000000006253, 17.00000000000000000, -54.99999999999999289 ) ) ;
#9436 = FACE_OUTER_BOUND ( 'NONE', #32893, .T. ) ;
#9437 = CARTESIAN_POINT ( 'NONE',  ( 191.5540265531851105, 0.000000000000000000, 79.06828755692797017 ) ) ;
#9438=STYLED_ITEM('',(#50775),#22320);
#9439 = CARTESIAN_POINT ( 'NONE',  ( -5.647304616913629616, 159.2880105690400399, 23.74256005001722158 ) ) ;
#9440 = ORIENTED_EDGE ( 'NONE', *, *, #9317, .F. ) ;
#9441 = EDGE_CURVE ( 'NONE', #45821, #12693, #50693, .T. ) ;
#9442 = CYLINDRICAL_SURFACE ( 'NONE', #25351, 1.749999999999973799 ) ;
#9443 = CARTESIAN_POINT ( 'NONE',  ( -7.200076171898729172, 0.000000000000000000, 0.000000000000000000 ) ) ;
#9444 = DIRECTION ( 'NONE',  ( -0.4740998230350175202, 0.3386427307392980146, -0.8127425537743157014 ) ) ;
#9445 =( GEOMETRIC_REPRESENTATION_CONTEXT ( 3 ) GLOBAL_UNCERTAINTY_ASSIGNED_CONTEXT ( ( #27008 ) ) GLOBAL_UNIT_ASSIGNED_CONTEXT ( ( #18758, #33681, #45182 ) ) REPRESENTATION_CONTEXT ( 'NONE', 'WORKASPACE' ) );
#9446 = CIRCLE ( 'NONE', #14353, 2.000000000000001776 ) ;
#9447 = DIRECTION ( 'NONE',  ( -1.000000000000000000, 0.000000000000000000, 0.000000000000000000 ) ) ;
#9448 = ORIENTED_EDGE ( 'NONE', *, *, #5640, .F. ) ;
#9449 = DIRECTION ( 'NONE',  ( 1.000000000000000000, 0.000000000000000000, 0.000000000000000000 ) ) ;
#9450 = FACE_OUTER_BOUND ( 'NONE', #2836, .T. ) ;
#9451 = ORIENTED_EDGE ( 'NONE', *, *, #15000, .T. ) ;
#9452 = CARTESIAN_POINT ( 'NONE',  ( -46.69597344681494633, -1.750000000000010658, -119.1817124430720440 ) ) ;
#9453 = FACE_OUTER_BOUND ( 'NONE', #13320, .T. ) ;
#9454 = CARTESIAN_POINT ( 'NONE',  ( 0.4400426740873927822, -2.015233077865103972, 9.886433018048071730 ) ) ;
#9455 = ORIENTED_EDGE ( 'NONE', *, *, #27646, .F. ) ;
#9456 = CARTESIAN_POINT ( 'NONE',  ( 73.30402655318508209, -1.750000000000010658, -79.18171244307201562 ) ) ;
#9457 = ORIENTED_EDGE ( 'NONE', *, *, #6445, .T. ) ;
#9458 = ORIENTED_EDGE ( 'NONE', *, *, #8337, .F. ) ;
#9459 = B_SPLINE_CURVE_WITH_KNOTS ( 'NONE', 3,
 ( #30434, #2964, #2718, #50126 ),
 .UNSPECIFIED., .F., .F.,
 ( 4, 4 ),
 ( 0.7491799374948677759, 1.000000000000000000 ),
 .UNSPECIFIED. ) ;
#9460 = VECTOR ( 'NONE', #390, 1000.000000000000000 ) ;
#9461 = ORIENTED_EDGE ( 'NONE', *, *, #38597, .F. ) ;
#9462 = DIRECTION ( 'NONE',  ( -1.000000000000000000, 0.000000000000000000, -0.000000000000000000 ) ) ;
#9463 = DIRECTION ( 'NONE',  ( -1.000000000000000000, -0.000000000000000000, -0.000000000000000000 ) ) ;
#9464 = VECTOR ( 'NONE', #46576, 1000.000000000000000 ) ;
#9465 = ORIENTED_EDGE ( 'NONE', *, *, #15031, .T. ) ;
#9466 = CARTESIAN_POINT ( 'NONE',  ( 29.39982726364966581, 16.78152490921169360, 8.356839323120299312 ) ) ;
#9467 = CARTESIAN_POINT ( 'NONE',  ( 240.0000000000000000, -164.9999999999999716, 32.29650858650035161 ) ) ;
#9468 = CARTESIAN_POINT ( 'NONE',  ( -0.9602803029231570253, 0.8490247040095960651, 9.976582533991679824 ) ) ;
#9469 = VECTOR ( 'NONE', #4655, 1000.000000000000000 ) ;
#9470 = DIRECTION ( 'NONE',  ( -0.000000000000000000, -1.000000000000000000, -0.000000000000000000 ) ) ;
#9471 = VERTEX_POINT ( 'NONE', #16720 ) ;
#9472 = PLANE ( 'NONE',  #39582 ) ;
#9473 = ORIENTED_EDGE ( 'NONE', *, *, #19898, .T. ) ;
#9474 = DIRECTION ( 'NONE',  ( 0.000000000000000000, 0.000000000000000000, -1.000000000000000000 ) ) ;
#9475 = DIRECTION ( 'NONE',  ( 0.000000000000000000, -0.3846153846153844702, 0.9230769230769231282 ) ) ;
#9476 = EDGE_LOOP ( 'NONE', ( #39624, #46789, #19400 ) ) ;
#9477 = VECTOR ( 'NONE', #3420, 1000.000000000000000 ) ;
#9478 = ORIENTED_EDGE ( 'NONE', *, *, #38074, .T. ) ;
#9479 = VERTEX_POINT ( 'NONE', #20570 ) ;
#9480 = DIRECTION ( 'NONE',  ( -1.000000000000000000, -0.000000000000000000, -0.000000000000000000 ) ) ;
#9481 = LINE ( 'NONE', #9730, #7102 ) ;
#9482 = VERTEX_POINT ( 'NONE', #47977 ) ;
#9483 = VECTOR ( 'NONE', #15054, 1000.000000000000000 ) ;
#9484 = VECTOR ( 'NONE', #15844, 1000.000000000000000 ) ;
#9485 = CARTESIAN_POINT ( 'NONE',  ( -1.222012661920452326, 0.2471648704738776681, 9.981352469109934233 ) ) ;
#9486 = FACE_OUTER_BOUND ( 'NONE', #35460, .T. ) ;
#9487 = CARTESIAN_POINT ( 'NONE',  ( -1.011271242968693862, 0.7347315653655780432, -10.00000000000000000 ) ) ;
#9488 = ORIENTED_EDGE ( 'NONE', *, *, #36880, .T. ) ;
#9489 = LINE ( 'NONE', #10257, #9756 ) ;
#9490 = CARTESIAN_POINT ( 'NONE',  ( 40.32982405930692948, 10.56057144604287146, -9.387872844313825738 ) ) ;
#9491 = CARTESIAN_POINT ( 'NONE',  ( 210.0000000000000568, 0.000000000000000000, -39.18171244307202983 ) ) ;
#9492 = ORIENTED_EDGE ( 'NONE', *, *, #43322, .T. ) ;
#9493 = ORIENTED_EDGE ( 'NONE', *, *, #23991, .F. ) ;
#9494 = APPLICATION_PROTOCOL_DEFINITION ( 'draft international standard', 'automotive_design', 1998, #10904 ) ;
#9495 = DIRECTION ( 'NONE',  ( -1.000000000000000000, -0.000000000000000000, -0.000000000000000000 ) ) ;
#9496 = CARTESIAN_POINT ( 'NONE',  ( 1.552956552085973607, 0.2464513101957388486, 9.945241992664932695 ) ) ;
#9497 = CIRCLE ( 'NONE', #42279, 4.000000000000003553 ) ;
#9498 = LINE ( 'NONE', #24911, #24873 ) ;
#9499 = FACE_OUTER_BOUND ( 'NONE', #43321, .T. ) ;
#9500 = ORIENTED_EDGE ( 'NONE', *, *, #36183, .T. ) ;
#9501 = FACE_OUTER_BOUND ( 'NONE', #4830, .T. ) ;
#9502 = EDGE_CURVE ( 'NONE', #40469, #21418, #22259, .T. ) ;
#9503 = LINE ( 'NONE', #3568, #15464 ) ;
#9504 = LINE ( 'NONE', #24917, #28269 ) ;
#9505 = EDGE_CURVE ( 'NONE', #30045, #38616, #31723, .T. ) ;
#9506 = LINE ( 'NONE', #29516, #20530 ) ;
#9507 = EDGE_CURVE ( 'NONE', #34169, #4486, #27526, .T. ) ;
#9508 = VECTOR ( 'NONE', #24567, 1000.000000000000000 ) ;
#9509 = ORIENTED_EDGE ( 'NONE', *, *, #32344, .T. ) ;
#9510 = LINE ( 'NONE', #29773, #18229 ) ;
#9511 = ORIENTED_EDGE ( 'NONE', *, *, #6239, .T. ) ;
#9512 = DIRECTION ( 'NONE',  ( -1.000000000000000000, 0.000000000000000000, 6.938893903907222067E-15 ) ) ;
#9513 = VERTEX_POINT ( 'NONE', #28019 ) ;
#9514 = CARTESIAN_POINT ( 'NONE',  ( -166.6959734468149463, -1.750000000000010214, 40.81828755692798438 ) ) ;
#9515 = CARTESIAN_POINT ( 'NONE',  ( 168.9999999999999716, -97.49999999999998579, -340.0000000000001137 ) ) ;
#9516 = EDGE_CURVE ( 'NONE', #32226, #1016, #48227, .T. ) ;
#9517 = LINE ( 'NONE', #25176, #17512 ) ;
#9518 = ORIENTED_EDGE ( 'NONE', *, *, #50611, .F. ) ;
#9519 = AXIS2_PLACEMENT_3D ( 'NONE', #28286, #20826, #20328 ) ;
#9520 = EDGE_CURVE ( 'NONE', #27480, #28855, #13116, .T. ) ;
#9521 =( BOUNDED_CURVE ( )  B_SPLINE_CURVE ( 3, ( #46489, #23697, #16249, #19333 ),
 .UNSPECIFIED., .F., .F. ) 
 B_SPLINE_CURVE_WITH_KNOTS ( ( 4, 4 ),
 ( 4.712388980384689674, 6.283185307179586232 ),
 .UNSPECIFIED. ) 
 CURVE ( )  GEOMETRIC_REPRESENTATION_ITEM ( )  RATIONAL_B_SPLINE_CURVE ( ( 1.000000000000000000, 0.8047378541243649375, 0.8047378541243649375, 1.000000000000000000 ) ) 
 REPRESENTATION_ITEM ( '' )  );
#9522 = CARTESIAN_POINT ( 'NONE',  ( 24.87155650802130680, -38.55075836233088893, -9.367992836599951190 ) ) ;
#9523 = ORIENTED_EDGE ( 'NONE', *, *, #16270, .F. ) ;
#9524 = CARTESIAN_POINT ( 'NONE',  ( 151.5540265531850537, 0.000000000000000000, 165.0000000000000000 ) ) ;
#9525 = CARTESIAN_POINT ( 'NONE',  ( -124.9459734468149463, 2.143131898507847836E-16, -0.9317124430719969652 ) ) ;
#9526 = LINE ( 'NONE', #44651, #36089 ) ;
#9527 = CARTESIAN_POINT ( 'NONE',  ( -0.4266413953668892756, -1.250184266969579294, 9.943883492372849631 ) ) ;
#9528 =( BOUNDED_CURVE ( )  B_SPLINE_CURVE ( 3, ( #1257, #17392, #17882, #28694 ),
 .UNSPECIFIED., .F., .F. ) 
 B_SPLINE_CURVE_WITH_KNOTS ( ( 4, 4 ),
 ( 4.712388980384689674, 6.283185307179586232 ),
 .UNSPECIFIED. ) 
 CURVE ( )  GEOMETRIC_REPRESENTATION_ITEM ( )  RATIONAL_B_SPLINE_CURVE ( ( 1.000000000000000000, 0.8047378541243649375, 0.8047378541243649375, 1.000000000000000000 ) ) 
 REPRESENTATION_ITEM ( '' )  );
#9529 = DIRECTION ( 'NONE',  ( -0.000000000000000000, -0.000000000000000000, -1.000000000000000000 ) ) ;
#9530 = ORIENTED_EDGE ( 'NONE', *, *, #737, .T. ) ;
#9532 = ORIENTED_EDGE ( 'NONE', *, *, #1066, .F. ) ;
#9531 = EDGE_CURVE ( 'NONE', #26103, #43683, #44893, .T. ) ;
#9533 = CARTESIAN_POINT ( 'NONE',  ( -5.000000000000000000, -184.7999999999999545, -359.8000000000002387 ) ) ;
#9534 = EDGE_CURVE ( 'NONE', #16032, #31922, #26256, .T. ) ;
#9535 = ADVANCED_FACE ( 'NONE', ( #22328 ), #45144, .F. ) ;
#9536 = EDGE_CURVE ( 'NONE', #33010, #14624, #32762, .T. ) ;
#9537 = ORIENTED_EDGE ( 'NONE', *, *, #22357, .F. ) ;
#9538 = AXIS2_PLACEMENT_3D ( 'NONE', #15160, #14905, #41848 ) ;
#9539 = DIRECTION ( 'NONE',  ( -1.000000000000000000, -0.000000000000000000, -0.000000000000000000 ) ) ;
#9540 = CARTESIAN_POINT ( 'NONE',  ( -0.1265591857321690383, -1.213367045380180809, 9.963925895596192461 ) ) ;
#9541 = VECTOR ( 'NONE', #15669, 1000.000000000000000 ) ;
#9542 = ORIENTED_EDGE ( 'NONE', *, *, #39388, .T. ) ;
#9543 = CARTESIAN_POINT ( 'NONE',  ( 15.00000000000000000, -46.01315789473684248, -5.916985404131813731 ) ) ;
#9544 = EDGE_CURVE ( 'NONE', #46997, #23241, #46390, .T. ) ;
#9545 = EDGE_CURVE ( 'NONE', #29162, #24955, #45652, .T. ) ;
#9546 =( BOUNDED_CURVE ( )  B_SPLINE_CURVE ( 3, ( #15321, #47069, #43509, #30974 ),
 .UNSPECIFIED., .F., .F. ) 
 B_SPLINE_CURVE_WITH_KNOTS ( ( 4, 4 ),
 ( 0.000000000000000000, 1.570796326794896558 ),
 .UNSPECIFIED. ) 
 CURVE ( )  GEOMETRIC_REPRESENTATION_ITEM ( )  RATIONAL_B_SPLINE_CURVE ( ( 1.000000000000000000, 0.8047378541243649375, 0.8047378541243649375, 1.000000000000000000 ) ) 
 REPRESENTATION_ITEM ( '' )  );
#9547 = DIRECTION ( 'NONE',  ( 0.000000000000000000, 2.265761274745217480E-16, -1.000000000000000000 ) ) ;
#9548 = ORIENTED_EDGE ( 'NONE', *, *, #29716, .T. ) ;
#9549 = CYLINDRICAL_SURFACE ( 'NONE', #24356, 4.000000000000003553 ) ;
#9550 = CARTESIAN_POINT ( 'NONE',  ( 0.3862712429686810944, 1.188820645368943607, 3.333333333333333481 ) ) ;
#9551 = DIRECTION ( 'NONE',  ( -0.000000000000000000, -0.000000000000000000, -1.000000000000000000 ) ) ;
#9553 = AXIS2_PLACEMENT_3D ( 'NONE', #24144, #39283, #7729 ) ;
#9552 = DIRECTION ( 'NONE',  ( 2.775557561562891351E-16, 0.7071067811865477948, 0.7071067811865473507 ) ) ;
#9554 = VERTEX_POINT ( 'NONE', #17734 ) ;
#9555 = ORIENTED_EDGE ( 'NONE', *, *, #20537, .T. ) ;
#9556 = EDGE_LOOP ( 'NONE', ( #8835, #40877, #36846, #48279 ) ) ;
#9557 = VECTOR ( 'NONE', #26538, 1000.000000000000000 ) ;
#9558 = CARTESIAN_POINT ( 'NONE',  ( -44.94597344681493922, 2.143131898507880377E-16, 42.56828755692798438 ) ) ;
#9559 = CARTESIAN_POINT ( 'NONE',  ( -0.3862712429686729343, -1.188820645368946050, 10.00000000000000000 ) ) ;
#9560 = CARTESIAN_POINT ( 'NONE',  ( 339.9999999999999432, -180.9999999999999716, -340.0000000000001705 ) ) ;
#9561 = CARTESIAN_POINT ( 'NONE',  ( -1.249999999999999778, 0.000000000000000000, 3.333333333333333481 ) ) ;
#9562 = ORIENTED_EDGE ( 'NONE', *, *, #17824, .T. ) ;
#9563 = EDGE_CURVE ( 'NONE', #50334, #39140, #47097, .T. ) ;
#9564 = AXIS2_PLACEMENT_3D ( 'NONE', #37454, #33342, #2272 ) ;
#9565 = FACE_OUTER_BOUND ( 'NONE', #33287, .T. ) ;
#9566 = ORIENTED_EDGE ( 'NONE', *, *, #47719, .T. ) ;
#9567 = CYLINDRICAL_SURFACE ( 'NONE', #10555, 1.750000000000008438 ) ;
#9568 = FACE_OUTER_BOUND ( 'NONE', #13745, .T. ) ;
#9569 = FACE_BOUND ( 'NONE', #46022, .T. ) ;
#9570 = EDGE_CURVE ( 'NONE', #19221, #30619, #25947, .T. ) ;
#9571 = ADVANCED_FACE ( 'NONE', ( #6679 ), #34163, .F. ) ;
#9572 = FACE_OUTER_BOUND ( 'NONE', #6734, .T. ) ;
#9573 = CARTESIAN_POINT ( 'NONE',  ( 164.9999999999999716, -5.999999999999950262, -340.0000000000001137 ) ) ;
#9574 = DIRECTION ( 'NONE',  ( -1.612977847700450206E-50, 0.000000000000000000, -1.000000000000000000 ) ) ;
#9575 = EDGE_LOOP ( 'NONE', ( #14324, #31273, #38521, #14127 ) ) ;
#9576 = FACE_OUTER_BOUND ( 'NONE', #11976, .T. ) ;
#9577 = CARTESIAN_POINT ( 'NONE',  ( 71.55402655318505367, 0.000000000000000000, -157.4317124430720014 ) ) ;
#9578 = EDGE_CURVE ( 'NONE', #30056, #35621, #22558, .T. ) ;
#9579 = CARTESIAN_POINT ( 'NONE',  ( 33.86622497129647513, -3.037805405904928868, 7.906207997025717304 ) ) ;
#9581 = ORIENTED_EDGE ( 'NONE', *, *, #47461, .T. ) ;
#9580 = CIRCLE ( 'NONE', #26798, 2.000000000000001776 ) ;
#9582 = FACE_OUTER_BOUND ( 'NONE', #31883, .T. ) ;
#9583 = VERTEX_POINT ( 'NONE', #21571 ) ;
#9584 = CARTESIAN_POINT ( 'NONE',  ( -45.67084718096785423, 1.750000000000010214, 81.84341382277507648 ) ) ;
#9585 = CARTESIAN_POINT ( 'NONE',  ( 356.0000000000003411, 165.0000000000000000, -92.00000000000019895 ) ) ;
#9586 = EDGE_CURVE ( 'NONE', #20951, #46680, #2088, .T. ) ;
#9587 = ORIENTED_EDGE ( 'NONE', *, *, #44110, .T. ) ;
#9588 = ORIENTED_EDGE ( 'NONE', *, *, #6094, .T. ) ;
#9589 = CARTESIAN_POINT ( 'NONE',  ( 0.000000000000000000, 0.000000000000000000, 0.000000000000000000 ) ) ;
#9590 = LINE ( 'NONE', #40888, #48345 ) ;
#9591 = ADVANCED_FACE ( 'NONE', ( #33153 ), #30293, .T. ) ;
#9592 = CARTESIAN_POINT ( 'NONE',  ( 210.0000000000000568, 0.000000000000000000, 2.568287556927987048 ) ) ;
#9593 = CARTESIAN_POINT ( 'NONE',  ( 50.11058929355270664, -7.578863168071591438, 7.455576670931136185 ) ) ;
#9594 = ORIENTED_EDGE ( 'NONE', *, *, #12105, .T. ) ;
#9595 = VERTEX_POINT ( 'NONE', #33896 ) ;
#9596 = DIRECTION ( 'NONE',  ( 0.000000000000000000, 0.000000000000000000, -1.000000000000000000 ) ) ;
#9597 = AXIS2_PLACEMENT_3D ( 'NONE', #35007, #19564, #31397 ) ;
#9598 = CARTESIAN_POINT ( 'NONE',  ( 0.000000000000000000, -165.1999999999999602, 340.1999999999997044 ) ) ;
#9599 = EDGE_CURVE ( 'NONE', #41270, #29317, #49490, .T. ) ;
#9600 = EDGE_CURVE ( 'NONE', #25574, #4867, #25688, .T. ) ;
#9601 = ORIENTED_EDGE ( 'NONE', *, *, #38117, .T. ) ;
#9602 = ORIENTED_EDGE ( 'NONE', *, *, #18181, .F. ) ;
#9603 = CARTESIAN_POINT ( 'NONE',  ( 168.9999999999999716, -272.5000000000000000, -94.99999999999988631 ) ) ;
#9604 = CARTESIAN_POINT ( 'NONE',  ( 1.721971274562253740, 0.09408549481334846365, 9.928159647716247704 ) ) ;
#9605 = DIRECTION ( 'NONE',  ( -0.000000000000000000, -0.000000000000000000, 1.000000000000000000 ) ) ;
#9606 = DIRECTION ( 'NONE',  ( -0.000000000000000000, -1.000000000000000000, -0.000000000000000000 ) ) ;
#9607 = ORIENTED_EDGE ( 'NONE', *, *, #45706, .T. ) ;
#9608 = EDGE_LOOP ( 'NONE', ( #23657, #44296, #28053, #44120 ) ) ;
#9609 = ORIENTED_EDGE ( 'NONE', *, *, #17355, .F. ) ;
#9610 = ADVANCED_FACE ( 'NONE', ( #2327 ), #9204, .T. ) ;
#9611 = EDGE_CURVE ( 'NONE', #50205, #12217, #47020, .T. ) ;
#9612 = DIRECTION ( 'NONE',  ( 0.000000000000000000, 0.000000000000000000, 1.000000000000000000 ) ) ;
#9613 = EDGE_CURVE ( 'NONE', #5706, #29610, #34725, .T. ) ;
#9614 = CARTESIAN_POINT ( 'NONE',  ( 0.8995557326246120811, 5.891360083018336802, 4.370690007832189750E-16 ) ) ;
#9615 = ORIENTED_EDGE ( 'NONE', *, *, #42119, .F. ) ;
#9616 = ORIENTED_EDGE ( 'NONE', *, *, #19386, .F. ) ;
#9617 = CARTESIAN_POINT ( 'NONE',  ( -48.44597344681495343, 0.000000000000000000, -37.43171244307200141 ) ) ;
#9618 = DIRECTION ( 'NONE',  ( 0.000000000000000000, -2.265761274745217480E-16, 1.000000000000000000 ) ) ;
#9619 = ORIENTED_EDGE ( 'NONE', *, *, #15792, .T. ) ;
#9621 = ORIENTED_EDGE ( 'NONE', *, *, #11567, .T. ) ;
#9620 = B_SPLINE_CURVE_WITH_KNOTS ( 'NONE', 3,
 ( #9889, #20682, #36357, #1200 ),
 .UNSPECIFIED., .F., .F.,
 ( 4, 4 ),
 ( 0.000000000000000000, 0.0002520763768916309180 ),
 .UNSPECIFIED. ) ;
#9622 = CARTESIAN_POINT ( 'NONE',  ( -84.94597344681494633, 2.143131898507880377E-16, -80.93171244307201562 ) ) ;
#9623 = CYLINDRICAL_SURFACE ( 'NONE', #3460, 1.750000000000036193 ) ;
#9624 = EDGE_LOOP ( 'NONE', ( #15315, #45539, #18156, #23223, #28370, #39665 ) ) ;
#9625 = CARTESIAN_POINT ( 'NONE',  ( -7.896046458374534893, 6.155518428822186472, 6.185594734181544929 ) ) ;
#9626 = DIRECTION ( 'NONE',  ( 0.000000000000000000, 0.000000000000000000, 1.000000000000000000 ) ) ;
#9627 = DIRECTION ( 'NONE',  ( -0.000000000000000000, -1.000000000000000000, -0.000000000000000000 ) ) ;
#9628 = CARTESIAN_POINT ( 'NONE',  ( -15.00000000000000000, 13.59802227364770388, 19.51251772323705325 ) ) ;
#9629 = EDGE_CURVE ( 'NONE', #38277, #14475, #11742, .T. ) ;
#9630 =( BOUNDED_CURVE ( )  B_SPLINE_CURVE ( 3, ( #12989, #24559, #48362, #36124 ),
 .UNSPECIFIED., .F., .F. ) 
 B_SPLINE_CURVE_WITH_KNOTS ( ( 4, 4 ),
 ( 0.000000000000000000, 1.570796326794896780 ),
 .UNSPECIFIED. ) 
 CURVE ( )  GEOMETRIC_REPRESENTATION_ITEM ( )  RATIONAL_B_SPLINE_CURVE ( ( 1.000000000000000000, 0.8047378541243649375, 0.8047378541243649375, 1.000000000000000000 ) ) 
 REPRESENTATION_ITEM ( '' )  );
#9631 = CARTESIAN_POINT ( 'NONE',  ( -46.69597344681494633, 0.000000000000000000, 165.0000000000000000 ) ) ;
#9632 = ORIENTED_EDGE ( 'NONE', *, *, #34394, .F. ) ;
#9633 = CARTESIAN_POINT ( 'NONE',  ( 432.7825420346616170, 102.9547873477646647, -7.018571579996165433 ) ) ;
#9634 = LINE ( 'NONE', #40936, #39609 ) ;
#9635 = B_SPLINE_SURFACE_WITH_KNOTS ( 'NONE', 3, 3, ( 
 ( #2497, #21996, #18138, #37668 ),
 ( #17391, #33057, #21485, #37176 ),
 ( #3491, #42498, #46823, #18889 ),
 ( #3240, #34568, #7622, #19149 ) ),
 .UNSPECIFIED., .F., .F., .F.,
 ( 4, 4 ),
 ( 4, 4 ),
 ( 0.000000000000000000, 1.000000000000000000 ),
 ( 0.000000000000000000, 1.000000000000000000 ),
 .UNSPECIFIED. ) ;
#9636 = DIRECTION ( 'NONE',  ( 0.000000000000000000, 0.000000000000000000, 1.000000000000000000 ) ) ;
#9637 = DIRECTION ( 'NONE',  ( -1.586032880504786307E-16, 1.654361225106055350E-24, -1.000000000000000000 ) ) ;
#9638 = DIRECTION ( 'NONE',  ( 0.000000000000000000, 0.000000000000000000, 1.000000000000000000 ) ) ;
#9639 = LINE ( 'NONE', #25287, #21229 ) ;
#9640 = DIRECTION ( 'NONE',  ( 1.000000000000000000, 0.000000000000000000, 0.000000000000000000 ) ) ;
#9641 = CARTESIAN_POINT ( 'NONE',  ( -208.4459734468148611, -1.025126265847089657, 119.0682875569279560 ) ) ;
#9642 = DIRECTION ( 'NONE',  ( 0.000000000000000000, 0.000000000000000000, -1.000000000000000000 ) ) ;
#9643 = ORIENTED_EDGE ( 'NONE', *, *, #4832, .F. ) ;
#9644 = DIRECTION ( 'NONE',  ( 0.000000000000000000, 1.544785076050074834E-48, 1.000000000000000000 ) ) ;
#9645 = VECTOR ( 'NONE', #8069, 1000.000000000000000 ) ;
#9646 = CARTESIAN_POINT ( 'NONE',  ( -0.3862712429686895876, 1.188820645368940720, -10.00000000000000000 ) ) ;
#9647 = DIRECTION ( 'NONE',  ( 1.000000000000000000, 0.000000000000000000, 0.000000000000000000 ) ) ;
#9648 = DIRECTION ( 'NONE',  ( 0.000000000000000000, -0.000000000000000000, -1.000000000000000000 ) ) ;
#9649 = CARTESIAN_POINT ( 'NONE',  ( -46.69597344681494633, -1.750000000000010214, -39.18171244307202983 ) ) ;
#9650 = ORIENTED_EDGE ( 'NONE', *, *, #498, .F. ) ;
#9651 = DIRECTION ( 'NONE',  ( 1.000000000000000000, -0.000000000000000000, 0.000000000000000000 ) ) ;
#9652 = VERTEX_POINT ( 'NONE', #4548 ) ;
#9653 = CARTESIAN_POINT ( 'NONE',  ( 0.1287570809895604018, 0.3962735484563146282, 10.00000000000000000 ) ) ;
#9654 = CARTESIAN_POINT ( 'NONE',  ( 168.9999999999999716, -254.4999999999999432, -339.9999999999998863 ) ) ;
#9655 = ADVANCED_FACE ( 'NONE', ( #24060 ), #43026, .F. ) ;
#9656 = EDGE_CURVE ( 'NONE', #12217, #37517, #14607, .T. ) ;
#9657 = VERTEX_POINT ( 'NONE', #12240 ) ;
#9658 = LINE ( 'NONE', #34277, #11469 ) ;
#9659 = ORIENTED_EDGE ( 'NONE', *, *, #8337, .T. ) ;
#9660 = ORIENTED_EDGE ( 'NONE', *, *, #42903, .T. ) ;
#9661 = EDGE_CURVE ( 'NONE', #30870, #47066, #35372, .T. ) ;
#9663 = EDGE_CURVE ( 'NONE', #13070, #42474, #47605, .T. ) ;
#9662 = CARTESIAN_POINT ( 'NONE',  ( 2.538055338523177440, 33.28424297489108596, -9.367992836599954742 ) ) ;
#9664 = CARTESIAN_POINT ( 'NONE',  ( 168.9999999999999716, -77.49999999999995737, -115.0000000000001563 ) ) ;
#9665 = EDGE_CURVE ( 'NONE', #15345, #24207, #3773, .T. ) ;
#9666 = CARTESIAN_POINT ( 'NONE',  ( -21.61731705588949737, -25.43568671410585935, -9.367992836599954742 ) ) ;
#9667 = ORIENTED_EDGE ( 'NONE', *, *, #36268, .T. ) ;
#9668 = CARTESIAN_POINT ( 'NONE',  ( -165.0000000000000284, 16.00000000000000000, 60.00000000000000000 ) ) ;
#9669 = DIRECTION ( 'NONE',  ( 1.000000000000000000, -4.758098676964956461E-16, -8.975803739141899931E-48 ) ) ;
#9670 = DIRECTION ( 'NONE',  ( -1.000000000000000000, 0.000000000000000000, 0.000000000000000000 ) ) ;
#9671 = ORIENTED_EDGE ( 'NONE', *, *, #5797, .T. ) ;
#9672 = ORIENTED_EDGE ( 'NONE', *, *, #24972, .F. ) ;
#9673 = VERTEX_POINT ( 'NONE', #27907 ) ;
#9674 = CARTESIAN_POINT ( 'NONE',  ( 111.5540265531850537, -1.025126265847081886, -40.93171244307202272 ) ) ;
#9675 = B_SPLINE_CURVE_WITH_KNOTS ( 'NONE', 3,
 ( #18654, #14817, #49165, #46343 ),
 .UNSPECIFIED., .F., .F.,
 ( 4, 4 ),
 ( 0.000000000000000000, 0.0002610106747150124813 ),
 .UNSPECIFIED. ) ;
#9676 = EDGE_CURVE ( 'NONE', #3789, #42829, #43534, .T. ) ;
#9677 = LINE ( 'NONE', #20460, #5375 ) ;
#9678 = EDGE_LOOP ( 'NONE', ( #17514, #35885, #50695, #1901, #5877, #28093 ) ) ;
#9679 = CARTESIAN_POINT ( 'NONE',  ( 166.9999999999999716, -164.9999999999999432, 355.9999999999998863 ) ) ;
#9680 = CARTESIAN_POINT ( 'NONE',  ( 0.000000000000000000, -43.33333333333333570, 790.0000000000000000 ) ) ;
#9681 =( BOUNDED_CURVE ( )  B_SPLINE_CURVE ( 3, ( #159, #8364, #27348, #31969 ),
 .UNSPECIFIED., .F., .F. ) 
 B_SPLINE_CURVE_WITH_KNOTS ( ( 4, 4 ),
 ( 4.712388980384689674, 6.283185307179586232 ),
 .UNSPECIFIED. ) 
 CURVE ( )  GEOMETRIC_REPRESENTATION_ITEM ( )  RATIONAL_B_SPLINE_CURVE ( ( 1.000000000000000000, 0.8047378541243649375, 0.8047378541243649375, 1.000000000000000000 ) ) 
 REPRESENTATION_ITEM ( '' )  );
#9682 = DIRECTION ( 'NONE',  ( 0.000000000000000000, 0.000000000000000000, 1.000000000000000000 ) ) ;
#9683 = CARTESIAN_POINT ( 'NONE',  ( 181.0000000000001705, -166.9999999999999432, -115.0000000000001847 ) ) ;
#9684 = AXIS2_PLACEMENT_3D ( 'NONE', #30328, #10566, #49520 ) ;
#9685 = CARTESIAN_POINT ( 'NONE',  ( 33.30402655318503946, -1.750000000000010214, -39.18171244307202983 ) ) ;
#9686 = PLANE ( 'NONE',  #32506 ) ;
#9687 = CYLINDRICAL_SURFACE ( 'NONE', #35710, 1.749999999999987566 ) ;
#9688 =( BOUNDED_CURVE ( )  B_SPLINE_CURVE ( 3, ( #17357, #44034, #47861, #44526 ),
 .UNSPECIFIED., .F., .F. ) 
 B_SPLINE_CURVE_WITH_KNOTS ( ( 4, 4 ),
 ( 4.712388980384689674, 6.283185307179586232 ),
 .UNSPECIFIED. ) 
 CURVE ( )  GEOMETRIC_REPRESENTATION_ITEM ( )  RATIONAL_B_SPLINE_CURVE ( ( 1.000000000000000000, 0.8047378541243649375, 0.8047378541243649375, 1.000000000000000000 ) ) 
 REPRESENTATION_ITEM ( '' )  );
#9689 = FACE_OUTER_BOUND ( 'NONE', #42752, .T. ) ;
#9690 = B_SPLINE_CURVE_WITH_KNOTS ( 'NONE', 3,
 ( #18929, #7411, #50184, #38222 ),
 .UNSPECIFIED., .F., .F.,
 ( 4, 4 ),
 ( 5.208685977958201486E-18, 0.009762429722931323731 ),
 .UNSPECIFIED. ) ;
#9691 = CARTESIAN_POINT ( 'NONE',  ( 46.75893035013449861, 17.89420872045614885, 3.199614146704519602 ) ) ;
#9692 = CARTESIAN_POINT ( 'NONE',  ( -4.945973446814903696, 2.143131898507912917E-16, 2.568287556928034121 ) ) ;
#9693 = LINE ( 'NONE', #45065, #14232 ) ;
#9694 = EDGE_LOOP ( 'NONE', ( #4665, #15751, #7304, #27447, #4501, #3224 ) ) ;
#9695 = DIRECTION ( 'NONE',  ( -1.000000000000000000, 0.000000000000000000, 0.000000000000000000 ) ) ;
#9696 = CARTESIAN_POINT ( 'NONE',  ( 350.0000000000001137, 181.0000000000000284, 343.9999999999997726 ) ) ;
#9697 = DIRECTION ( 'NONE',  ( -1.000000000000000000, -0.000000000000000000, -0.000000000000000000 ) ) ;
#9698 = ADVANCED_FACE ( 'NONE', ( #39712 ), #20195, .F. ) ;
#9699 = EDGE_LOOP ( 'NONE', ( #38299, #17940, #42655, #33434 ) ) ;
#9700 = DIRECTION ( 'NONE',  ( 0.000000000000000000, -0.000000000000000000, -1.000000000000000000 ) ) ;
#9701 = DIRECTION ( 'NONE',  ( -1.000000000000000000, 0.000000000000000000, -2.958228394578794270E-31 ) ) ;
#9702 = VERTEX_POINT ( 'NONE', #206 ) ;
#9703 = DIRECTION ( 'NONE',  ( -1.000000000000000000, 0.000000000000000000, -2.958228394578794270E-31 ) ) ;
#9704 = CARTESIAN_POINT ( 'NONE',  ( 0.000000000000000000, 17.00000000000000000, 0.000000000000000000 ) ) ;
#9705 = CARTESIAN_POINT ( 'NONE',  ( -126.6959734468149321, 0.000000000000000000, 165.0000000000000000 ) ) ;
#9706 = ORIENTED_EDGE ( 'NONE', *, *, #20839, .F. ) ;
#9707 = FACE_OUTER_BOUND ( 'NONE', #42896, .T. ) ;
#9708 = VERTEX_POINT ( 'NONE', #38268 ) ;
#9709 = ORIENTED_EDGE ( 'NONE', *, *, #40106, .F. ) ;
#9710 = LINE ( 'NONE', #2023, #22167 ) ;
#9711 = CIRCLE ( 'NONE', #13800, 2.000000000000001776 ) ;
#9712 = EDGE_LOOP ( 'NONE', ( #16727, #32001, #47507, #6952 ) ) ;
#9713 = CARTESIAN_POINT ( 'NONE',  ( 192.2789002873380184, -1.750000000000010214, 79.79316129108087807 ) ) ;
#9714 = DIRECTION ( 'NONE',  ( -0.000000000000000000, -0.000000000000000000, -1.000000000000000000 ) ) ;
#9715 = VERTEX_POINT ( 'NONE', #35115 ) ;
#9716 = DIRECTION ( 'NONE',  ( -0.000000000000000000, -0.000000000000000000, -1.000000000000000000 ) ) ;
#9717 = CYLINDRICAL_SURFACE ( 'NONE', #12761, 5.000000000000000000 ) ;
#9718 = DIRECTION ( 'NONE',  ( -1.000000000000000000, 4.996003610813203446E-16, 7.930164450086814785E-16 ) ) ;
#9719 = CARTESIAN_POINT ( 'NONE',  ( 181.0000000000000000, -174.9999999999999716, -358.0000000000001705 ) ) ;
#9720 = ORIENTED_EDGE ( 'NONE', *, *, #38891, .T. ) ;
#9721 = CARTESIAN_POINT ( 'NONE',  ( 349.9999999999999432, -180.9999999999999716, 359.9999999999997726 ) ) ;
#9722 = VERTEX_POINT ( 'NONE', #36120 ) ;
#9723 = DIRECTION ( 'NONE',  ( 1.000000000000000000, 0.000000000000000000, 1.612977847700450206E-50 ) ) ;
#9724 = CARTESIAN_POINT ( 'NONE',  ( 341.6568542494922553, 165.0000000000000284, -339.9999999999999432 ) ) ;
#9725 = ORIENTED_EDGE ( 'NONE', *, *, #36299, .T. ) ;
#9726 = EDGE_LOOP ( 'NONE', ( #14547, #21611, #21138, #1675, #35607, #27449, #16566, #22388, #33800, #5390, #34985, #37680, #42247, #3860, #26715, #16156, #34500 ) ) ;
#9727 = EDGE_LOOP ( 'NONE', ( #36338, #7751, #12589, #7986 ) ) ;
#9728 = CYLINDRICAL_SURFACE ( 'NONE', #35237, 1.750000000000001554 ) ;
#9729 = EDGE_CURVE ( 'NONE', #26100, #47737, #50689, .T. ) ;
#9730 = CARTESIAN_POINT ( 'NONE',  ( 350.0000000000001137, 181.0000000000000284, 357.9999999999997726 ) ) ;
#9731 = PRODUCT_DEFINITION_SHAPE ( 'NONE', 'NONE',  #48451 ) ;
#9732 = VERTEX_POINT ( 'NONE', #961 ) ;
#9733 = DIRECTION ( 'NONE',  ( 0.000000000000000000, 0.000000000000000000, 1.000000000000000000 ) ) ;
#9734 = CARTESIAN_POINT ( 'NONE',  ( 1.275971930252332243, -0.1228246474626390333, 9.957892297621015132 ) ) ;
#9735 = DIRECTION ( 'NONE',  ( 1.132880637372608740E-16, 4.718402560806925739E-50, 1.000000000000000000 ) ) ;
#9736 = DIRECTION ( 'NONE',  ( 0.000000000000000000, 0.000000000000000000, 1.000000000000000000 ) ) ;
#9737 = VERTEX_POINT ( 'NONE', #44031 ) ;
#9738 = CARTESIAN_POINT ( 'NONE',  ( 33.30402655318503946, 1.750000000000009992, 0.8182875569279768335 ) ) ;
#9739 = DIRECTION ( 'NONE',  ( -0.7233555441435719491, 0.6904757466825007794, -0.000000000000000000 ) ) ;
#9740 = CARTESIAN_POINT ( 'NONE',  ( -15.44803555374685189, -6.237487519713257100, -3.546734833711462365 ) ) ;
#9741 = ORIENTED_EDGE ( 'NONE', *, *, #33399, .T. ) ;
#9742 = ITEM_DEFINED_TRANSFORMATION ( 'NONE', 'NONE', #5345,  #45486 ) ;
#9743 = AXIS2_PLACEMENT_3D ( 'NONE', #22243, #21987, #37661 ) ;
#9744 = CARTESIAN_POINT ( 'NONE',  ( -204.9459734468148895, -1.025126265847089435, -40.93171244307204404 ) ) ;
#9745 = CARTESIAN_POINT ( 'NONE',  ( 1.365263087672787590, -0.5437404457008400138, 9.958264684458717042 ) ) ;
#9746 = CIRCLE ( 'NONE', #39255, 1.750000000000015543 ) ;
#9747 = CARTESIAN_POINT ( 'NONE',  ( -12.15085308559838317, 11.68662139125813226, 2.590526750877053086 ) ) ;
#9748 = CYLINDRICAL_SURFACE ( 'NONE', #1919, 1.750000000000015543 ) ;
#9749 = ORIENTED_EDGE ( 'NONE', *, *, #4856, .T. ) ;
#9750 = AXIS2_PLACEMENT_3D ( 'NONE', #21051, #36738, #12333 ) ;
#9751 = AXIS2_PLACEMENT_3D ( 'NONE', #29485, #44357, #6137 ) ;
#9752 = DIRECTION ( 'NONE',  ( -1.000000000000000000, -0.000000000000000000, -0.000000000000000000 ) ) ;
#9753 = DIRECTION ( 'NONE',  ( 0.000000000000000000, 0.000000000000000000, 1.000000000000000000 ) ) ;
#9754 = DIRECTION ( 'NONE',  ( -1.000000000000000000, 0.000000000000000000, 0.000000000000000000 ) ) ;
#9755 = DIRECTION ( 'NONE',  ( -0.000000000000000000, -0.000000000000000000, -1.000000000000000000 ) ) ;
#9756 = VECTOR ( 'NONE', #21804, 1000.000000000000000 ) ;
#9757 = PLANE ( 'NONE',  #17278 ) ;
#9758 = ADVANCED_FACE ( 'NONE', ( #13996 ), #9148, .T. ) ;
#9759 = AXIS2_PLACEMENT_3D ( 'NONE', #5418, #39843, #44645 ) ;
#9760 = EDGE_LOOP ( 'NONE', ( #39795, #29788, #24517 ) ) ;
#9761 = DIRECTION ( 'NONE',  ( -0.6805276818820399365, -0.4944323023722067556, -0.5407575913134975432 ) ) ;
#9762 = EDGE_LOOP ( 'NONE', ( #16186, #34761, #9461, #49324, #23687, #33579, #24922, #17561 ) ) ;
#9763 = CARTESIAN_POINT ( 'NONE',  ( -567.5000000000000000, 57.49999999999996447, -183.5999999999997954 ) ) ;
#9764 = ORIENTED_EDGE ( 'NONE', *, *, #36140, .T. ) ;
#9765 = DIRECTION ( 'NONE',  ( 0.000000000000000000, 0.000000000000000000, 1.000000000000000000 ) ) ;
#9766 = LINE ( 'NONE', #2082, #35627 ) ;
#9767 = ORIENTED_EDGE ( 'NONE', *, *, #13609, .F. ) ;
#9768 = CARTESIAN_POINT ( 'NONE',  ( 193.3040265531851105, -1.750000000000010658, 80.81828755692798438 ) ) ;
#9769 = ORIENTED_EDGE ( 'NONE', *, *, #1733, .F. ) ;
#9770 = CARTESIAN_POINT ( 'NONE',  ( 210.0000000000000568, 2.143131898507880377E-16, -0.9317124430720331585 ) ) ;
#9771 = CARTESIAN_POINT ( 'NONE',  ( 0.8590960553269455513, 0.9801595984304427578, 9.961915419665690052 ) ) ;
#9772 = CARTESIAN_POINT ( 'NONE',  ( 33.30402655318503946, 0.000000000000000000, -165.0000000000000000 ) ) ;
#9773 = DIRECTION ( 'NONE',  ( -1.000000000000000000, 0.000000000000000000, -0.000000000000000000 ) ) ;
#9774 = ORIENTED_EDGE ( 'NONE', *, *, #34082, .T. ) ;
#9775 = VERTEX_POINT ( 'NONE', #21199 ) ;
#9776 = CARTESIAN_POINT ( 'NONE',  ( 35.00000000000122213, 17.00000000000000000, 5.000000000000004441 ) ) ;
#9777 = VECTOR ( 'NONE', #14437, 1000.000000000000000 ) ;
#9778 = ORIENTED_EDGE ( 'NONE', *, *, #30694, .T. ) ;
#9779 = DIRECTION ( 'NONE',  ( -1.156482317317870492E-16, 1.000000000000000000, 0.000000000000000000 ) ) ;
#9780 = DIRECTION ( 'NONE',  ( 1.000000000000000000, -4.996003610813203446E-16, -1.586032878436834529E-16 ) ) ;
#9781 = ORIENTED_EDGE ( 'NONE', *, *, #43614, .F. ) ;
#9782 = DIRECTION ( 'NONE',  ( 0.4374820812098837997, -0.3178493372392718341, 0.8411784753765542133 ) ) ;
#9783 = VECTOR ( 'NONE', #1482, 1000.000000000000000 ) ;
#9784 = EDGE_CURVE ( 'NONE', #21642, #20088, #28904, .T. ) ;
#9785 = AXIS2_PLACEMENT_3D ( 'NONE', #18459, #21820, #9753 ) ;
#9786 = EDGE_LOOP ( 'NONE', ( #7195, #23163, #23264, #7541 ) ) ;
#9787 = CARTESIAN_POINT ( 'NONE',  ( -6.695973446814940111, -1.750000000000023315, -159.1817124430720298 ) ) ;
#9788 = CARTESIAN_POINT ( 'NONE',  ( -124.9459734468149463, 2.143131898507847836E-16, -40.93171244307202983 ) ) ;
#9789 = FACE_OUTER_BOUND ( 'NONE', #28115, .T. ) ;
#9790 = AXIS2_PLACEMENT_3D ( 'NONE', #50429, #23542, #15835 ) ;
#9791 = CARTESIAN_POINT ( 'NONE',  ( 113.3040265531850537, -1.749999999999997113, 40.81828755692798438 ) ) ;
#9792 = ORIENTED_EDGE ( 'NONE', *, *, #21807, .F. ) ;
#9793 = ORIENTED_EDGE ( 'NONE', *, *, #49891, .F. ) ;
#9794 = EDGE_LOOP ( 'NONE', ( #44512, #29118, #15117, #27789 ) ) ;
#9795 = CARTESIAN_POINT ( 'NONE',  ( -4.999999999999948486, -204.9999999999999716, -234.7500000000000000 ) ) ;
#9796 = CARTESIAN_POINT ( 'NONE',  ( 0.000000000000000000, -168.9999999999999432, -356.0000000000002274 ) ) ;
#9797 = EDGE_CURVE ( 'NONE', #30725, #6936, #36889, .T. ) ;
#9798 = LINE ( 'NONE', #49004, #24935 ) ;
#9799 = EDGE_CURVE ( 'NONE', #42832, #20659, #24809, .T. ) ;
#9800 = CARTESIAN_POINT ( 'NONE',  ( -1.066995270233474624, 33.23888904628638841, -3.760136334089591248 ) ) ;
#9801 = VERTEX_POINT ( 'NONE', #21701 ) ;
#9802 = CARTESIAN_POINT ( 'NONE',  ( -44.94597344681493922, 2.143131898507880377E-16, -160.9317124430720582 ) ) ;
#9803 = EDGE_LOOP ( 'NONE', ( #24500, #35219, #43473, #1925 ) ) ;
#9804 =( NAMED_UNIT ( * ) SI_UNIT ( $, .STERADIAN. ) SOLID_ANGLE_UNIT ( ) );
#9805 = ADVANCED_FACE ( 'NONE', ( #17352 ), #2261, .T. ) ;
#9806 = CARTESIAN_POINT ( 'NONE',  ( -8.277096487746778308, 33.14818118907697198, 7.455576670931136185 ) ) ;
#9807 = CARTESIAN_POINT ( 'NONE',  ( 165.0000000000000000, -174.9999999999999716, -99.00000000000014211 ) ) ;
#9808 = DIRECTION ( 'NONE',  ( -1.000000000000000000, 0.000000000000000000, -0.000000000000000000 ) ) ;
#9809 = DIRECTION ( 'NONE',  ( -1.000000000000000000, -0.000000000000000000, -0.000000000000000000 ) ) ;
#9810 = CARTESIAN_POINT ( 'NONE',  ( 360.0000000000000568, -166.6568542494925396, 341.6568542494923122 ) ) ;
#9811 = LINE ( 'NONE', #48521, #24010 ) ;
#9812 = ORIENTED_EDGE ( 'NONE', *, *, #2208, .T. ) ;
#9813 = CARTESIAN_POINT ( 'NONE',  ( 71.55402655318505367, 0.000000000000000000, 39.06828755692795596 ) ) ;
#9814 = CARTESIAN_POINT ( 'NONE',  ( 240.0000000000000000, -175.0000000000000000, 474.9999999999998863 ) ) ;
#9815 = LINE ( 'NONE', #25479, #45519 ) ;
#9816 = EDGE_CURVE ( 'NONE', #22449, #9166, #48607, .T. ) ;
#9817 = EDGE_CURVE ( 'NONE', #1522, #8172, #40960, .T. ) ;
#9818 = VECTOR ( 'NONE', #23089, 1000.000000000000000 ) ;
#9819 =( BOUNDED_CURVE ( )  B_SPLINE_CURVE ( 3, ( #46561, #22744, #46316, #26087 ),
 .UNSPECIFIED., .F., .F. ) 
 B_SPLINE_CURVE_WITH_KNOTS ( ( 4, 4 ),
 ( 4.712388980384689674, 6.283185307179586232 ),
 .UNSPECIFIED. ) 
 CURVE ( )  GEOMETRIC_REPRESENTATION_ITEM ( )  RATIONAL_B_SPLINE_CURVE ( ( 1.000000000000000000, 0.8047378541243649375, 0.8047378541243649375, 1.000000000000000000 ) ) 
 REPRESENTATION_ITEM ( '' )  );
#9820 = EDGE_CURVE ( 'NONE', #25937, #12379, #36640, .T. ) ;
#9821 = EDGE_CURVE ( 'NONE', #40512, #25153, #5179, .T. ) ;
#9822 = AXIS2_PLACEMENT_3D ( 'NONE', #11409, #49837, #42442 ) ;
#9823 = CARTESIAN_POINT ( 'NONE',  ( -125.6708471809678542, -1.749999999999996225, 1.843413822775058497 ) ) ;
#9824 = VERTEX_POINT ( 'NONE', #13746 ) ;
#9825 = CARTESIAN_POINT ( 'NONE',  ( -10.69268279052439574, -12.77266927778454964, -2.870787844569587133 ) ) ;
#9826 = ORIENTED_EDGE ( 'NONE', *, *, #15222, .T. ) ;
#9827 = AXIS2_PLACEMENT_3D ( 'NONE', #41542, #10492, #25646 ) ;
#9828 = FACE_OUTER_BOUND ( 'NONE', #42596, .T. ) ;
#9829 =( BOUNDED_CURVE ( )  B_SPLINE_CURVE ( 3, ( #3425, #49822, #23454, #14729 ),
 .UNSPECIFIED., .F., .F. ) 
 B_SPLINE_CURVE_WITH_KNOTS ( ( 4, 4 ),
 ( 4.712388980384689674, 6.283185307179586232 ),
 .UNSPECIFIED. ) 
 CURVE ( )  GEOMETRIC_REPRESENTATION_ITEM ( )  RATIONAL_B_SPLINE_CURVE ( ( 1.000000000000000000, 0.8047378541243649375, 0.8047378541243649375, 1.000000000000000000 ) ) 
 REPRESENTATION_ITEM ( '' )  );
#9830 = CARTESIAN_POINT ( 'NONE',  ( 74.32915281903215998, -1.750000000000009326, 1.843413822775066269 ) ) ;
#9831 = EDGE_CURVE ( 'NONE', #29600, #29991, #26159, .T. ) ;
#9832 = CARTESIAN_POINT ( 'NONE',  ( 339.9999999999999432, -182.9999999999999716, -356.0000000000002274 ) ) ;
#9833 = VECTOR ( 'NONE', #42899, 1000.000000000000000 ) ;
#9834 = CARTESIAN_POINT ( 'NONE',  ( 73.30402655318508209, 0.000000000000000000, 165.0000000000000000 ) ) ;
#9835 = FACE_OUTER_BOUND ( 'NONE', #42939, .T. ) ;
#9836 = LINE ( 'NONE', #18277, #36051 ) ;
#9837 = CARTESIAN_POINT ( 'NONE',  ( -8.277096487746778308, 50.00000000000000000, 7.455576670931136185 ) ) ;
#9838 =( BOUNDED_CURVE ( )  B_SPLINE_CURVE ( 3, ( #3797, #19444, #3278, #45350 ),
 .UNSPECIFIED., .F., .F. ) 
 B_SPLINE_CURVE_WITH_KNOTS ( ( 4, 4 ),
 ( 4.712388980384689674, 6.283185307179586232 ),
 .UNSPECIFIED. ) 
 CURVE ( )  GEOMETRIC_REPRESENTATION_ITEM ( )  RATIONAL_B_SPLINE_CURVE ( ( 1.000000000000000000, 0.8047378541243649375, 0.8047378541243649375, 1.000000000000000000 ) ) 
 REPRESENTATION_ITEM ( '' )  );
#9839 = VERTEX_POINT ( 'NONE', #24553 ) ;
#9840 = ORIENTED_EDGE ( 'NONE', *, *, #22462, .F. ) ;
#9841 = ADVANCED_FACE ( 'NONE', ( #40205 ), #36264, .T. ) ;
#9842 = PLANE ( 'NONE',  #30817 ) ;
#9843 = CARTESIAN_POINT ( 'NONE',  ( -114.9999999999997158, 17.00000000000000000, -84.99999999999998579 ) ) ;
#9844 = EDGE_CURVE ( 'NONE', #29454, #17433, #49610, .T. ) ;
#9845 = ORIENTED_EDGE ( 'NONE', *, *, #43751, .T. ) ;
#9846 = EDGE_CURVE ( 'NONE', #41166, #6332, #42455, .T. ) ;
#9847 = ORIENTED_EDGE ( 'NONE', *, *, #36191, .T. ) ;
#9848 = CARTESIAN_POINT ( 'NONE',  ( 0.000000000000000000, 0.000000000000000000, 0.000000000000000000 ) ) ;
#9849 = CARTESIAN_POINT ( 'NONE',  ( -86.69597344681496054, 0.000000000000000000, 165.0000000000000000 ) ) ;
#9850 = CARTESIAN_POINT ( 'NONE',  ( -205.6708471809678827, 1.750000000000010214, 79.79316129108087807 ) ) ;
#9851 = VERTEX_POINT ( 'NONE', #10908 ) ;
#9852 = EDGE_CURVE ( 'NONE', #15608, #25523, #30679, .T. ) ;
#9853 = ORIENTED_EDGE ( 'NONE', *, *, #11385, .T. ) ;
#9854 = CIRCLE ( 'NONE', #2455, 0.4999999999999997224 ) ;
#9855 = EDGE_CURVE ( 'NONE', #20536, #16093, #25815, .T. ) ;
#9856 = CARTESIAN_POINT ( 'NONE',  ( 0.5000000000000000000, -0.5000000000000000000, 1000.000000000000000 ) ) ;
#9857 = VECTOR ( 'NONE', #41189, 1000.000000000000000 ) ;
#9858 = LINE ( 'NONE', #41155, #38034 ) ;
#9859 = CIRCLE ( 'NONE', #38563, 0.4999999999999997224 ) ;
#9860 = ORIENTED_EDGE ( 'NONE', *, *, #45089, .T. ) ;
#9861 = ORIENTED_EDGE ( 'NONE', *, *, #28193, .F. ) ;
#9862 = CIRCLE ( 'NONE', #33617, 2.000000000000001776 ) ;
#9863 = CYLINDRICAL_SURFACE ( 'NONE', #20139, 1.750000000000008438 ) ;
#9864 = CARTESIAN_POINT ( 'NONE',  ( -206.6959734468149463, 1.750000000000009992, -159.1817124430720298 ) ) ;
#9865 = ORIENTED_EDGE ( 'NONE', *, *, #19874, .T. ) ;
#9866 = VECTOR ( 'NONE', #26417, 1000.000000000000000 ) ;
#9867 = ORIENTED_EDGE ( 'NONE', *, *, #25812, .T. ) ;
#9868 = CARTESIAN_POINT ( 'NONE',  ( -125.6708471809678542, 1.749999999999996669, 39.79316129108089228 ) ) ;
#9869 = CARTESIAN_POINT ( 'NONE',  ( -15.39115647749013505, 6.484697992489888208, -9.458680755252684591 ) ) ;
#9870 = ORIENTED_EDGE ( 'NONE', *, *, #11133, .F. ) ;
#9871 = CARTESIAN_POINT ( 'NONE',  ( 0.000000000000000000, 0.000000000000000000, 10.00000000000000000 ) ) ;
#9872 = FACE_OUTER_BOUND ( 'NONE', #41409, .T. ) ;
#9873 = CYLINDRICAL_SURFACE ( 'NONE', #21922, 4.000000000000003553 ) ;
#9874 = CARTESIAN_POINT ( 'NONE',  ( 153.3040265531850537, 1.750000000000009992, -159.1817124430720298 ) ) ;
#9875 = EDGE_CURVE ( 'NONE', #9063, #9286, #41460, .T. ) ;
#9876 = DIRECTION ( 'NONE',  ( 0.000000000000000000, 2.537652627714642000E-15, 1.000000000000000000 ) ) ;
#9877 = ORIENTED_EDGE ( 'NONE', *, *, #12, .F. ) ;
#9878 = DIRECTION ( 'NONE',  ( 0.000000000000000000, 0.000000000000000000, 1.000000000000000000 ) ) ;
#9879 = CARTESIAN_POINT ( 'NONE',  ( 0.3862712429686727678, 1.188820645368945605, 10.00000000000000000 ) ) ;
#9880 = CARTESIAN_POINT ( 'NONE',  ( 1.011271242968683648, 0.7347315653655930312, 10.00000000000000000 ) ) ;
#9881 = CARTESIAN_POINT ( 'NONE',  ( 44.99506233596246574, 23.32283626942318477, 7.455576670931136185 ) ) ;
#9882 = ADVANCED_FACE ( 'NONE', ( #6317 ), #2949, .T. ) ;
#9883 = EDGE_CURVE ( 'NONE', #11818, #3838, #38134, .T. ) ;
#9884 = EDGE_CURVE ( 'NONE', #29962, #375, #14507, .T. ) ;
#9885 = CYLINDRICAL_SURFACE ( 'NONE', #27333, 1.750000000000036193 ) ;
#9886 = CARTESIAN_POINT ( 'NONE',  ( 3.627208138665139803, 0.000000000000000000, 0.000000000000000000 ) ) ;
#9887 = ADVANCED_FACE ( 'NONE', ( #46276 ), #34797, .T. ) ;
#9888 = LINE ( 'NONE', #41181, #46592 ) ;
#9889 = CARTESIAN_POINT ( 'NONE',  ( -0.9390173899430289683, -1.130417317737636651, 9.958264684458541183 ) ) ;
#9890 = EDGE_CURVE ( 'NONE', #35501, #32520, #28070, .T. ) ;
#9891 = CARTESIAN_POINT ( 'NONE',  ( 16.15814872688565984, 4.048305257546810587, -2.870787844569587133 ) ) ;
#9892 = CIRCLE ( 'NONE', #26276, 0.5000000000000004441 ) ;
#9893 = EDGE_LOOP ( 'NONE', ( #38931, #16511, #24800, #25278 ) ) ;
#9894 = CARTESIAN_POINT ( 'NONE',  ( 164.9999999999999716, 17.00000000000000000, 90.00000000000000000 ) ) ;
#9895 = VECTOR ( 'NONE', #44217, 1000.000000000000000 ) ;
#9896 = CARTESIAN_POINT ( 'NONE',  ( 3.345242017215822372, -2.159124855890657724, -4.878909776184769953E-16 ) ) ;
#9897 = CARTESIAN_POINT ( 'NONE',  ( 115.0540265531850395, 2.143131898507847836E-16, -77.43171244307204404 ) ) ;
#9898 = CARTESIAN_POINT ( 'NONE',  ( 23.29043492822826167, -24.10797434788167948, 1.847720168420772691 ) ) ;
#9899 = CYLINDRICAL_SURFACE ( 'NONE', #47884, 1.750000000000008438 ) ;
#9900 = VERTEX_POINT ( 'NONE', #10657 ) ;
#9901 = DIRECTION ( 'NONE',  ( -0.000000000000000000, -0.000000000000000000, -1.000000000000000000 ) ) ;
#9902 = VECTOR ( 'NONE', #38432, 1000.000000000000000 ) ;
#9903 = ORIENTED_EDGE ( 'NONE', *, *, #46373, .F. ) ;
#9904 = DIRECTION ( 'NONE',  ( 1.000000000000000000, 0.000000000000000000, 0.000000000000000000 ) ) ;
#9905 = EDGE_LOOP ( 'NONE', ( #12263, #3205, #23516, #26832, #35487, #11554 ) ) ;
#9906 = EDGE_CURVE ( 'NONE', #47750, #47029, #3196, .T. ) ;
#9907 = LINE ( 'NONE', #26324, #44233 ) ;
#9908 = DIRECTION ( 'NONE',  ( 0.000000000000000000, 0.000000000000000000, 1.000000000000000000 ) ) ;
#9909 = ORIENTED_EDGE ( 'NONE', *, *, #7485, .T. ) ;
#9910 = VERTEX_POINT ( 'NONE', #11180 ) ;
#9911 = ORIENTED_EDGE ( 'NONE', *, *, #10448, .F. ) ;
#9912 = PRODUCT_RELATED_PRODUCT_CATEGORY ( 'part', '', ( #29832 ) ) ;
#9913 = CARTESIAN_POINT ( 'NONE',  ( -1.249999999999999778, 0.000000000000000000, -3.333333333333333481 ) ) ;
#9914 = CARTESIAN_POINT ( 'NONE',  ( -208.4459734468149463, 0.000000000000000000, -40.93171244307202983 ) ) ;
#9915 = LINE ( 'NONE', #26074, #11981 ) ;
#9916 = ORIENTED_EDGE ( 'NONE', *, *, #26682, .T. ) ;
#9917 = DIRECTION ( 'NONE',  ( -0.1191452206184309970, 0.000000000000000000, 0.9928768384869220975 ) ) ;
#9918 = CARTESIAN_POINT ( 'NONE',  ( 210.0000000000000568, 0.000000000000000000, -159.1817124430720298 ) ) ;
#9919 = CARTESIAN_POINT ( 'NONE',  ( 24.39427009665985224, 44.07992421011656603, 8.807470649214879543 ) ) ;
#9920 = ORIENTED_EDGE ( 'NONE', *, *, #21525, .T. ) ;
#9921 =( BOUNDED_CURVE ( )  B_SPLINE_CURVE ( 3, ( #36219, #810, #35968, #50605 ),
 .UNSPECIFIED., .F., .F. ) 
 B_SPLINE_CURVE_WITH_KNOTS ( ( 4, 4 ),
 ( 4.712388980384689674, 6.283185307179586232 ),
 .UNSPECIFIED. ) 
 CURVE ( )  GEOMETRIC_REPRESENTATION_ITEM ( )  RATIONAL_B_SPLINE_CURVE ( ( 1.000000000000000000, 0.8047378541243649375, 0.8047378541243649375, 1.000000000000000000 ) ) 
 REPRESENTATION_ITEM ( '' )  );
#9922 = ORIENTED_EDGE ( 'NONE', *, *, #20027, .T. ) ;
#9923 = PLANE ( 'NONE',  #10667 ) ;
#9924 = EDGE_CURVE ( 'NONE', #4803, #15022, #36377, .T. ) ;
#9925 = CARTESIAN_POINT ( 'NONE',  ( 113.3040265531850537, -1.749999999999997335, 120.8182875569279702 ) ) ;
#9926 = CARTESIAN_POINT ( 'NONE',  ( -84.94597344681494633, 2.143131898507880377E-16, 165.0000000000000000 ) ) ;
#9927 = ORIENTED_EDGE ( 'NONE', *, *, #39600, .T. ) ;
#9928 = CIRCLE ( 'NONE', #14021, 2.000000000000001776 ) ;
#9929 = DIRECTION ( 'NONE',  ( -0.000000000000000000, -0.000000000000000000, -1.000000000000000000 ) ) ;
#9930 = CARTESIAN_POINT ( 'NONE',  ( -36.08557433729204433, 35.58569447144795106, 7.455576670931136185 ) ) ;
#9931 = CARTESIAN_POINT ( 'NONE',  ( -48.44597344681495343, 0.000000000000000000, -165.0000000000000000 ) ) ;
#9932 = PLANE ( 'NONE',  #41906 ) ;
#9933 =( REPRESENTATION_RELATIONSHIP ('NONE','NONE', #45699, #35275 ) REPRESENTATION_RELATIONSHIP_WITH_TRANSFORMATION ( #48454 )SHAPE_REPRESENTATION_RELATIONSHIP( ) );
#9934 = ADVANCED_FACE ( 'NONE', ( #18101 ), #37883, .F. ) ;
#9935 = DIRECTION ( 'NONE',  ( 1.000000000000000000, -0.000000000000000000, 0.000000000000000000 ) ) ;
#9936 = CARTESIAN_POINT ( 'NONE',  ( -206.6959734468149463, -1.750000000000010658, -79.18171244307201562 ) ) ;
#9937 = VECTOR ( 'NONE', #35011, 1000.000000000000000 ) ;
#9938 = CARTESIAN_POINT ( 'NONE',  ( 1.011271242968694084, -0.7347315653655782652, -10.00000000000000000 ) ) ;
#9939 = CARTESIAN_POINT ( 'NONE',  ( -208.4459734468148611, 1.025126265847089213, -160.9317124430720014 ) ) ;
#9940 = VECTOR ( 'NONE', #45585, 1000.000000000000000 ) ;
#9941 = FACE_BOUND ( 'NONE', #37580, .T. ) ;
#9942 = DIRECTION ( 'NONE',  ( -1.000000000000000000, -0.000000000000000000, -0.000000000000000000 ) ) ;
#9943 = EDGE_CURVE ( 'NONE', #32080, #26268, #45531, .T. ) ;
#9944 = EDGE_CURVE ( 'NONE', #3012, #49797, #41593, .T. ) ;
#9945 = CARTESIAN_POINT ( 'NONE',  ( 0.000000000000000000, 175.0000000000000284, 350.0000000000002274 ) ) ;
#9946 = EDGE_LOOP ( 'NONE', ( #39923, #4159, #37574, #33449 ) ) ;
#9947 = CARTESIAN_POINT ( 'NONE',  ( -205.6708471809678827, -1.750000000000009548, 81.84341382277507648 ) ) ;
#9948 = EDGE_CURVE ( 'NONE', #37343, #16704, #29453, .T. ) ;
#9949 = CARTESIAN_POINT ( 'NONE',  ( -175.0000000000000000, 15.00000000000000000, -122.5000000000000000 ) ) ;
#9950 = LINE ( 'NONE', #2506, #4165 ) ;
#9951 = EDGE_CURVE ( 'NONE', #46103, #11178, #23989, .T. ) ;
#9952 = EDGE_CURVE ( 'NONE', #35009, #339, #26147, .T. ) ;
#9953 = ORIENTED_EDGE ( 'NONE', *, *, #46124, .F. ) ;
#9954 = B_SPLINE_CURVE_WITH_KNOTS ( 'NONE', 3,
 ( #21306, #6659, #29766, #14364 ),
 .UNSPECIFIED., .F., .F.,
 ( 4, 4 ),
 ( 0.000000000000000000, 0.2637263876330693813 ),
 .UNSPECIFIED. ) ;
#9955 = CARTESIAN_POINT ( 'NONE',  ( -0.6108107228405769140, 1.056024183042602482, 9.963925895596188909 ) ) ;
#9956 = ORIENTED_EDGE ( 'NONE', *, *, #9944, .F. ) ;
#9957 = CARTESIAN_POINT ( 'NONE',  ( 349.9999999999999432, -164.9999999999999432, 355.9999999999997726 ) ) ;
#9958 = FACE_OUTER_BOUND ( 'NONE', #25464, .T. ) ;
#9959 = DIRECTION ( 'NONE',  ( 0.000000000000000000, -1.000000000000000000, 0.000000000000000000 ) ) ;
#9960 = DIRECTION ( 'NONE',  ( 0.000000000000000000, -1.000000000000000000, 1.604368532695312981E-16 ) ) ;
#9961 = AXIS2_PLACEMENT_3D ( 'NONE', #14523, #48874, #30175 ) ;
#9962 = ADVANCED_FACE ( 'NONE', ( #35303 ), #8345, .T. ) ;
#9963 = ORIENTED_EDGE ( 'NONE', *, *, #9586, .F. ) ;
#9964 = LINE ( 'NONE', #28713, #12594 ) ;
#9965 = VERTEX_POINT ( 'NONE', #43226 ) ;
#9966 = ORIENTED_EDGE ( 'NONE', *, *, #10574, .F. ) ;
#9967 = DIRECTION ( 'NONE',  ( 0.000000000000000000, -1.000000000000000000, 0.000000000000000000 ) ) ;
#9968 = EDGE_LOOP ( 'NONE', ( #35188, #31710, #6042, #18245 ) ) ;
#9969 = AXIS2_PLACEMENT_3D ( 'NONE', #4464, #17019, #48022 ) ;
#9970 = CARTESIAN_POINT ( 'NONE',  ( -167.4999999999999432, -112.5000000000000000, -10.00000000000000000 ) ) ;
#9971 = CARTESIAN_POINT ( 'NONE',  ( -166.6959734468149463, 1.750000000000009992, 160.8182875569279702 ) ) ;
#9972 = VERTEX_POINT ( 'NONE', #39644 ) ;
#9973 = CARTESIAN_POINT ( 'NONE',  ( 181.0000000000000284, 2.775557561562891351E-14, -111.0000000000001563 ) ) ;
#9974 = AXIS2_PLACEMENT_3D ( 'NONE', #42015, #38688, #30212 ) ;
#9975 = CARTESIAN_POINT ( 'NONE',  ( 168.9999999999999716, -93.49999999999997158, -115.0000000000001563 ) ) ;
#9976 = VERTEX_POINT ( 'NONE', #3972 ) ;
#9977 = DIRECTION ( 'NONE',  ( -1.000000000000000000, -0.000000000000000000, -0.000000000000000000 ) ) ;
#9978 = CYLINDRICAL_SURFACE ( 'NONE', #13472, 4.000000000000003553 ) ;
#9979 = LINE ( 'NONE', #17915, #29153 ) ;
#9980 =( BOUNDED_CURVE ( )  B_SPLINE_CURVE ( 3, ( #7203, #3335, #45659, #26949 ),
 .UNSPECIFIED., .F., .F. ) 
 B_SPLINE_CURVE_WITH_KNOTS ( ( 4, 4 ),
 ( 1.570796326794896558, 3.141592653589793116 ),
 .UNSPECIFIED. ) 
 CURVE ( )  GEOMETRIC_REPRESENTATION_ITEM ( )  RATIONAL_B_SPLINE_CURVE ( ( 1.000000000000000000, 0.8047378541243649375, 0.8047378541243649375, 1.000000000000000000 ) ) 
 REPRESENTATION_ITEM ( '' )  );
#9981 = ORIENTED_EDGE ( 'NONE', *, *, #38433, .F. ) ;
#9982 = B_SPLINE_CURVE_WITH_KNOTS ( 'NONE', 3,
 ( #42087, #6951, #38279, #3089 ),
 .UNSPECIFIED., .F., .F.,
 ( 4, 4 ),
 ( 2.424349759030540154E-19, 0.0003407397535652242774 ),
 .UNSPECIFIED. ) ;
#9983 = LINE ( 'NONE', #49188, #7124 ) ;
#9984 = DIRECTION ( 'NONE',  ( 1.000000000000000000, 0.000000000000000000, 0.000000000000000000 ) ) ;
#9985 = ORIENTED_EDGE ( 'NONE', *, *, #14576, .F. ) ;
#9986 = ORIENTED_EDGE ( 'NONE', *, *, #9992, .T. ) ;
#9987 = EDGE_LOOP ( 'NONE', ( #7263, #32871, #12133, #17955 ) ) ;
#9988 = FACE_OUTER_BOUND ( 'NONE', #8102, .T. ) ;
#9989 =( BOUNDED_CURVE ( )  B_SPLINE_CURVE ( 3, ( #15500, #3436, #39385, #34256 ),
 .UNSPECIFIED., .F., .F. ) 
 B_SPLINE_CURVE_WITH_KNOTS ( ( 4, 4 ),
 ( 1.570796326794896558, 3.141592653589793116 ),
 .UNSPECIFIED. ) 
 CURVE ( )  GEOMETRIC_REPRESENTATION_ITEM ( )  RATIONAL_B_SPLINE_CURVE ( ( 1.000000000000000000, 0.8047378541243649375, 0.8047378541243649375, 1.000000000000000000 ) ) 
 REPRESENTATION_ITEM ( '' )  );
#9990 = DIRECTION ( 'NONE',  ( -1.000000000000000000, -0.000000000000000000, -0.000000000000000000 ) ) ;
#9991 = ORIENTED_EDGE ( 'NONE', *, *, #28142, .F. ) ;
#9992 = EDGE_CURVE ( 'NONE', #47482, #49500, #47295, .T. ) ;
#9993 = CARTESIAN_POINT ( 'NONE',  ( -206.6959734468149463, 1.750000000000010658, 80.81828755692798438 ) ) ;
#9994 = LINE ( 'NONE', #33608, #18028 ) ;
#9995 = CARTESIAN_POINT ( 'NONE',  ( -0.9494396179258391966, 9.954826186926261755, 9.646707543097345905 ) ) ;
#9996 = CARTESIAN_POINT ( 'NONE',  ( 73.30402655318508209, 0.000000000000000000, -165.0000000000000000 ) ) ;
#9997 = ORIENTED_EDGE ( 'NONE', *, *, #3987, .F. ) ;
#9998 = CARTESIAN_POINT ( 'NONE',  ( 30.00000000000153833, 16.00000000000000000, 60.00000000000000000 ) ) ;
#9999 = CARTESIAN_POINT ( 'NONE',  ( 1.222012661920449439, -0.2471648704738783342, 9.981352469109934233 ) ) ;
#10000 = VECTOR ( 'NONE', #50518, 1000.000000000000000 ) ;
#10001 = FACE_OUTER_BOUND ( 'NONE', #20278, .T. ) ;
#10002 = MECHANICAL_DESIGN_GEOMETRIC_PRESENTATION_REPRESENTATION (  '', ( #46960 ), #16568 ) ;
#10003 = EDGE_LOOP ( 'NONE', ( #12347, #29026, #40817, #10752, #8995, #46287, #43627, #35979 ) ) ;
#10004 = DIRECTION ( 'NONE',  ( 0.000000000000000000, 0.000000000000000000, -1.000000000000000000 ) ) ;
#10005 = CARTESIAN_POINT ( 'NONE',  ( 11.73320209285708415, -11.96063479729170886, 9.403735324607438884 ) ) ;
#10006 = EDGE_CURVE ( 'NONE', #7917, #9972, #43474, .T. ) ;
#10007 = ADVANCED_FACE ( 'NONE', ( #31443 ), #8092, .F. ) ;
#10008 = VECTOR ( 'NONE', #16046, 1000.000000000000000 ) ;
#10009 = CARTESIAN_POINT ( 'NONE',  ( -1.456734136747265929, 2.915208416222881294, 9.799352050262545077 ) ) ;
#10010 = DIRECTION ( 'NONE',  ( -0.000000000000000000, -0.000000000000000000, -1.000000000000000000 ) ) ;
#10011 = ORIENTED_EDGE ( 'NONE', *, *, #2294, .F. ) ;
#10012 = CARTESIAN_POINT ( 'NONE',  ( 210.0000000000000568, 0.000000000000000000, -77.43171244307200141 ) ) ;
#10013 = PLANE ( 'NONE',  #40935 ) ;
#10014 = CYLINDRICAL_SURFACE ( 'NONE', #10552, 1.750000000000008438 ) ;
#10015 = CARTESIAN_POINT ( 'NONE',  ( -6.875132362119187768, 33.14667368551891258, 8.356839323120299312 ) ) ;
#10016 = CARTESIAN_POINT ( 'NONE',  ( 344.0000000000000000, 174.9999999999996589, -344.0000000000002842 ) ) ;
#10017 = B_SPLINE_CURVE_WITH_KNOTS ( 'NONE', 3,
 ( #18288, #30369, #45217, #38078 ),
 .UNSPECIFIED., .F., .F.,
 ( 4, 4 ),
 ( 0.0007271047118230567798, 0.006865190725605201105 ),
 .UNSPECIFIED. ) ;
#10018 = ADVANCED_FACE ( 'NONE', ( #46778 ), #15525, .T. ) ;
#10019 = EDGE_CURVE ( 'NONE', #48624, #30357, #16041, .T. ) ;
#10020 = ORIENTED_EDGE ( 'NONE', *, *, #35555, .T. ) ;
#10021 = CARTESIAN_POINT ( 'NONE',  ( 356.0000000000001137, 183.0000000000000284, 357.9999999999998295 ) ) ;
#10022 = ORIENTED_EDGE ( 'NONE', *, *, #19513, .F. ) ;
#10023 = DIRECTION ( 'NONE',  ( 1.860490536778032451E-50, 0.000000000000000000, -1.000000000000000000 ) ) ;
#10024 = ORIENTED_EDGE ( 'NONE', *, *, #13089, .F. ) ;
#10025 = EDGE_CURVE ( 'NONE', #48660, #31445, #31189, .T. ) ;
#10026 = CARTESIAN_POINT ( 'NONE',  ( -7.721099712662037540, -1.750000000000023315, 41.84341382277508359 ) ) ;
#10027 = CARTESIAN_POINT ( 'NONE',  ( 35.00000000000028422, 17.00000000000000000, -60.00000000000000000 ) ) ;
#10028 = AXIS2_PLACEMENT_3D ( 'NONE', #44974, #21396, #45475 ) ;
#10029 = LINE ( 'NONE', #5667, #319 ) ;
#10030 = ORIENTED_EDGE ( 'NONE', *, *, #19397, .T. ) ;
#10031 = CARTESIAN_POINT ( 'NONE',  ( 192.2789002873380184, -1.750000000000010214, 81.84341382277507648 ) ) ;
#10032 = ORIENTED_EDGE ( 'NONE', *, *, #3320, .T. ) ;
#10033 = CARTESIAN_POINT ( 'NONE',  ( 192.2789002873380184, -1.750000000000010214, -80.20683870891910772 ) ) ;
#10034 = CARTESIAN_POINT ( 'NONE',  ( -9.999999999999994671, 2.168404344971008375E-16, 8.340239149799208107 ) ) ;
#10035 = COLOUR_RGB ( '',0.7921568627450980005, 0.8196078431372548767, 0.9333333333333333481 ) ;
#10036 = CARTESIAN_POINT ( 'NONE',  ( 115.0540265531850395, 2.143131898507847836E-16, -157.4317124430720582 ) ) ;
#10037 = CARTESIAN_POINT ( 'NONE',  ( -119.9999999999984652, 16.00000000000000000, 35.00000000000000000 ) ) ;
#10038 = VECTOR ( 'NONE', #45235, 1000.000000000000000 ) ;
#10039 = CARTESIAN_POINT ( 'NONE',  ( 210.0000000000000568, 2.143131898507880377E-16, -160.9317124430720298 ) ) ;
#10040 = ORIENTED_EDGE ( 'NONE', *, *, #12961, .F. ) ;
#10041 = VERTEX_POINT ( 'NONE', #24250 ) ;
#10042 = CARTESIAN_POINT ( 'NONE',  ( 196.8526953830862567, 2.688010569040066411, 472.8425600500171981 ) ) ;
#10043 = CIRCLE ( 'NONE', #44447, 0.5000000000000004441 ) ;
#10044 = ORIENTED_EDGE ( 'NONE', *, *, #8013, .T. ) ;
#10045 = DIRECTION ( 'NONE',  ( 0.000000000000000000, -0.4436251537532894806, 0.8962124318248270161 ) ) ;
#10046 = CARTESIAN_POINT ( 'NONE',  ( -128.4459734468149463, -1.025126265847082108, 122.5682875569279702 ) ) ;
#10047 = EDGE_LOOP ( 'NONE', ( #11824, #3912, #37045, #19623, #23247, #48530 ) ) ;
#10048 = DIRECTION ( 'NONE',  ( 0.000000000000000000, 0.000000000000000000, 1.000000000000000000 ) ) ;
#10049 = FACE_OUTER_BOUND ( 'NONE', #30015, .T. ) ;
#10050 = B_SPLINE_SURFACE_WITH_KNOTS ( 'NONE', 3, 3, ( 
 ( #5738, #1902, #48548, #17549 ),
 ( #8842, #29101, #44720, #24498 ),
 ( #33221, #48805, #13691, #12927 ),
 ( #28587, #36578, #1407, #17042 ) ),
 .UNSPECIFIED., .F., .F., .F.,
 ( 4, 4 ),
 ( 4, 4 ),
 ( 0.000000000000000000, 1.000000000000000000 ),
 ( 0.000000000000000000, 1.000000000000000000 ),
 .UNSPECIFIED. ) ;
#10051 = VERTEX_POINT ( 'NONE', #39906 ) ;
#10052 = LINE ( 'NONE', #41352, #22714 ) ;
#10053 = EDGE_CURVE ( 'NONE', #3893, #13210, #37808, .T. ) ;
#10054 = DIRECTION ( 'NONE',  ( 0.000000000000000000, 5.664403186863042467E-17, 1.000000000000000000 ) ) ;
#10055 = DIRECTION ( 'NONE',  ( 1.132880637372608740E-16, 4.718402560806925739E-50, 1.000000000000000000 ) ) ;
#10056 = CARTESIAN_POINT ( 'NONE',  ( -205.6708471809678827, 1.750000000000009548, 161.8434138227750907 ) ) ;
#10057 = DIRECTION ( 'NONE',  ( -0.000000000000000000, 0.2223603367690637489, 0.9749645535258953943 ) ) ;
#10058 = VERTEX_POINT ( 'NONE', #4736 ) ;
#10059 = ORIENTED_EDGE ( 'NONE', *, *, #15093, .T. ) ;
#10060 = CARTESIAN_POINT ( 'NONE',  ( 153.3040265531850537, 1.750000000000010214, -39.18171244307202983 ) ) ;
#10061 = DIRECTION ( 'NONE',  ( -7.793956916774525800E-48, 0.000000000000000000, -1.000000000000000000 ) ) ;
#10062 = DIRECTION ( 'NONE',  ( -1.000000000000000000, 4.996003610813203446E-16, -1.033975765691284410E-24 ) ) ;
#10063 = VECTOR ( 'NONE', #9780, 1000.000000000000000 ) ;
#10064 = CARTESIAN_POINT ( 'NONE',  ( 358.3431457505076310, -164.9999999999999432, 339.9999999999998295 ) ) ;
#10065 = ORIENTED_EDGE ( 'NONE', *, *, #13074, .T. ) ;
#10066 = CARTESIAN_POINT ( 'NONE',  ( 0.000000000000000000, 181.0000000000000284, -344.0000000000001705 ) ) ;
#10067 = EDGE_LOOP ( 'NONE', ( #48538, #11928, #40802, #4409 ) ) ;
#10068 = LINE ( 'NONE', #29318, #3182 ) ;
#10069 = DIRECTION ( 'NONE',  ( 1.000000000000000000, 0.000000000000000000, 0.000000000000000000 ) ) ;
#10070 = DIRECTION ( 'NONE',  ( 0.000000000000000000, 0.000000000000000000, 1.000000000000000000 ) ) ;
#10071 = DIRECTION ( 'NONE',  ( -1.000000000000000000, -0.000000000000000000, -0.000000000000000000 ) ) ;
#10072 = DIRECTION ( 'NONE',  ( 0.8637789008984335659, -0.000000000000000000, 0.5038710255240859137 ) ) ;
#10073 = DIRECTION ( 'NONE',  ( -0.000000000000000000, -0.000000000000000000, -1.000000000000000000 ) ) ;
#10074 = ORIENTED_EDGE ( 'NONE', *, *, #26140, .F. ) ;
#10075 = CARTESIAN_POINT ( 'NONE',  ( 1.052829316634732892, 0.8818324942345726614, 9.946805383069621698 ) ) ;
#10076 = AXIS2_PLACEMENT_3D ( 'NONE', #3303, #38237, #46116 ) ;
#10077 = DIRECTION ( 'NONE',  ( 0.000000000000000000, 0.000000000000000000, -1.000000000000000000 ) ) ;
#10078 = CARTESIAN_POINT ( 'NONE',  ( 370.7621192902014968, 103.1142457376053727, -17.29493270523947501 ) ) ;
#10079 = VECTOR ( 'NONE', #9449, 1000.000000000000000 ) ;
#10080 = DIRECTION ( 'NONE',  ( 0.000000000000000000, 1.000000000000000000, 0.000000000000000000 ) ) ;
#10081 = ORIENTED_EDGE ( 'NONE', *, *, #32277, .T. ) ;
#10083 = B_SPLINE_CURVE_WITH_KNOTS ( 'NONE', 3,
 ( #16296, #28593, #39653, #17048 ),
 .UNSPECIFIED., .F., .F.,
 ( 4, 4 ),
 ( 3.824224708052577823E-16, 0.009762429722931321996 ),
 .UNSPECIFIED. ) ;
#10082 = VECTOR ( 'NONE', #31039, 1000.000000000000000 ) ;
#10084 = CARTESIAN_POINT ( 'NONE',  ( -12.16428377685542017, -11.73151505502925929, -9.008049429158100807 ) ) ;
#10085 = ORIENTED_EDGE ( 'NONE', *, *, #14919, .T. ) ;
#10086 = ADVANCED_FACE ( 'NONE', ( #27072 ), #42704, .T. ) ;
#10087 = CARTESIAN_POINT ( 'NONE',  ( 0.000000000000000000, 17.00000000000000000, 0.000000000000000000 ) ) ;
#10088 = FACE_OUTER_BOUND ( 'NONE', #47952, .T. ) ;
#10089 = FACE_OUTER_BOUND ( 'NONE', #12232, .T. ) ;
#10090 = CARTESIAN_POINT ( 'NONE',  ( 24.39427009665985224, 44.07992421011656603, 8.807470649214879543 ) ) ;
#10091 = ORIENTED_EDGE ( 'NONE', *, *, #49304, .T. ) ;
#10092 = CARTESIAN_POINT ( 'NONE',  ( -0.7142790906314216981, 1.400791805248629895, 9.945241992664895392 ) ) ;
#10093 = CARTESIAN_POINT ( 'NONE',  ( -1.721971274562257515, -0.09408549481333014497, 9.928159647716187308 ) ) ;
#10094 = CARTESIAN_POINT ( 'NONE',  ( -206.6959734468149463, -1.750000000000010214, -39.18171244307202983 ) ) ;
#10095 = VERTEX_POINT ( 'NONE', #38896 ) ;
#10096 = ORIENTED_EDGE ( 'NONE', *, *, #7057, .F. ) ;
#10097 = DIRECTION ( 'NONE',  ( 0.000000000000000000, 1.000000000000000000, 0.000000000000000000 ) ) ;
#10098 = CARTESIAN_POINT ( 'NONE',  ( -164.9459734468149463, 2.143131898507880377E-16, 119.0682875569279702 ) ) ;
#10099 = ORIENTED_EDGE ( 'NONE', *, *, #37230, .T. ) ;
#10100 = ORIENTED_EDGE ( 'NONE', *, *, #3388, .F. ) ;
#10101 = CARTESIAN_POINT ( 'NONE',  ( 210.0000000000000568, 2.143131898507881856E-16, 79.06828755692797017 ) ) ;
#10102 = DIRECTION ( 'NONE',  ( -0.000000000000000000, -6.123233995736766036E-17, 1.000000000000000000 ) ) ;
#10103 = CARTESIAN_POINT ( 'NONE',  ( -166.6959734468149463, 1.750000000000009992, 160.8182875569279702 ) ) ;
#10104 = FACE_OUTER_BOUND ( 'NONE', #20894, .T. ) ;
#10105 = ORIENTED_EDGE ( 'NONE', *, *, #6531, .F. ) ;
#10106 = LINE ( 'NONE', #18553, #14497 ) ;
#10107 = AXIS2_PLACEMENT_3D ( 'NONE', #12220, #39440, #429 ) ;
#10108 = VERTEX_POINT ( 'NONE', #3721 ) ;
#10109 = VECTOR ( 'NONE', #15907, 1000.000000000000000 ) ;
#10110 = DIRECTION ( 'NONE',  ( -1.000000000000000000, 0.000000000000000000, 0.000000000000000000 ) ) ;
#10111 = CARTESIAN_POINT ( 'NONE',  ( 0.000000000000000000, 17.00000000000000000, 0.000000000000000000 ) ) ;
#10112 = AXIS2_PLACEMENT_3D ( 'NONE', #26304, #21425, #44766 ) ;
#10113 = ORIENTED_EDGE ( 'NONE', *, *, #37510, .F. ) ;
#10114 = VERTEX_POINT ( 'NONE', #50626 ) ;
#10115 = CARTESIAN_POINT ( 'NONE',  ( 111.5540265531850537, -1.025126265847081442, 162.5682875569279133 ) ) ;
#10116 = CARTESIAN_POINT ( 'NONE',  ( 192.2789002873380184, -1.750000000000009548, -0.2068387089191121020 ) ) ;
#10117 = ORIENTED_EDGE ( 'NONE', *, *, #28149, .F. ) ;
#10118 = FACE_OUTER_BOUND ( 'NONE', #44471, .T. ) ;
#10119 = ORIENTED_EDGE ( 'NONE', *, *, #31508, .T. ) ;
#10120 = CARTESIAN_POINT ( 'NONE',  ( -124.9459734468149321, 1.025126265847081886, 39.06828755692799149 ) ) ;
#10121 = EDGE_LOOP ( 'NONE', ( #426, #3650, #29424 ) ) ;
#10122 = DIRECTION ( 'NONE',  ( 0.000000000000000000, -1.544785076050074834E-48, -1.000000000000000000 ) ) ;
#10123 =( BOUNDED_CURVE ( )  B_SPLINE_CURVE ( 3, ( #41592, #10298, #25958, #33907 ),
 .UNSPECIFIED., .F., .F. ) 
 B_SPLINE_CURVE_WITH_KNOTS ( ( 4, 4 ),
 ( 3.141592653589793116, 4.712388980384689674 ),
 .UNSPECIFIED. ) 
 CURVE ( )  GEOMETRIC_REPRESENTATION_ITEM ( )  RATIONAL_B_SPLINE_CURVE ( ( 1.000000000000000000, 0.8047378541243649375, 0.8047378541243649375, 1.000000000000000000 ) ) 
 REPRESENTATION_ITEM ( '' )  );
#10124 = DIRECTION ( 'NONE',  ( -0.000000000000000000, -1.000000000000000000, -0.000000000000000000 ) ) ;
#10125 = PLANE ( 'NONE',  #3076 ) ;
#10126 = DIRECTION ( 'NONE',  ( -1.000000000000000000, -0.000000000000000000, -0.000000000000000000 ) ) ;
#10127 = VECTOR ( 'NONE', #28868, 1000.000000000000114 ) ;
#10128 = CARTESIAN_POINT ( 'NONE',  ( 73.30402655318508209, 1.750000000000009992, 0.8182875569279768335 ) ) ;
#10129 = ORIENTED_EDGE ( 'NONE', *, *, #48830, .T. ) ;
#10130 = DIRECTION ( 'NONE',  ( 0.000000000000000000, -1.000000000000000000, 0.000000000000000000 ) ) ;
#10131 =( BOUNDED_CURVE ( )  B_SPLINE_CURVE ( 3, ( #19900, #42241, #7100, #46811 ),
 .UNSPECIFIED., .F., .F. ) 
 B_SPLINE_CURVE_WITH_KNOTS ( ( 4, 4 ),
 ( 0.000000000000000000, 1.570796326794896558 ),
 .UNSPECIFIED. ) 
 CURVE ( )  GEOMETRIC_REPRESENTATION_ITEM ( )  RATIONAL_B_SPLINE_CURVE ( ( 1.000000000000000000, 0.8047378541243649375, 0.8047378541243649375, 1.000000000000000000 ) ) 
 REPRESENTATION_ITEM ( '' )  );
#10132 = CARTESIAN_POINT ( 'NONE',  ( 71.55402655318505367, -1.025126265847089435, -40.93171244307204404 ) ) ;
#10133 = DIRECTION ( 'NONE',  ( -0.000000000000000000, -0.000000000000000000, -1.000000000000000000 ) ) ;
#10134 = DIRECTION ( 'NONE',  ( 0.000000000000000000, 0.000000000000000000, 1.000000000000000000 ) ) ;
#10135 = EDGE_CURVE ( 'NONE', #16798, #5037, #23489, .T. ) ;
#10136 = LINE ( 'NONE', #45257, #35449 ) ;
#10137 = LINE ( 'NONE', #10640, #5658 ) ;
#10138 = AXIS2_PLACEMENT_3D ( 'NONE', #29397, #10153, #30415 ) ;
#10139 = FACE_OUTER_BOUND ( 'NONE', #16870, .T. ) ;
#10140 = ADVANCED_FACE ( 'NONE', ( #9097 ), #25494, .T. ) ;
#10141 = VECTOR ( 'NONE', #2173, 1000.000000000000000 ) ;
#10142 = DIRECTION ( 'NONE',  ( -1.000000000000000000, 0.000000000000000000, 0.000000000000000000 ) ) ;
#10143 =( BOUNDED_CURVE ( )  B_SPLINE_CURVE ( 3, ( #46331, #11226, #26865, #34842 ),
 .UNSPECIFIED., .F., .F. ) 
 B_SPLINE_CURVE_WITH_KNOTS ( ( 4, 4 ),
 ( 0.000000000000000000, 1.570796326794896558 ),
 .UNSPECIFIED. ) 
 CURVE ( )  GEOMETRIC_REPRESENTATION_ITEM ( )  RATIONAL_B_SPLINE_CURVE ( ( 1.000000000000000000, 0.8047378541243649375, 0.8047378541243649375, 1.000000000000000000 ) ) 
 REPRESENTATION_ITEM ( '' )  );
#10144 = LINE ( 'NONE', #33762, #25478 ) ;
#10145 = AXIS2_PLACEMENT_3D ( 'NONE', #47407, #12298, #20256 ) ;
#10146 = ADVANCED_FACE ( 'NONE', ( #44469 ), #21140, .T. ) ;
#10147 = VECTOR ( 'NONE', #38491, 1000.000000000000000 ) ;
#10148 = ORIENTED_EDGE ( 'NONE', *, *, #46335, .F. ) ;
#10149 = EDGE_CURVE ( 'NONE', #50401, #11765, #18491, .T. ) ;
#10150 = DIRECTION ( 'NONE',  ( 0.000000000000000000, 0.000000000000000000, -1.000000000000000000 ) ) ;
#10151 = LINE ( 'NONE', #33767, #9857 ) ;
#10152 = DIRECTION ( 'NONE',  ( -1.000000000000000000, -0.000000000000000000, -0.000000000000000000 ) ) ;
#10153 = DIRECTION ( 'NONE',  ( 0.000000000000000000, 0.000000000000000000, -1.000000000000000000 ) ) ;
#10154 = CARTESIAN_POINT ( 'NONE',  ( 349.9999999999999432, -166.9999999999999432, 343.9999999999997726 ) ) ;
#10155 = ORIENTED_EDGE ( 'NONE', *, *, #21122, .F. ) ;
#10156 = PRODUCT ( 'fan', 'fan', '', ( #39299 ) ) ;
#10157 = ORIENTED_EDGE ( 'NONE', *, *, #31822, .T. ) ;
#10158 = DIRECTION ( 'NONE',  ( 0.000000000000000000, 0.000000000000000000, -1.000000000000000000 ) ) ;
#10159 = CARTESIAN_POINT ( 'NONE',  ( 73.30402655318508209, 1.750000000000010214, 40.81828755692798438 ) ) ;
#10160 = VECTOR ( 'NONE', #46877, 1000.000000000000000 ) ;
#10161 = EDGE_LOOP ( 'NONE', ( #50373, #5305, #21441, #23555 ) ) ;
#10162 = CARTESIAN_POINT ( 'NONE',  ( 6.875132362119187768, -33.14667368551891258, 8.356839323120299312 ) ) ;
#10163 = DIRECTION ( 'NONE',  ( 3.172065745548403743E-16, 1.000000000000000000, 0.000000000000000000 ) ) ;
#10164 = ORIENTED_EDGE ( 'NONE', *, *, #19288, .T. ) ;
#10165 = ORIENTED_EDGE ( 'NONE', *, *, #1507, .F. ) ;
#10166 = EDGE_LOOP ( 'NONE', ( #4937, #42763, #45111, #44914, #25432 ) ) ;
#10167 = B_SPLINE_CURVE_WITH_KNOTS ( 'NONE', 3,
 ( #8642, #40447, #47838, #31750 ),
 .UNSPECIFIED., .F., .F.,
 ( 4, 4 ),
 ( 0.7998230999345287140, 0.9869080488566184250 ),
 .UNSPECIFIED. ) ;
#10168 = EDGE_CURVE ( 'NONE', #20400, #29240, #39842, .T. ) ;
#10169 = EDGE_CURVE ( 'NONE', #38591, #28471, #28844, .T. ) ;
#10170 = CARTESIAN_POINT ( 'NONE',  ( 164.9999999999999716, -168.9999999999999432, -350.0000000000001705 ) ) ;
#10171 = CARTESIAN_POINT ( 'NONE',  ( 0.3862712429686727678, 1.188820645368945605, 10.00000000000000000 ) ) ;
#10172 = CARTESIAN_POINT ( 'NONE',  ( 168.9999999999999716, -93.49999999999998579, -340.0000000000001137 ) ) ;
#10173 = ADVANCED_FACE ( 'NONE', ( #44966 ), #20889, .F. ) ;
#10174 = ORIENTED_EDGE ( 'NONE', *, *, #19751, .T. ) ;
#10175 = EDGE_CURVE ( 'NONE', #8966, #48305, #50542, .T. ) ;
#10176 = DIRECTION ( 'NONE',  ( -0.000000000000000000, -1.000000000000000000, -0.000000000000000000 ) ) ;
#10177 = CARTESIAN_POINT ( 'NONE',  ( -14.99999999999937472, 17.00000000000000000, -54.99999999999999289 ) ) ;
#10178 =( NAMED_UNIT ( * ) SI_UNIT ( $, .STERADIAN. ) SOLID_ANGLE_UNIT ( ) );
#10179 = ORIENTED_EDGE ( 'NONE', *, *, #3344, .F. ) ;
#10180 = EDGE_LOOP ( 'NONE', ( #15997, #36779, #31571 ) ) ;
#10181 = LINE ( 'NONE', #37156, #48316 ) ;
#10182 = EDGE_CURVE ( 'NONE', #39878, #1277, #1153, .T. ) ;
#10183 = AXIS2_PLACEMENT_3D ( 'NONE', #40077, #39576, #43161 ) ;
#10184 = LINE ( 'NONE', #37910, #48800 ) ;
#10185 = ADVANCED_FACE ( 'NONE', ( #4984, #28342 ), #9842, .T. ) ;
#10186 = CARTESIAN_POINT ( 'NONE',  ( 72.27890028733797578, -1.750000000000010214, 79.79316129108087807 ) ) ;
#10187 = VERTEX_POINT ( 'NONE', #36315 ) ;
#10188 = CARTESIAN_POINT ( 'NONE',  ( 155.0540265531850537, 2.143131898507880377E-16, 165.0000000000000000 ) ) ;
#10189 = LINE ( 'NONE', #49140, #18221 ) ;
#10190 = DIRECTION ( 'NONE',  ( -0.000000000000000000, -0.000000000000000000, -1.000000000000000000 ) ) ;
#10191 = CARTESIAN_POINT ( 'NONE',  ( 432.7825420346616170, -69.93075758371364259, -120.5992382549688671 ) ) ;
#10192 = DIRECTION ( 'NONE',  ( 1.000000000000000000, 0.000000000000000000, 0.000000000000000000 ) ) ;
#10193 = LINE ( 'NONE', #38668, #6987 ) ;
#10194 = DIRECTION ( 'NONE',  ( 0.000000000000000000, 0.000000000000000000, 1.000000000000000000 ) ) ;
#10195 = CARTESIAN_POINT ( 'NONE',  ( 50.24128791297869867, 41.04536285977714982, 5.000000000000000000 ) ) ;
#10196 = DIRECTION ( 'NONE',  ( 6.203854594147707562E-25, -2.067951531382569187E-25, 1.000000000000000000 ) ) ;
#10197 = EDGE_CURVE ( 'NONE', #25811, #16425, #23051, .T. ) ;
#10198 = EDGE_CURVE ( 'NONE', #7355, #9513, #38621, .T. ) ;
#10199 = CARTESIAN_POINT ( 'NONE',  ( 356.0000000000002842, -165.0000000000001137, -110.0000000000002132 ) ) ;
#10200 = VECTOR ( 'NONE', #18824, 1000.000000000000114 ) ;
#10201 = ADVANCED_FACE ( 'NONE', ( #32198 ), #10050, .T. ) ;
#10202 = EDGE_CURVE ( 'NONE', #38172, #17930, #11114, .T. ) ;
#10203 = CARTESIAN_POINT ( 'NONE',  ( -31.46770792452106846, 38.94077080897363885, 3.199614146704519602 ) ) ;
#10204 = AXIS2_PLACEMENT_3D ( 'NONE', #26408, #25410, #49211 ) ;
#10205 = ORIENTED_EDGE ( 'NONE', *, *, #44178, .T. ) ;
#10206 = DIRECTION ( 'NONE',  ( 1.000000000000000000, -0.000000000000000000, -0.000000000000000000 ) ) ;
#10207 = CARTESIAN_POINT ( 'NONE',  ( -14.52758583651993618, -8.922352469211071835, 8.953103998512858652 ) ) ;
#10208 = CARTESIAN_POINT ( 'NONE',  ( 155.0540265531850537, 1.025126265847089657, -120.9317124430720440 ) ) ;
#10209 = EDGE_LOOP ( 'NONE', ( #39783, #1652, #49691, #25955, #43220, #35433 ) ) ;
#10210 =( NAMED_UNIT ( * ) SI_UNIT ( $, .STERADIAN. ) SOLID_ANGLE_UNIT ( ) );
#10211 = CARTESIAN_POINT ( 'NONE',  ( 164.9999999999999716, -272.5000000000000000, -98.99999999999990052 ) ) ;
#10212 = CIRCLE ( 'NONE', #27432, 4.000000000000003553 ) ;
#10213 = ORIENTED_EDGE ( 'NONE', *, *, #47118, .F. ) ;
#10214 = PLANE ( 'NONE',  #45141 ) ;
#10215 = CARTESIAN_POINT ( 'NONE',  ( 349.9999999999999432, -180.9999999999999716, 339.9999999999997726 ) ) ;
#10217 = EDGE_CURVE ( 'NONE', #28864, #2021, #2399, .T. ) ;
#10216 = CARTESIAN_POINT ( 'NONE',  ( -124.9459734468149321, 1.025126265847081664, 2.568287556927973281 ) ) ;
#10218 = FACE_OUTER_BOUND ( 'NONE', #40098, .T. ) ;
#10219 = ORIENTED_EDGE ( 'NONE', *, *, #45226, .T. ) ;
#10220 = DIRECTION ( 'NONE',  ( -0.000000000000000000, 0.000000000000000000, 1.000000000000000000 ) ) ;
#10221 = ORIENTED_EDGE ( 'NONE', *, *, #16836, .T. ) ;
#10222 = VERTEX_POINT ( 'NONE', #37825 ) ;
#10223 = CIRCLE ( 'NONE', #38111, 2.000000000000001776 ) ;
#10224 = CYLINDRICAL_SURFACE ( 'NONE', #37752, 4.000000000000003553 ) ;
#10225 = EDGE_LOOP ( 'NONE', ( #39027, #17856, #46245, #17934, #591, #27097 ) ) ;
#10226 = CARTESIAN_POINT ( 'NONE',  ( -48.44597344681495343, 0.000000000000000000, -157.4317124430720014 ) ) ;
#10227 = DIRECTION ( 'NONE',  ( -1.000000000000000000, -0.000000000000000000, -0.000000000000000000 ) ) ;
#10228 = ADVANCED_FACE ( 'NONE', ( #42146 ), #33464, .F. ) ;
#10229 = DIRECTION ( 'NONE',  ( -1.000000000000000000, 0.000000000000000000, -0.000000000000000000 ) ) ;
#10230 = CARTESIAN_POINT ( 'NONE',  ( 80.00000000000028422, 17.00000000000000000, -60.00000000000000000 ) ) ;
#10231 = CARTESIAN_POINT ( 'NONE',  ( 135.0000000000012790, 17.00000000000000000, 5.000000000000004441 ) ) ;
#10232 = ORIENTED_EDGE ( 'NONE', *, *, #2632, .F. ) ;
#10233 = CARTESIAN_POINT ( 'NONE',  ( 10.50000000000000178, -46.51315789473684248, -6.315789473684215949 ) ) ;
#10234 = LINE ( 'NONE', #47989, #47863 ) ;
#10235 = DIRECTION ( 'NONE',  ( -0.000000000000000000, -0.000000000000000000, 1.000000000000000000 ) ) ;
#10236 = EDGE_CURVE ( 'NONE', #7661, #18090, #37575, .T. ) ;
#10237 = VECTOR ( 'NONE', #30736, 1000.000000000000000 ) ;
#10238 = VERTEX_POINT ( 'NONE', #22653 ) ;
#10239 = EDGE_CURVE ( 'NONE', #27847, #36062, #2244, .T. ) ;
#10240 = CARTESIAN_POINT ( 'NONE',  ( 1.305659100530805361, -0.2632760600745564505, 9.951893257060017817 ) ) ;
#10241 = DIRECTION ( 'NONE',  ( 0.000000000000000000, 0.9230769230769231282, 0.3846153846153844702 ) ) ;
#10242 = ORIENTED_EDGE ( 'NONE', *, *, #20, .F. ) ;
#10243 = CIRCLE ( 'NONE', #38938, 1.750000000000008438 ) ;
#10244 = ORIENTED_EDGE ( 'NONE', *, *, #19075, .F. ) ;
#10245 = ORIENTED_EDGE ( 'NONE', *, *, #49756, .F. ) ;
#10246 = CARTESIAN_POINT ( 'NONE',  ( -167.4999999999999716, -62.49999999999997158, -120.5992382549688671 ) ) ;
#10247 = EDGE_CURVE ( 'NONE', #1790, #10360, #45114, .T. ) ;
#10248 = ORIENTED_EDGE ( 'NONE', *, *, #33122, .F. ) ;
#10249 = EDGE_CURVE ( 'NONE', #10420, #47806, #24522, .T. ) ;
#10250 = CARTESIAN_POINT ( 'NONE',  ( 0.3862712429686894766, -1.188820645368940276, 10.00000000000000000 ) ) ;
#10251 = SURFACE_STYLE_USAGE ( .BOTH. , #45362 ) ;
#10252 = ADVANCED_FACE ( 'NONE', ( #14963 ), #26506, .F. ) ;
#10253 = FACE_BOUND ( 'NONE', #46200, .T. ) ;
#10254 = DIRECTION ( 'NONE',  ( -1.000000000000000000, -0.000000000000000000, -0.000000000000000000 ) ) ;
#10255 = ORIENTED_EDGE ( 'NONE', *, *, #45625, .F. ) ;
#10256 = VECTOR ( 'NONE', #3796, 1000.000000000000000 ) ;
#10257 = CARTESIAN_POINT ( 'NONE',  ( 350.0000000000000000, -168.9999999999999432, -340.0000000000001705 ) ) ;
#10258 = CYLINDRICAL_SURFACE ( 'NONE', #41492, 1.750000000000008438 ) ;
#10259 = ADVANCED_FACE ( 'NONE', ( #18040 ), #49300, .T. ) ;
#10260 = CARTESIAN_POINT ( 'NONE',  ( 153.3040265531850537, 1.750000000000009992, 160.8182875569279702 ) ) ;
#10261 = AXIS2_PLACEMENT_3D ( 'NONE', #34193, #45935, #19518 ) ;
#10262 = AXIS2_PLACEMENT_3D ( 'NONE', #18069, #19589, #7811 ) ;
#10263 = ORIENTED_EDGE ( 'NONE', *, *, #13985, .F. ) ;
#10264 = DIRECTION ( 'NONE',  ( 1.000000000000000000, 0.000000000000000000, 0.000000000000000000 ) ) ;
#10265 = CARTESIAN_POINT ( 'NONE',  ( -124.9459734468149463, 2.143131898507847836E-16, 119.0682875569279844 ) ) ;
#10266 = EDGE_CURVE ( 'NONE', #25811, #23429, #17605, .T. ) ;
#10267 = CARTESIAN_POINT ( 'NONE',  ( -33.16902712922616558, 37.70469005304312304, 1.847720168420772691 ) ) ;
#10268 = CARTESIAN_POINT ( 'NONE',  ( -125.6708471809678542, 1.749999999999996891, -118.1565861772249661 ) ) ;
#10269 = ORIENTED_EDGE ( 'NONE', *, *, #50260, .T. ) ;
#10270 = CARTESIAN_POINT ( 'NONE',  ( 195.0540265531851105, -1.025126265847089213, 42.56828755692799149 ) ) ;
#10271 = CARTESIAN_POINT ( 'NONE',  ( 341.2957005644334458, 2.688010569040066411, 225.2259797391361644 ) ) ;
#10272 = CARTESIAN_POINT ( 'NONE',  ( -14.49999999999999822, -46.01315789473684248, 5.916985404131814619 ) ) ;
#10273 = CARTESIAN_POINT ( 'NONE',  ( 194.9999999999999432, 164.9999999999999716, 112.0000000000000000 ) ) ;
#10274 = EDGE_LOOP ( 'NONE', ( #45472, #29853, #38354, #1958 ) ) ;
#10275 = LINE ( 'NONE', #48717, #16601 ) ;
#10276 = ORIENTED_EDGE ( 'NONE', *, *, #43094, .T. ) ;
#10277 = CARTESIAN_POINT ( 'NONE',  ( -194.9999999999999432, 0.000000000000000000, 0.000000000000000000 ) ) ;
#10278 = VECTOR ( 'NONE', #30203, 1000.000000000000000 ) ;
#10279 = EDGE_LOOP ( 'NONE', ( #4296, #37742, #15771, #5995, #30125, #42949 ) ) ;
#10280 = LINE ( 'NONE', #25684, #35306 ) ;
#10281 = DIRECTION ( 'NONE',  ( 0.000000000000000000, 0.000000000000000000, -1.000000000000000000 ) ) ;
#10282 = AXIS2_PLACEMENT_3D ( 'NONE', #14672, #47454, #31355 ) ;
#10283 = CARTESIAN_POINT ( 'NONE',  ( 154.1026953830863420, -98.56198943095992604, 22.84256005001721945 ) ) ;
#10284 = ORIENTED_EDGE ( 'NONE', *, *, #21486, .F. ) ;
#10285 =( BOUNDED_CURVE ( )  B_SPLINE_CURVE ( 3, ( #15940, #19511, #4138, #35200 ),
 .UNSPECIFIED., .F., .F. ) 
 B_SPLINE_CURVE_WITH_KNOTS ( ( 4, 4 ),
 ( 0.000000000000000000, 1.570796326794896558 ),
 .UNSPECIFIED. ) 
 CURVE ( )  GEOMETRIC_REPRESENTATION_ITEM ( )  RATIONAL_B_SPLINE_CURVE ( ( 1.000000000000000000, 0.8047378541243649375, 0.8047378541243649375, 1.000000000000000000 ) ) 
 REPRESENTATION_ITEM ( '' )  );
#10286 = MECHANICAL_DESIGN_GEOMETRIC_PRESENTATION_REPRESENTATION (  '', ( #9438 ), #44644 ) ;
#10287 = DIRECTION ( 'NONE',  ( -0.000000000000000000, -0.000000000000000000, -1.000000000000000000 ) ) ;
#10288 = ORIENTED_EDGE ( 'NONE', *, *, #14234, .F. ) ;
#10289 = CARTESIAN_POINT ( 'NONE',  ( 356.0000000000002274, 183.0000000000000284, -358.0000000000001705 ) ) ;
#10290 = CARTESIAN_POINT ( 'NONE',  ( 344.0000000000000568, 165.0000000000000000, 339.9999999999998295 ) ) ;
#10291 = VECTOR ( 'NONE', #34293, 1000.000000000000000 ) ;
#10292 = CARTESIAN_POINT ( 'NONE',  ( -165.6708471809677974, 1.750000000000010214, -78.15658617722490931 ) ) ;
#10293 = CARTESIAN_POINT ( 'NONE',  ( -9.999999999999998224, -41.51315789473684248, -25.00000000000000000 ) ) ;
#10294 = LINE ( 'NONE', #26440, #46984 ) ;
#10295 =( BOUNDED_CURVE ( )  B_SPLINE_CURVE ( 3, ( #7364, #27635, #3489, #42741 ),
 .UNSPECIFIED., .F., .F. ) 
 B_SPLINE_CURVE_WITH_KNOTS ( ( 4, 4 ),
 ( 1.570796326794896558, 3.141592653589793116 ),
 .UNSPECIFIED. ) 
 CURVE ( )  GEOMETRIC_REPRESENTATION_ITEM ( )  RATIONAL_B_SPLINE_CURVE ( ( 1.000000000000000000, 0.8047378541243649375, 0.8047378541243649375, 1.000000000000000000 ) ) 
 REPRESENTATION_ITEM ( '' )  );
#10296 = EDGE_LOOP ( 'NONE', ( #20382, #26510, #27115, #33635 ) ) ;
#10297 = ORIENTED_EDGE ( 'NONE', *, *, #15258, .F. ) ;
#10298 = CARTESIAN_POINT ( 'NONE',  ( 35.05402655318504657, -1.025126265847089435, 122.5682875569280128 ) ) ;
#10299 = VECTOR ( 'NONE', #40692, 1000.000000000000000 ) ;
#10300 = EDGE_CURVE ( 'NONE', #21591, #49766, #29855, .T. ) ;
#10301 = ORIENTED_EDGE ( 'NONE', *, *, #2670, .T. ) ;
#10302 = EDGE_CURVE ( 'NONE', #15862, #11298, #2881, .T. ) ;
#10303 = CARTESIAN_POINT ( 'NONE',  ( 191.5540265531851105, 0.000000000000000000, -157.4317124430720582 ) ) ;
#10304 = LINE ( 'NONE', #25964, #12511 ) ;
#10305 = ORIENTED_EDGE ( 'NONE', *, *, #18008, .F. ) ;
#10306 = DIRECTION ( 'NONE',  ( 0.000000000000000000, 0.000000000000000000, -1.000000000000000000 ) ) ;
#10307 = EDGE_CURVE ( 'NONE', #37848, #49781, #10362, .T. ) ;
#10308 = CARTESIAN_POINT ( 'NONE',  ( 7.500000000000000000, 224.9999999999999716, -240.0000000000000000 ) ) ;
#10309 = EDGE_LOOP ( 'NONE', ( #41983, #38654, #5294, #13936 ) ) ;
#10310 = DIRECTION ( 'NONE',  ( 0.000000000000000000, -2.265761274745217480E-16, 1.000000000000000000 ) ) ;
#10311 = CARTESIAN_POINT ( 'NONE',  ( 181.0000000000000284, -182.9999999999999716, -115.0000000000001279 ) ) ;
#10312 = EDGE_CURVE ( 'NONE', #10463, #29819, #16977, .T. ) ;
#10313 = DIRECTION ( 'NONE',  ( -1.000000000000000000, 0.000000000000000000, -0.000000000000000000 ) ) ;
#10314 = CARTESIAN_POINT ( 'NONE',  ( 343.9999999999999432, 185.0000000000002558, -360.0000000000003411 ) ) ;
#10315 = ADVANCED_FACE ( 'NONE', ( #45210 ), #18282, .F. ) ;
#10316 = CARTESIAN_POINT ( 'NONE',  ( 0.000000000000000000, 6.912230148066162094, 5.000000000000000000 ) ) ;
#10317 = AXIS2_PLACEMENT_3D ( 'NONE', #35935, #43348, #16172 ) ;
#10318 = VERTEX_POINT ( 'NONE', #41653 ) ;
#10319 = ORIENTED_EDGE ( 'NONE', *, *, #31508, .F. ) ;
#10320 = DIRECTION ( 'NONE',  ( 1.000000000000000000, 0.000000000000000000, -0.000000000000000000 ) ) ;
#10321 = VECTOR ( 'NONE', #13755, 1000.000000000000000 ) ;
#10322 = EDGE_CURVE ( 'NONE', #30968, #15451, #14703, .T. ) ;
#10323 = DIRECTION ( 'NONE',  ( -1.000000000000000000, -6.938893903907233308E-16, -0.000000000000000000 ) ) ;
#10324 = CARTESIAN_POINT ( 'NONE',  ( 350.0000000000000000, 169.0000000000000000, -356.0000000000002274 ) ) ;
#10325 = EDGE_CURVE ( 'NONE', #38882, #7516, #46794, .T. ) ;
#10326 = PLANE ( 'NONE',  #35446 ) ;
#10327 = ORIENTED_EDGE ( 'NONE', *, *, #8416, .T. ) ;
#10328 = CARTESIAN_POINT ( 'NONE',  ( 350.0000000000001137, 181.0000000000000284, 341.9999999999997726 ) ) ;
#10329 = EDGE_LOOP ( 'NONE', ( #37635, #17282, #14035, #18306, #43259, #13127 ) ) ;
#10330 = CARTESIAN_POINT ( 'NONE',  ( 210.0000000000000568, 0.000000000000000000, 162.5682875569279702 ) ) ;
#10331 = MECHANICAL_DESIGN_GEOMETRIC_PRESENTATION_REPRESENTATION (  '', ( #29995 ), #2125 ) ;
#10332 = FACE_OUTER_BOUND ( 'NONE', #24987, .T. ) ;
#10333 = DIRECTION ( 'NONE',  ( 0.000000000000000000, 0.000000000000000000, 1.000000000000000000 ) ) ;
#10334 = CARTESIAN_POINT ( 'NONE',  ( -208.1473046169136580, 159.2880105690400399, 472.8425600500171981 ) ) ;
#10335 = CARTESIAN_POINT ( 'NONE',  ( 75.05402655318509630, 2.143131898507880377E-16, 165.0000000000000000 ) ) ;
#10336 = VECTOR ( 'NONE', #47689, 1000.000000000000000 ) ;
#10337 = CARTESIAN_POINT ( 'NONE',  ( 1.249999999999999778, -0.000000000000000000, -10.00000000000000000 ) ) ;
#10338 = ORIENTED_EDGE ( 'NONE', *, *, #24370, .F. ) ;
#10339 = CARTESIAN_POINT ( 'NONE',  ( 7.499999999999944045, -224.9999999999999716, -240.0000000000000000 ) ) ;
#10340 = CARTESIAN_POINT ( 'NONE',  ( 72.27890028733797578, 1.750000000000009326, -158.1565861772249377 ) ) ;
#10341 = PLANE ( 'NONE',  #31545 ) ;
#10342 = B_SPLINE_CURVE_WITH_KNOTS ( 'NONE', 3,
 ( #34356, #41781, #31017, #49694 ),
 .UNSPECIFIED., .F., .F.,
 ( 4, 4 ),
 ( 0.000000000000000000, 0.0001252128669263171713 ),
 .UNSPECIFIED. ) ;
#10343 = VECTOR ( 'NONE', #20955, 1000.000000000000000 ) ;
#10344 = DIRECTION ( 'NONE',  ( -1.587271980518778491E-16, 5.169878828456422968E-26, 1.000000000000000000 ) ) ;
#10345 = ORIENTED_EDGE ( 'NONE', *, *, #2980, .T. ) ;
#10346 = FACE_OUTER_BOUND ( 'NONE', #38478, .T. ) ;
#10347 = ORIENTED_EDGE ( 'NONE', *, *, #46797, .F. ) ;
#10348 = CARTESIAN_POINT ( 'NONE',  ( 193.3040265531851105, 0.000000000000000000, 165.0000000000000000 ) ) ;
#10349 = CARTESIAN_POINT ( 'NONE',  ( -168.4459734468149463, 0.000000000000000000, 165.0000000000000000 ) ) ;
#10350 = CYLINDRICAL_SURFACE ( 'NONE', #37042, 1.750000000000008438 ) ;
#10351 = VERTEX_POINT ( 'NONE', #28030 ) ;
#10352 = EDGE_CURVE ( 'NONE', #29314, #5869, #12134, .T. ) ;
#10353 = AXIS2_PLACEMENT_3D ( 'NONE', #30370, #14459, #35245 ) ;
#10354 = CARTESIAN_POINT ( 'NONE',  ( 0.1287570809895575430, 0.3962735484563150168, -10.00000000000000000 ) ) ;
#10355 = ORIENTED_EDGE ( 'NONE', *, *, #12681, .T. ) ;
#10356 = DIRECTION ( 'NONE',  ( -1.000000000000000000, -0.000000000000000000, -0.000000000000000000 ) ) ;
#10357 = AXIS2_PLACEMENT_3D ( 'NONE', #10933, #42987, #30965 ) ;
#10358 = DIRECTION ( 'NONE',  ( -1.000000000000000000, -0.000000000000000000, -0.000000000000000000 ) ) ;
#10359 = CARTESIAN_POINT ( 'NONE',  ( -4.945973446814917018, -1.025126265847096763, 2.568287556927999926 ) ) ;
#10360 = VERTEX_POINT ( 'NONE', #47239 ) ;
#10361 = ORIENTED_EDGE ( 'NONE', *, *, #4911, .T. ) ;
#10362 = LINE ( 'NONE', #34473, #21842 ) ;
#10363 = CARTESIAN_POINT ( 'NONE',  ( -119.9999999999984652, 17.00000000000000000, 35.00000000000000000 ) ) ;
#10364 = VECTOR ( 'NONE', #22973, 1000.000000000000000 ) ;
#10365 = ORIENTED_EDGE ( 'NONE', *, *, #18666, .T. ) ;
#10366 = ORIENTED_EDGE ( 'NONE', *, *, #39308, .F. ) ;
#10367 = CARTESIAN_POINT ( 'NONE',  ( 33.30402655318503946, -1.750000000000010658, -79.18171244307201562 ) ) ;
#10368 = CARTESIAN_POINT ( 'NONE',  ( -84.94597344681494633, 2.143131898507880377E-16, -37.43171244307205825 ) ) ;
#10369 = VECTOR ( 'NONE', #9739, 1000.000000000000000 ) ;
#10370 = ORIENTED_EDGE ( 'NONE', *, *, #22698, .F. ) ;
#10371 = CARTESIAN_POINT ( 'NONE',  ( 115.0540265531850395, 2.143131898507847836E-16, -157.4317124430720582 ) ) ;
#10372 = VERTEX_POINT ( 'NONE', #43175 ) ;
#10373 = VECTOR ( 'NONE', #41904, 1000.000000000000000 ) ;
#10374 = DIRECTION ( 'NONE',  ( 0.000000000000000000, 0.000000000000000000, 1.000000000000000000 ) ) ;
#10375 = FACE_OUTER_BOUND ( 'NONE', #48052, .T. ) ;
#10376 = ORIENTED_EDGE ( 'NONE', *, *, #17666, .F. ) ;
#10377 = ORIENTED_EDGE ( 'NONE', *, *, #33550, .T. ) ;
#10378 = EDGE_CURVE ( 'NONE', #23064, #10490, #47490, .T. ) ;
#10379 = DIRECTION ( 'NONE',  ( 0.000000000000000000, -0.000000000000000000, -1.000000000000000000 ) ) ;
#10380 = CARTESIAN_POINT ( 'NONE',  ( 210.0000000000000568, 2.143131898507881116E-16, 39.06828755692797728 ) ) ;
#10381 = ORIENTED_EDGE ( 'NONE', *, *, #50390, .F. ) ;
#10382 = LINE ( 'NONE', #41673, #26403 ) ;
#10383 = VERTEX_POINT ( 'NONE', #23672 ) ;
#10384 = DIRECTION ( 'NONE',  ( -0.000000000000000000, -0.000000000000000000, -1.000000000000000000 ) ) ;
#10385 = CYLINDRICAL_SURFACE ( 'NONE', #17434, 1.750000000000015543 ) ;
#10386 = ORIENTED_EDGE ( 'NONE', *, *, #23322, .F. ) ;
#10387 = DIRECTION ( 'NONE',  ( 0.000000000000000000, 0.000000000000000000, 1.000000000000000000 ) ) ;
#10388 = LINE ( 'NONE', #29626, #40800 ) ;
#10389 = CARTESIAN_POINT ( 'NONE',  ( -64.99999999999971578, 17.00000000000000000, -84.99999999999998579 ) ) ;
#10390 = LINE ( 'NONE', #49582, #39376 ) ;
#10391 = VECTOR ( 'NONE', #1234, 1000.000000000000000 ) ;
#10392 = FACE_OUTER_BOUND ( 'NONE', #27905, .T. ) ;
#10393 = ORIENTED_EDGE ( 'NONE', *, *, #27794, .T. ) ;
#10394 = CARTESIAN_POINT ( 'NONE',  ( 151.5540265531850537, 0.000000000000000000, 119.0682875569279702 ) ) ;
#10395 = DIRECTION ( 'NONE',  ( -1.000000000000000000, 0.000000000000000000, 0.000000000000000000 ) ) ;
#10396 = CYLINDRICAL_SURFACE ( 'NONE', #5607, 1.750000000000008438 ) ;
#10397 = CARTESIAN_POINT ( 'NONE',  ( -48.34672127938071640, 13.00749071703899773, 3.199614146704519602 ) ) ;
#10398 = DIRECTION ( 'NONE',  ( -0.6805276818820364948, -0.4944323023722119737, 0.5407575913134972101 ) ) ;
#10399 = DIRECTION ( 'NONE',  ( -0.000000000000000000, -0.000000000000000000, -1.000000000000000000 ) ) ;
#10400 = CARTESIAN_POINT ( 'NONE',  ( 1.249999999999999778, 0.000000000000000000, 10.00000000000000000 ) ) ;
#10401 = CARTESIAN_POINT ( 'NONE',  ( 350.0000000000000000, -164.9999999999999432, -360.0000000000002274 ) ) ;
#10402 = CARTESIAN_POINT ( 'NONE',  ( -114.9999999999994031, 16.00000000000000000, -30.00000000000000000 ) ) ;
#10403 = ADVANCED_FACE ( 'NONE', ( #15461 ), #39342, .F. ) ;
#10404 = ORIENTED_EDGE ( 'NONE', *, *, #36343, .F. ) ;
#10405 = CARTESIAN_POINT ( 'NONE',  ( 33.14391172085758086, 37.72293746533119219, -8.016098858316205167 ) ) ;
#10406 = CARTESIAN_POINT ( 'NONE',  ( -14.86945752723352498, -7.944783388878907004, 2.590526750877053086 ) ) ;
#10407 = CARTESIAN_POINT ( 'NONE',  ( 1.011271242968688311, -0.7347315653655855927, 10.00000000000000000 ) ) ;
#10408 = CARTESIAN_POINT ( 'NONE',  ( -125.6708471809678542, -1.749999999999996669, 41.84341382277508359 ) ) ;
#10409 = CARTESIAN_POINT ( 'NONE',  ( 0.4402948852767718524, -2.015117899693914527, 9.894754715216725671 ) ) ;
#10410 = ORIENTED_EDGE ( 'NONE', *, *, #47146, .F. ) ;
#10411 = ORIENTED_EDGE ( 'NONE', *, *, #26811, .F. ) ;
#10412 = DIRECTION ( 'NONE',  ( 1.000000000000000000, 0.000000000000000000, 0.000000000000000000 ) ) ;
#10413 = CARTESIAN_POINT ( 'NONE',  ( 185.0000000000000000, -184.9999999999999716, -356.0000000000014211 ) ) ;
#10414 = AXIS2_PLACEMENT_3D ( 'NONE', #13645, #13387, #25197 ) ;
#10415 = ORIENTED_EDGE ( 'NONE', *, *, #30569, .F. ) ;
#10416 = CARTESIAN_POINT ( 'NONE',  ( -1.250000000000000222, 0.000000000000000000, 10.00000000000000000 ) ) ;
#10417 = LINE ( 'NONE', #21705, #48623 ) ;
#10418 = ORIENTED_EDGE ( 'NONE', *, *, #21596, .T. ) ;
#10419 = ORIENTED_EDGE ( 'NONE', *, *, #41882, .T. ) ;
#10420 = VERTEX_POINT ( 'NONE', #35240 ) ;
#10421 = CARTESIAN_POINT ( 'NONE',  ( -204.9459734468149463, 2.143131898507880377E-16, -37.43171244307205825 ) ) ;
#10422 = CARTESIAN_POINT ( 'NONE',  ( -1.769963848780949478, 9.842115015280430868, 0.000000000000000000 ) ) ;
#10423 = CARTESIAN_POINT ( 'NONE',  ( 28.52604530808654815, 41.07801380285680892, -3.760136334089591248 ) ) ;
#10424 =( BOUNDED_CURVE ( )  B_SPLINE_CURVE ( 3, ( #1199, #35354, #47334, #16838 ),
 .UNSPECIFIED., .F., .F. ) 
 B_SPLINE_CURVE_WITH_KNOTS ( ( 4, 4 ),
 ( 4.712388980384689674, 6.283185307179586232 ),
 .UNSPECIFIED. ) 
 CURVE ( )  GEOMETRIC_REPRESENTATION_ITEM ( )  RATIONAL_B_SPLINE_CURVE ( ( 1.000000000000000000, 0.8047378541243649375, 0.8047378541243649375, 1.000000000000000000 ) ) 
 REPRESENTATION_ITEM ( '' )  );
#10425 = ORIENTED_EDGE ( 'NONE', *, *, #2005, .T. ) ;
#10426 = CYLINDRICAL_SURFACE ( 'NONE', #38281, 2.000000000000001776 ) ;
#10427 = CARTESIAN_POINT ( 'NONE',  ( 166.9999999999999716, -272.5000000000000000, -99.00000000000014211 ) ) ;
#10428 = CARTESIAN_POINT ( 'NONE',  ( 355.9999999999999432, -185.0000000000002558, -360.0000000000003411 ) ) ;
#10429 = VERTEX_POINT ( 'NONE', #7787 ) ;
#10430 = ORIENTED_EDGE ( 'NONE', *, *, #35603, .T. ) ;
#10431 = EDGE_CURVE ( 'NONE', #18861, #7763, #7074, .T. ) ;
#10433 = CARTESIAN_POINT ( 'NONE',  ( -4.945973446814903696, 2.143131898507912917E-16, -40.93171244307205825 ) ) ;
#10432 =( BOUNDED_CURVE ( )  B_SPLINE_CURVE ( 3, ( #48959, #29519, #45135, #10021 ),
 .UNSPECIFIED., .F., .F. ) 
 B_SPLINE_CURVE_WITH_KNOTS ( ( 4, 4 ),
 ( 1.570796326794883235, 3.141592653589794004 ),
 .UNSPECIFIED. ) 
 CURVE ( )  GEOMETRIC_REPRESENTATION_ITEM ( )  RATIONAL_B_SPLINE_CURVE ( ( 1.000000000000000000, 0.8047378541243617178, 0.8047378541243617178, 1.000000000000000000 ) ) 
 REPRESENTATION_ITEM ( '' )  );
#10434 = CARTESIAN_POINT ( 'NONE',  ( 151.5540265531850537, 0.000000000000000000, 119.0682875569279702 ) ) ;
#10435 = ORIENTED_EDGE ( 'NONE', *, *, #19414, .F. ) ;
#10436 = CARTESIAN_POINT ( 'NONE',  ( 31.55402655318503236, 0.000000000000000000, 165.0000000000000000 ) ) ;
#10437 = FACE_BOUND ( 'NONE', #1213, .T. ) ;
#10438 = DIRECTION ( 'NONE',  ( -0.000000000000000000, -1.000000000000000000, -0.000000000000000000 ) ) ;
#10439 = CARTESIAN_POINT ( 'NONE',  ( 166.9999999999999716, 165.0000000000000000, -344.0000000000001137 ) ) ;
#10440 = DIRECTION ( 'NONE',  ( 0.000000000000000000, 0.000000000000000000, 1.000000000000000000 ) ) ;
#10441 = ORIENTED_EDGE ( 'NONE', *, *, #38193, .F. ) ;
#10442 = EDGE_CURVE ( 'NONE', #25305, #4914, #15672, .T. ) ;
#10443 = PLANE ( 'NONE',  #44700 ) ;
#10444 = CARTESIAN_POINT ( 'NONE',  ( -47.72109971266203132, 1.750000000000009548, -118.1565861772249519 ) ) ;
#10445 = ADVANCED_FACE ( 'NONE', ( #42651 ), #50567, .T. ) ;
#10446 =( BOUNDED_CURVE ( )  B_SPLINE_CURVE ( 3, ( #48368, #20448, #972, #39978 ),
 .UNSPECIFIED., .F., .F. ) 
 B_SPLINE_CURVE_WITH_KNOTS ( ( 4, 4 ),
 ( 1.570796326794896558, 3.141592653589793116 ),
 .UNSPECIFIED. ) 
 CURVE ( )  GEOMETRIC_REPRESENTATION_ITEM ( )  RATIONAL_B_SPLINE_CURVE ( ( 1.000000000000000000, 0.8047378541243649375, 0.8047378541243649375, 1.000000000000000000 ) ) 
 REPRESENTATION_ITEM ( '' )  );
#10447 = CARTESIAN_POINT ( 'NONE',  ( 232.4999999999999716, -169.9999999999999716, 4.999999999999616307 ) ) ;
#10448 = EDGE_CURVE ( 'NONE', #25186, #17816, #38585, .T. ) ;
#10449 = LINE ( 'NONE', #48891, #24716 ) ;
#10450 = AXIS2_PLACEMENT_3D ( 'NONE', #26601, #7612, #35340 ) ;
#10451 = CARTESIAN_POINT ( 'NONE',  ( -14.99999999999845812, 16.00000000000000000, 35.00000000000000000 ) ) ;
#10452 = EDGE_LOOP ( 'NONE', ( #23340, #5444, #17413, #39603 ) ) ;
#10453 = CARTESIAN_POINT ( 'NONE',  ( 350.0000000000001137, 183.0000000000000284, 355.9999999999997726 ) ) ;
#10454 = CYLINDRICAL_SURFACE ( 'NONE', #436, 1.750000000000001554 ) ;
#10455 = ADVANCED_FACE ( 'NONE', ( #31126 ), #341, .F. ) ;
#10456 = EDGE_CURVE ( 'NONE', #28373, #19760, #19051, .T. ) ;
#10457 = DIRECTION ( 'NONE',  ( -1.000000000000000000, -0.000000000000000000, -0.000000000000000000 ) ) ;
#10459 = ORIENTED_EDGE ( 'NONE', *, *, #1792, .T. ) ;
#10458 = EDGE_CURVE ( 'NONE', #4352, #23493, #15979, .T. ) ;
#10460 = CYLINDRICAL_SURFACE ( 'NONE', #37135, 4.000000000000003553 ) ;
#10461 = EDGE_CURVE ( 'NONE', #42393, #47565, #43414, .T. ) ;
#10462 = LINE ( 'NONE', #13544, #39327 ) ;
#10463 = VERTEX_POINT ( 'NONE', #84 ) ;
#10464 = CARTESIAN_POINT ( 'NONE',  ( 113.3040265531850537, 1.749999999999996891, 160.8182875569279702 ) ) ;
#10465 = CARTESIAN_POINT ( 'NONE',  ( 350.0000000000000000, 175.0000000000000568, -350.0000000000001705 ) ) ;
#10466 = CARTESIAN_POINT ( 'NONE',  ( 340.0000000000000568, 169.0000000000000000, 343.9999999999997726 ) ) ;
#10467 = CARTESIAN_POINT ( 'NONE',  ( -44.94597344681493922, 2.143131898507880377E-16, -40.93171244307205825 ) ) ;
#10468 = ADVANCED_FACE ( 'NONE', ( #27277 ), #23158, .F. ) ;
#10469 = ORIENTED_EDGE ( 'NONE', *, *, #23811, .F. ) ;
#10470 = LINE ( 'NONE', #22772, #26559 ) ;
#10471 = ORIENTED_EDGE ( 'NONE', *, *, #9611, .T. ) ;
#10472 = ORIENTED_EDGE ( 'NONE', *, *, #9611, .F. ) ;
#10473 = CARTESIAN_POINT ( 'NONE',  ( 85.00000000000152056, 16.00000000000000000, 60.00000000000000000 ) ) ;
#10474 = ORIENTED_EDGE ( 'NONE', *, *, #35944, .F. ) ;
#10475 = FACE_OUTER_BOUND ( 'NONE', #45479, .T. ) ;
#10476 = CARTESIAN_POINT ( 'NONE',  ( 0.3862712429686978033, -1.188820645368937834, 10.00000000000000000 ) ) ;
#10477 = LINE ( 'NONE', #31450, #226 ) ;
#10478 = CARTESIAN_POINT ( 'NONE',  ( 31.55402655318503236, 0.000000000000000000, 2.568287556927978166 ) ) ;
#10479 = EDGE_CURVE ( 'NONE', #41719, #25164, #2171, .T. ) ;
#10480 = ORIENTED_EDGE ( 'NONE', *, *, #2418, .F. ) ;
#10481 = CARTESIAN_POINT ( 'NONE',  ( 25.04522487443081502, -22.77512090857307925, 8.356839323120299312 ) ) ;
#10482 = FACE_OUTER_BOUND ( 'NONE', #8908, .T. ) ;
#10483 = DIRECTION ( 'NONE',  ( 0.000000000000000000, 0.000000000000000000, 1.000000000000000000 ) ) ;
#10484 = ADVANCED_FACE ( 'NONE', ( #11879 ), #27538, .T. ) ;
#10485 = EDGE_LOOP ( 'NONE', ( #27195, #11760, #38471, #31246 ) ) ;
#10486 = EDGE_CURVE ( 'NONE', #30177, #6629, #24696, .T. ) ;
#10487 = CARTESIAN_POINT ( 'NONE',  ( -1.057156451998854996, 0.7920882637787067804, 9.943883492372851407 ) ) ;
#10488 = CARTESIAN_POINT ( 'NONE',  ( 177.5000000000000284, 112.5000000000000000, 0.000000000000000000 ) ) ;
#10489 = EDGE_LOOP ( 'NONE', ( #37756, #30420, #2589, #21081 ) ) ;
#10490 = VERTEX_POINT ( 'NONE', #16988 ) ;
#10491 = EDGE_LOOP ( 'NONE', ( #7476, #37100, #24736, #22797, #46403 ) ) ;
#10492 = DIRECTION ( 'NONE',  ( 1.000000000000000000, 0.000000000000000000, 0.000000000000000000 ) ) ;
#10493 = EDGE_CURVE ( 'NONE', #21514, #24866, #8980, .T. ) ;
#10494 = LINE ( 'NONE', #25906, #17645 ) ;
#10495 = ORIENTED_EDGE ( 'NONE', *, *, #25612, .T. ) ;
#10496 = ADVANCED_FACE ( 'NONE', ( #20579 ), #16729, .F. ) ;
#10497 = CARTESIAN_POINT ( 'NONE',  ( -119.9999999999978400, 17.00000000000000000, 115.0000000000000142 ) ) ;
#10498 = CARTESIAN_POINT ( 'NONE',  ( 112.2789002873379758, 1.749999999999997113, 79.79316129108087807 ) ) ;
#10499 = FACE_BOUND ( 'NONE', #41012, .T. ) ;
#10500 = CARTESIAN_POINT ( 'NONE',  ( 114.3291528190321173, 1.749999999999996891, 119.7931612910809065 ) ) ;
#10501 = ORIENTED_EDGE ( 'NONE', *, *, #1979, .T. ) ;
#10502 = FACE_OUTER_BOUND ( 'NONE', #3532, .T. ) ;
#10503 = DIRECTION ( 'NONE',  ( -0.000000000000000000, -1.000000000000000000, -0.000000000000000000 ) ) ;
#10504 = ORIENTED_EDGE ( 'NONE', *, *, #6745, .F. ) ;
#10505 = CARTESIAN_POINT ( 'NONE',  ( 10.28825587112223161, -13.03847615613158517, 3.266473740018926541 ) ) ;
#10506 = EDGE_CURVE ( 'NONE', #11997, #22181, #27823, .T. ) ;
#10507 = DIRECTION ( 'NONE',  ( 1.000000000000000000, 0.000000000000000000, 0.000000000000000000 ) ) ;
#10508 = EDGE_LOOP ( 'NONE', ( #8425, #18349, #48223, #39121 ) ) ;
#10509 = FACE_OUTER_BOUND ( 'NONE', #4176, .T. ) ;
#10510 = CARTESIAN_POINT ( 'NONE',  ( -204.9459734468148895, 1.025126265847089879, 82.56828755692798438 ) ) ;
#10511 = CARTESIAN_POINT ( 'NONE',  ( 1.543575086786857176, -5.756316005467325247, -1.301042606982605321E-15 ) ) ;
#10512 = CARTESIAN_POINT ( 'NONE',  ( -5.000000000000000000, -184.7999999999999545, 340.1999999999997044 ) ) ;
#10514 = VERTEX_POINT ( 'NONE', #12619 ) ;
#10513 = EDGE_CURVE ( 'NONE', #42224, #14015, #47986, .T. ) ;
#10515 = CARTESIAN_POINT ( 'NONE',  ( -4.945973446814903696, 2.143131898507912917E-16, 119.0682875569279418 ) ) ;
#10516 = EDGE_CURVE ( 'NONE', #30605, #8966, #32895, .T. ) ;
#10518 = ORIENTED_EDGE ( 'NONE', *, *, #21829, .F. ) ;
#10517 = VECTOR ( 'NONE', #45190, 1000.000000000000000 ) ;
#10519 = CARTESIAN_POINT ( 'NONE',  ( 0.000000000000000000, 0.000000000000000000, 0.000000000000000000 ) ) ;
#10520 = ORIENTED_EDGE ( 'NONE', *, *, #44350, .T. ) ;
#10521 = EDGE_CURVE ( 'NONE', #48821, #17870, #33162, .T. ) ;
#10522 = CARTESIAN_POINT ( 'NONE',  ( 130.0000000000005684, 16.00000000000000000, -30.00000000000000000 ) ) ;
#10523 = CARTESIAN_POINT ( 'NONE',  ( 35.05402655318504657, 2.143131898507880377E-16, -80.93171244307204404 ) ) ;
#10524 = ADVANCED_FACE ( 'NONE', ( #48742 ), #48488, .F. ) ;
#10525 = VERTEX_POINT ( 'NONE', #9040 ) ;
#10526 = DIRECTION ( 'NONE',  ( -1.000000000000000000, -0.000000000000000000, -0.000000000000000000 ) ) ;
#10527 = CLOSED_SHELL ( 'NONE', ( #1724, #30696, #21741, #34122, #49410, #6815, #41560, #14250, #8115, #11460, #24630, #23401, #29705, #29430, #40561, #49652, #39784, #46766 ) ) ;
#10528 = ORIENTED_EDGE ( 'NONE', *, *, #18636, .F. ) ;
#10529 = EDGE_CURVE ( 'NONE', #31210, #33108, #34976, .T. ) ;
#10530 = CARTESIAN_POINT ( 'NONE',  ( 15.00000000000000000, -46.51315789473684248, 5.916985404131814619 ) ) ;
#10531 = ORIENTED_EDGE ( 'NONE', *, *, #2428, .T. ) ;
#10532 = CARTESIAN_POINT ( 'NONE',  ( -126.6959734468149321, 0.000000000000000000, -165.0000000000000000 ) ) ;
#10533 = CARTESIAN_POINT ( 'NONE',  ( -0.3370904143228943828, -0.2449105217885308716, 10.00000000000000000 ) ) ;
#10534 = DIRECTION ( 'NONE',  ( 6.203854594147707562E-25, -2.067951531382569187E-25, 1.000000000000000000 ) ) ;
#10535 = DIRECTION ( 'NONE',  ( 1.132880637372608740E-16, 4.718402560806925739E-50, 1.000000000000000000 ) ) ;
#10536 = ORIENTED_EDGE ( 'NONE', *, *, #3239, .T. ) ;
#10537 = VERTEX_POINT ( 'NONE', #32905 ) ;
#10538 = CARTESIAN_POINT ( 'NONE',  ( 191.5540265531851105, 0.000000000000000000, 159.0682875569279702 ) ) ;
#10539 = B_SPLINE_CURVE_WITH_KNOTS ( 'NONE', 3,
 ( #40371, #8818, #20353, #36029 ),
 .UNSPECIFIED., .F., .F.,
 ( 4, 4 ),
 ( 0.001152428489661395028, 0.001623376834729682886 ),
 .UNSPECIFIED. ) ;
#10540 = VERTEX_POINT ( 'NONE', #29291 ) ;
#10541 = ADVANCED_FACE ( 'NONE', ( #13379 ), #8540, .T. ) ;
#10542 = CARTESIAN_POINT ( 'NONE',  ( -18.79997501618753830, -32.48828710620296789, 6.057468652304065060 ) ) ;
#10543 = CARTESIAN_POINT ( 'NONE',  ( 0.3656201545664388708, -2.182515578491310393, 9.881002359080277131 ) ) ;
#10544 = ORIENTED_EDGE ( 'NONE', *, *, #17490, .F. ) ;
#10545 = CARTESIAN_POINT ( 'NONE',  ( 153.3040265531850537, 1.750000000000010658, -79.18171244307201562 ) ) ;
#10546 = ORIENTED_EDGE ( 'NONE', *, *, #21182, .F. ) ;
#10547 = CARTESIAN_POINT ( 'NONE',  ( -1.917969350850688315, 0.3547183498317107442, 9.896382706792438810 ) ) ;
#10548 = AXIS2_PLACEMENT_3D ( 'NONE', #22190, #14218, #42428 ) ;
#10549 = CARTESIAN_POINT ( 'NONE',  ( -1.011271242968677875, -0.7347315653656004697, 10.00000000000000000 ) ) ;
#10550 = LINE ( 'NONE', #6451, #13168 ) ;
#10551 = CARTESIAN_POINT ( 'NONE',  ( 210.0000000000000568, 0.000000000000000000, 162.5682875569279702 ) ) ;
#10552 = AXIS2_PLACEMENT_3D ( 'NONE', #48464, #48712, #18201 ) ;
#10553 = VERTEX_POINT ( 'NONE', #844 ) ;
#10554 = LINE ( 'NONE', #49260, #26942 ) ;
#10555 = AXIS2_PLACEMENT_3D ( 'NONE', #1873, #37046, #28560 ) ;
#10556 = AXIS2_PLACEMENT_3D ( 'NONE', #3603, #46162, #18233 ) ;
#10557 =( NAMED_UNIT ( * ) PLANE_ANGLE_UNIT ( ) SI_UNIT ( $, .RADIAN. ) );
#10558 = ADVANCED_FACE ( 'NONE', ( #13128, #39853 ), #24945, .T. ) ;
#10559 = CARTESIAN_POINT ( 'NONE',  ( -4.999999999999948486, -204.9999999999999716, -230.2499999999999716 ) ) ;
#10560 = VECTOR ( 'NONE', #24153, 1000.000000000000000 ) ;
#10561 = ORIENTED_EDGE ( 'NONE', *, *, #50415, .F. ) ;
#10562 = ORIENTED_EDGE ( 'NONE', *, *, #46361, .F. ) ;
#10563 = DIRECTION ( 'NONE',  ( -6.982962677686266711E-15, -1.396592535537253342E-14, -1.000000000000000000 ) ) ;
#10565 = CARTESIAN_POINT ( 'NONE',  ( -126.6959734468149321, 0.000000000000000000, 165.0000000000000000 ) ) ;
#10564 = VECTOR ( 'NONE', #46971, 1000.000000000000000 ) ;
#10566 = DIRECTION ( 'NONE',  ( -1.000000000000000000, -0.000000000000000000, -0.000000000000000000 ) ) ;
#10567 = CARTESIAN_POINT ( 'NONE',  ( 168.9999999999999716, -268.4999999999999432, -339.9999999999998863 ) ) ;
#10568 = FACE_OUTER_BOUND ( 'NONE', #17572, .T. ) ;
#10569 = FACE_OUTER_BOUND ( 'NONE', #33163, .T. ) ;
#10570 = ORIENTED_EDGE ( 'NONE', *, *, #4439, .T. ) ;
#10571 = CARTESIAN_POINT ( 'NONE',  ( 71.55402655318505367, -1.025126265847089435, 39.06828755692797728 ) ) ;
#10572 = PRODUCT_DEFINITION_SHAPE ( 'NONE', 'NONE',  #26547 ) ;
#10573 = DIRECTION ( 'NONE',  ( -0.6904757466825006684, 0.7233555441435720601, 0.000000000000000000 ) ) ;
#10574 = EDGE_CURVE ( 'NONE', #17433, #3732, #43919, .T. ) ;
#10575 = CARTESIAN_POINT ( 'NONE',  ( 349.9999999999999432, -180.9999999999999716, 357.9999999999997726 ) ) ;
#10576 = ADVANCED_FACE ( 'NONE', ( #36002 ), #16488, .F. ) ;
#10577 = ORIENTED_EDGE ( 'NONE', *, *, #10053, .T. ) ;
#10578 = DIRECTION ( 'NONE',  ( -0.2599384441937612200, -0.8000082703740950540, -0.5407575913134975432 ) ) ;
#10579 = ORIENTED_EDGE ( 'NONE', *, *, #30205, .T. ) ;
#10580 = CARTESIAN_POINT ( 'NONE',  ( -14.99999999999876366, 17.00000000000000000, 30.00000000000000000 ) ) ;
#10581 = CARTESIAN_POINT ( 'NONE',  ( 181.0000000000000000, -254.4999999999999432, -339.9999999999998863 ) ) ;
#10582 =( BOUNDED_CURVE ( )  B_SPLINE_CURVE ( 3, ( #14698, #45966, #18278, #26503 ),
 .UNSPECIFIED., .F., .F. ) 
 B_SPLINE_CURVE_WITH_KNOTS ( ( 4, 4 ),
 ( 1.570796326794896558, 3.141592653589793116 ),
 .UNSPECIFIED. ) 
 CURVE ( )  GEOMETRIC_REPRESENTATION_ITEM ( )  RATIONAL_B_SPLINE_CURVE ( ( 1.000000000000000000, 0.8047378541243649375, 0.8047378541243649375, 1.000000000000000000 ) ) 
 REPRESENTATION_ITEM ( '' )  );
#10583 = EDGE_CURVE ( 'NONE', #19479, #35494, #5679, .T. ) ;
#10584 = FACE_OUTER_BOUND ( 'NONE', #13014, .T. ) ;
#10585 = ORIENTED_EDGE ( 'NONE', *, *, #23297, .T. ) ;
#10586 = EDGE_CURVE ( 'NONE', #43944, #40512, #6950, .T. ) ;
#10587 = CIRCLE ( 'NONE', #17151, 4.000000000000003553 ) ;
#10588 = EDGE_CURVE ( 'NONE', #28991, #218, #30058, .T. ) ;
#10589 = B_SPLINE_CURVE_WITH_KNOTS ( 'NONE', 3,
 ( #225, #50457, #38715, #27667 ),
 .UNSPECIFIED., .F., .F.,
 ( 4, 4 ),
 ( 0.9890644561682319091, 1.000000000000000000 ),
 .UNSPECIFIED. ) ;
#10590 = VECTOR ( 'NONE', #15446, 1000.000000000000114 ) ;
#10591 = DIRECTION ( 'NONE',  ( 0.000000000000000000, 0.000000000000000000, -1.000000000000000000 ) ) ;
#10592 = EDGE_LOOP ( 'NONE', ( #48221, #34760, #46414, #27155 ) ) ;
#10593 = CARTESIAN_POINT ( 'NONE',  ( -164.9459734468149463, 2.143131898507880377E-16, 2.568287556927978166 ) ) ;
#10594 = DIRECTION ( 'NONE',  ( 0.000000000000000000, -1.000000000000000000, 2.537652627714642000E-15 ) ) ;
#10595 = CIRCLE ( 'NONE', #5687, 2.000000000000001776 ) ;
#10596 = FACE_OUTER_BOUND ( 'NONE', #45122, .T. ) ;
#10597 = CIRCLE ( 'NONE', #11408, 4.000000000000003553 ) ;
#10598 = EDGE_CURVE ( 'NONE', #31678, #29962, #21853, .T. ) ;
#10599 = ORIENTED_EDGE ( 'NONE', *, *, #25378, .F. ) ;
#10600 = VERTEX_POINT ( 'NONE', #25698 ) ;
#10601 = CARTESIAN_POINT ( 'NONE',  ( 339.9999999999999432, 169.0000000000000000, -344.0000000000001705 ) ) ;
#10602 = VECTOR ( 'NONE', #45462, 1000.000000000000000 ) ;
#10603 = EDGE_LOOP ( 'NONE', ( #14283, #22505, #36317, #16123, #41540, #50252, #49482, #14904, #27974, #50566, #14044, #36094, #4274, #18683, #35581 ) ) ;
#10604 = VERTEX_POINT ( 'NONE', #22598 ) ;
#10605 = DIRECTION ( 'NONE',  ( 0.000000000000000000, 0.000000000000000000, 1.000000000000000000 ) ) ;
#10606 = CARTESIAN_POINT ( 'NONE',  ( -0.5000000000000000000, -0.5000000000000000000, 1000.000000000000000 ) ) ;
#10607 = CARTESIAN_POINT ( 'NONE',  ( 210.0000000000000568, 0.000000000000000000, 0.8182875569279768335 ) ) ;
#10608 = ORIENTED_EDGE ( 'NONE', *, *, #33976, .T. ) ;
#10609 = DIRECTION ( 'NONE',  ( -1.000000000000000000, 0.000000000000000000, 0.000000000000000000 ) ) ;
#10610 = ORIENTED_EDGE ( 'NONE', *, *, #29275, .F. ) ;
#10611 = CARTESIAN_POINT ( 'NONE',  ( -14.99999999999845812, 17.00000000000000000, 60.00000000000000000 ) ) ;
#10612 = DIRECTION ( 'NONE',  ( 1.000000000000000000, 0.000000000000000000, -0.000000000000000000 ) ) ;
#10613 = ORIENTED_EDGE ( 'NONE', *, *, #50050, .T. ) ;
#10614 = ORIENTED_EDGE ( 'NONE', *, *, #7011, .F. ) ;
#10615 = EDGE_LOOP ( 'NONE', ( #21316, #23122, #48569, #41107 ) ) ;
#10616 = CARTESIAN_POINT ( 'NONE',  ( -0.4500758073841509277, -0.7003689023519117374, 9.985686052694763504 ) ) ;
#10617 = CARTESIAN_POINT ( 'NONE',  ( -208.4459734468149463, 0.000000000000000000, -157.4317124430720582 ) ) ;
#10618 = ORIENTED_EDGE ( 'NONE', *, *, #30207, .F. ) ;
#10619 = CARTESIAN_POINT ( 'NONE',  ( 359.9999999999999432, -174.9999999999999432, 355.9999999999998295 ) ) ;
#10621 = EDGE_LOOP ( 'NONE', ( #11422, #7723, #18595 ) ) ;
#10620 = VECTOR ( 'NONE', #34338, 1000.000000000000000 ) ;
#10622 = EDGE_CURVE ( 'NONE', #50239, #3325, #49034, .T. ) ;
#10623 = PLANE ( 'NONE',  #40550 ) ;
#10625 = ORIENTED_EDGE ( 'NONE', *, *, #35773, .T. ) ;
#10624 = VECTOR ( 'NONE', #9701, 1000.000000000000000 ) ;
#10626 = DIRECTION ( 'NONE',  ( -1.000000000000000000, 0.000000000000000000, 0.000000000000000000 ) ) ;
#10627 = DIRECTION ( 'NONE',  ( 1.000000000000000000, 0.000000000000000000, 0.000000000000000000 ) ) ;
#10628 = DIRECTION ( 'NONE',  ( 1.000000000000000000, 0.000000000000000000, 0.000000000000000000 ) ) ;
#10629 = CARTESIAN_POINT ( 'NONE',  ( -64.99999999999940314, 16.00000000000000000, -30.00000000000000000 ) ) ;
#10630 = VECTOR ( 'NONE', #18087, 1000.000000000000000 ) ;
#10631 = CARTESIAN_POINT ( 'NONE',  ( -206.6959734468149463, 0.000000000000000000, 165.0000000000000000 ) ) ;
#10632 = EDGE_LOOP ( 'NONE', ( #45945, #21619 ) ) ;
#10634 = CIRCLE ( 'NONE', #32769, 1.750000000000015543 ) ;
#10633 = CARTESIAN_POINT ( 'NONE',  ( 153.3040265531850537, -1.750000000000009992, -159.1817124430720298 ) ) ;
#10635 = CARTESIAN_POINT ( 'NONE',  ( -2.143303323993650533, 0.2858885274054065451, 9.882710035074774524 ) ) ;
#10636 = CARTESIAN_POINT ( 'NONE',  ( -165.6708471809677974, -1.750000000000009548, 121.8434138227750623 ) ) ;
#10637 = CARTESIAN_POINT ( 'NONE',  ( 210.0000000000000568, 0.000000000000000000, 122.5682875569279844 ) ) ;
#10638 = VECTOR ( 'NONE', #27007, 1000.000000000000000 ) ;
#10639 = CARTESIAN_POINT ( 'NONE',  ( -1.962558162477761714, 3.366505435501197407, 9.741991644046970933 ) ) ;
#10640 = CARTESIAN_POINT ( 'NONE',  ( -543.3973046169135159, 54.43801056904003133, -177.1374399499827916 ) ) ;
#10641 = EDGE_CURVE ( 'NONE', #28669, #5426, #50460, .T. ) ;
#10642 = CARTESIAN_POINT ( 'NONE',  ( 33.30402655318503946, -1.750000000000010658, -79.18171244307201562 ) ) ;
#10643 = CARTESIAN_POINT ( 'NONE',  ( 339.9999999999999432, -180.9999999999999716, -344.0000000000001705 ) ) ;
#10644 = CARTESIAN_POINT ( 'NONE',  ( 111.5540265531850537, 2.143131898507880377E-16, -160.9317124430720298 ) ) ;
#10645 = ADVANCED_FACE ( 'NONE', ( #45154 ), #45664, .T. ) ;
#10646 = EDGE_CURVE ( 'NONE', #15843, #38289, #35991, .T. ) ;
#10647 = ORIENTED_EDGE ( 'NONE', *, *, #26581, .T. ) ;
#10648 = FACE_OUTER_BOUND ( 'NONE', #9608, .T. ) ;
#10649 = CARTESIAN_POINT ( 'NONE',  ( 17.51065725283126895, -28.41934970907778890, -9.367992836599954742 ) ) ;
#10650 = CARTESIAN_POINT ( 'NONE',  ( 50.00000000000000000, 0.000000000000000000, 800.0000000000000000 ) ) ;
#10651 = ADVANCED_FACE ( 'NONE', ( #13867 ), #37526, .T. ) ;
#10652 = CARTESIAN_POINT ( 'NONE',  ( 39.35269538308637038, -42.31198943095992604, 742.8425600500171413 ) ) ;
#10653 = CARTESIAN_POINT ( 'NONE',  ( -0.8431937073480634259, 1.111389989012122825, 9.955131761384899747 ) ) ;
#10654 = ORIENTED_EDGE ( 'NONE', *, *, #48394, .F. ) ;
#10655 = ORIENTED_EDGE ( 'NONE', *, *, #45948, .T. ) ;
#10656 = AXIS2_PLACEMENT_3D ( 'NONE', #33843, #25883, #2522 ) ;
#10657 = CARTESIAN_POINT ( 'NONE',  ( -119.9999999999984652, 16.00000000000000000, 60.00000000000000000 ) ) ;
#10658 = AXIS2_PLACEMENT_3D ( 'NONE', #49484, #22577, #37258 ) ;
#10659 = ORIENTED_EDGE ( 'NONE', *, *, #32652, .F. ) ;
#10660 = CARTESIAN_POINT ( 'NONE',  ( -35.51846793572368455, 35.99772139009146343, 7.906207997025717304 ) ) ;
#10661 = AXIS2_PLACEMENT_3D ( 'NONE', #48829, #5522, #32996 ) ;
#10662 = CARTESIAN_POINT ( 'NONE',  ( 191.5540265531850537, -1.025126265847089435, 2.568287556927986159 ) ) ;
#10663 = CARTESIAN_POINT ( 'NONE',  ( -543.3973046169135159, -62.56198943095993315, -177.1374399499827916 ) ) ;
#10664 = AXIS2_PLACEMENT_3D ( 'NONE', #44002, #44753, #28376 ) ;
#10665 = ORIENTED_EDGE ( 'NONE', *, *, #25201, .T. ) ;
#10666 = ORIENTED_EDGE ( 'NONE', *, *, #3543, .F. ) ;
#10667 = AXIS2_PLACEMENT_3D ( 'NONE', #25328, #41221, #41730 ) ;
#10668 = ORIENTED_EDGE ( 'NONE', *, *, #27087, .T. ) ;
#10669 = VECTOR ( 'NONE', #35714, 1000.000000000000000 ) ;
#10670 = FACE_OUTER_BOUND ( 'NONE', #31781, .T. ) ;
#10671 = DIRECTION ( 'NONE',  ( 0.000000000000000000, -1.000000000000000000, 0.000000000000000000 ) ) ;
#10672 = CARTESIAN_POINT ( 'NONE',  ( 18.67411147745603373, 27.51799019669827473, -3.760136334089591248 ) ) ;
#10673 = VECTOR ( 'NONE', #8220, 1000.000000000000000 ) ;
#10674 = EDGE_LOOP ( 'NONE', ( #25649, #44963, #20366 ) ) ;
#10675 = CARTESIAN_POINT ( 'NONE',  ( 0.000000000000000000, 175.0000000000000284, -346.2500000000002274 ) ) ;
#10676 = DIRECTION ( 'NONE',  ( 0.000000000000000000, 0.000000000000000000, -1.000000000000000000 ) ) ;
#10677 = CARTESIAN_POINT ( 'NONE',  ( -6.880036658038864772, 197.4999999999999432, -228.6347188485896140 ) ) ;
#10678 = EDGE_LOOP ( 'NONE', ( #7193, #39157, #24508, #46612, #9300, #47349 ) ) ;
#10679 = ORIENTED_EDGE ( 'NONE', *, *, #45717, .T. ) ;
#10680 = DIRECTION ( 'NONE',  ( -0.000000000000000000, -0.000000000000000000, -1.000000000000000000 ) ) ;
#10681 = CARTESIAN_POINT ( 'NONE',  ( -48.99656738986512039, 11.00747004110376182, 1.847720168420772691 ) ) ;
#10682 = CARTESIAN_POINT ( 'NONE',  ( -47.72109971266203132, 1.750000000000009548, -40.20683870891912193 ) ) ;
#10683 = ORIENTED_EDGE ( 'NONE', *, *, #8964, .T. ) ;
#10684 = ORIENTED_EDGE ( 'NONE', *, *, #4927, .F. ) ;
#10685 = EDGE_CURVE ( 'NONE', #32767, #19888, #10123, .T. ) ;
#10686 = PLANE ( 'NONE',  #24194 ) ;
#10687 = CARTESIAN_POINT ( 'NONE',  ( 153.2026953830863647, 103.0380105690400683, 23.74256005001722158 ) ) ;
#10688 = DIRECTION ( 'NONE',  ( -0.000000000000000000, -0.000000000000000000, -1.000000000000000000 ) ) ;
#10689 = CARTESIAN_POINT ( 'NONE',  ( -1.250000000000000222, 0.000000000000000000, 10.00000000000000000 ) ) ;
#10690 = ORIENTED_EDGE ( 'NONE', *, *, #16557, .F. ) ;
#10691 = CARTESIAN_POINT ( 'NONE',  ( 34.38425513258721367, -36.82177522737821107, 8.807470649214879543 ) ) ;
#10692 = CARTESIAN_POINT ( 'NONE',  ( -46.69597344681494633, 1.750000000000010658, -119.1817124430720440 ) ) ;
#10693 = CARTESIAN_POINT ( 'NONE',  ( -167.7210997126620384, 1.750000000000009548, -0.2068387089191121020 ) ) ;
#10694 = AXIS2_PLACEMENT_3D ( 'NONE', #34588, #27395, #50170 ) ;
#10695 = CYLINDRICAL_SURFACE ( 'NONE', #46772, 1.750000000000008438 ) ;
#10696 = AXIS2_PLACEMENT_3D ( 'NONE', #30735, #50161, #38689 ) ;
#10697 = CARTESIAN_POINT ( 'NONE',  ( 185.0000000000000284, -174.9999999999999716, -111.0000000000001563 ) ) ;
#10698 = EDGE_LOOP ( 'NONE', ( #28094, #3684, #21917, #40204 ) ) ;
#10699 = DIRECTION ( 'NONE',  ( -1.000000000000000000, -0.000000000000000000, -0.000000000000000000 ) ) ;
#10700 = VECTOR ( 'NONE', #31725, 1000.000000000000000 ) ;
#10701 = CARTESIAN_POINT ( 'NONE',  ( -45.21167770612412085, -22.65616271077779942, 7.906207997025717304 ) ) ;
#10702 = COLOUR_RGB ( '',0.7921568627450980005, 0.8196078431372548767, 0.9333333333333333481 ) ;
#10703 = FACE_OUTER_BOUND ( 'NONE', #46615, .T. ) ;
#10704 = VERTEX_POINT ( 'NONE', #49499 ) ;
#10705 = FACE_OUTER_BOUND ( 'NONE', #35812, .T. ) ;
#10706 = CYLINDRICAL_SURFACE ( 'NONE', #2426, 1.750000000000001554 ) ;
#10707 = ORIENTED_EDGE ( 'NONE', *, *, #13656, .F. ) ;
#10708 = CARTESIAN_POINT ( 'NONE',  ( -48.44597344681495343, 0.000000000000000000, 39.06828755692798438 ) ) ;
#10709 = EDGE_CURVE ( 'NONE', #29620, #40413, #23490, .T. ) ;
#10710 = DIRECTION ( 'NONE',  ( -0.000000000000000000, -1.000000000000000000, -0.000000000000000000 ) ) ;
#10711 = FACE_OUTER_BOUND ( 'NONE', #47867, .T. ) ;
#10712 = VERTEX_POINT ( 'NONE', #42086 ) ;
#10713 = CARTESIAN_POINT ( 'NONE',  ( 210.0000000000000568, 0.000000000000000000, 160.8182875569279702 ) ) ;
#10714 = ORIENTED_EDGE ( 'NONE', *, *, #7810, .T. ) ;
#10715 = ORIENTED_EDGE ( 'NONE', *, *, #18836, .T. ) ;
#10716 = CARTESIAN_POINT ( 'NONE',  ( -6.695973446814940111, -1.750000000000024203, -119.1817124430720440 ) ) ;
#10717 =( BOUNDED_CURVE ( )  B_SPLINE_CURVE ( 3, ( #10840, #6997, #329, #26752 ),
 .UNSPECIFIED., .F., .F. ) 
 B_SPLINE_CURVE_WITH_KNOTS ( ( 4, 4 ),
 ( 1.570796326794896558, 3.141592653589793116 ),
 .UNSPECIFIED. ) 
 CURVE ( )  GEOMETRIC_REPRESENTATION_ITEM ( )  RATIONAL_B_SPLINE_CURVE ( ( 1.000000000000000000, 0.8047378541243649375, 0.8047378541243649375, 1.000000000000000000 ) ) 
 REPRESENTATION_ITEM ( '' )  );
#10718 = ORIENTED_EDGE ( 'NONE', *, *, #25802, .F. ) ;
#10719 = DIRECTION ( 'NONE',  ( -0.000000000000000000, -0.000000000000000000, 1.000000000000000000 ) ) ;
#10720 = DIRECTION ( 'NONE',  ( -0.000000000000000000, -0.000000000000000000, -1.000000000000000000 ) ) ;
#10721 = LINE ( 'NONE', #20134, #43341 ) ;
#10722 = CARTESIAN_POINT ( 'NONE',  ( -4.945973446814903696, 2.143131898507912917E-16, 119.0682875569279418 ) ) ;
#10723 =( BOUNDED_CURVE ( )  B_SPLINE_CURVE ( 3, ( #12355, #31633, #13110, #24431 ),
 .UNSPECIFIED., .F., .F. ) 
 B_SPLINE_CURVE_WITH_KNOTS ( ( 4, 4 ),
 ( 0.000000000000000000, 1.570796326794896558 ),
 .UNSPECIFIED. ) 
 CURVE ( )  GEOMETRIC_REPRESENTATION_ITEM ( )  RATIONAL_B_SPLINE_CURVE ( ( 1.000000000000000000, 0.8047378541243649375, 0.8047378541243649375, 1.000000000000000000 ) ) 
 REPRESENTATION_ITEM ( '' )  );
#10724 = CARTESIAN_POINT ( 'NONE',  ( 3.893440183625898054, 0.6391102933654070339, 6.494306319013603890 ) ) ;
#10725 = EDGE_LOOP ( 'NONE', ( #914, #47443, #43739 ) ) ;
#10726 = EDGE_CURVE ( 'NONE', #25574, #42832, #3087, .T. ) ;
#10727 = DIRECTION ( 'NONE',  ( -1.000000000000000000, 0.000000000000000000, 0.000000000000000000 ) ) ;
#10728 = AXIS2_PLACEMENT_3D ( 'NONE', #17800, #37576, #2400 ) ;
#10729 = CYLINDRICAL_SURFACE ( 'NONE', #16775, 1.750000000000008438 ) ;
#10730 = ORIENTED_EDGE ( 'NONE', *, *, #50611, .T. ) ;
#10731 = DIRECTION ( 'NONE',  ( 0.000000000000000000, 0.000000000000000000, 1.000000000000000000 ) ) ;
#10732 = LINE ( 'NONE', #6895, #36012 ) ;
#10733 = ORIENTED_EDGE ( 'NONE', *, *, #9038, .F. ) ;
#10734 = ORIENTED_EDGE ( 'NONE', *, *, #4524, .T. ) ;
#10735 = ORIENTED_EDGE ( 'NONE', *, *, #45665, .F. ) ;
#10736 = LINE ( 'NONE', #21793, #47487 ) ;
#10737 = VECTOR ( 'NONE', #738, 1000.000000000000000 ) ;
#10738 =( BOUNDED_CURVE ( )  B_SPLINE_CURVE ( 3, ( #32737, #37370, #24793, #501 ),
 .UNSPECIFIED., .F., .F. ) 
 B_SPLINE_CURVE_WITH_KNOTS ( ( 4, 4 ),
 ( 3.169317492284500903E-16, 1.570796326794903663 ),
 .UNSPECIFIED. ) 
 CURVE ( )  GEOMETRIC_REPRESENTATION_ITEM ( )  RATIONAL_B_SPLINE_CURVE ( ( 1.000000000000000000, 0.8047378541243634942, 0.8047378541243634942, 1.000000000000000000 ) ) 
 REPRESENTATION_ITEM ( '' )  );
#10739 = CARTESIAN_POINT ( 'NONE',  ( 31.44259251615245887, 38.95901822126168668, -9.367992836599954742 ) ) ;
#10740 = AXIS2_PLACEMENT_3D ( 'NONE', #19363, #15274, #38885 ) ;
#10741 = EDGE_CURVE ( 'NONE', #30190, #11666, #35787, .T. ) ;
#10742 = ORIENTED_EDGE ( 'NONE', *, *, #38708, .F. ) ;
#10743 = CARTESIAN_POINT ( 'NONE',  ( 236.0000000000000000, -169.9999999999999716, 62.29650858650038003 ) ) ;
#10744 = LINE ( 'NONE', #43567, #45197 ) ;
#10745 = ADVANCED_FACE ( 'NONE', ( #33410 ), #50246, .F. ) ;
#10746 = CARTESIAN_POINT ( 'NONE',  ( -567.5000000000000000, 57.49999999999996447, -183.5999999999997954 ) ) ;
#10747 = DIRECTION ( 'NONE',  ( 0.000000000000000000, -0.000000000000000000, 1.000000000000000000 ) ) ;
#10748 = ORIENTED_EDGE ( 'NONE', *, *, #46572, .F. ) ;
#10749 = CARTESIAN_POINT ( 'NONE',  ( 350.0000000000000000, -166.9999999999999432, -356.0000000000002274 ) ) ;
#10750 = CARTESIAN_POINT ( 'NONE',  ( 15.80799809827373004, -29.65358618225706522, -8.016098858316199838 ) ) ;
#10751 = CARTESIAN_POINT ( 'NONE',  ( -22.69295089195507487, -45.31600496604688999, 7.455576670931136185 ) ) ;
#10752 = ORIENTED_EDGE ( 'NONE', *, *, #12170, .F. ) ;
#10753 = CONTEXT_DEPENDENT_SHAPE_REPRESENTATION ( #25987, #15104 ) ;
#10754 = CARTESIAN_POINT ( 'NONE',  ( 71.55402655318505367, 0.000000000000000000, 165.0000000000000000 ) ) ;
#10755 = DIRECTION ( 'NONE',  ( -1.000000000000000000, 0.000000000000000000, 0.000000000000000000 ) ) ;
#10756 = DIRECTION ( 'NONE',  ( 0.000000000000000000, 0.000000000000000000, -1.000000000000000000 ) ) ;
#10757 = CARTESIAN_POINT ( 'NONE',  ( 153.2026953830863647, 70.03596893647589638, -93.79675437945476801 ) ) ;
#10758 = VERTEX_POINT ( 'NONE', #22844 ) ;
#10759 = DIRECTION ( 'NONE',  ( -1.000000000000000000, 0.000000000000000000, 0.000000000000000000 ) ) ;
#10760 = CARTESIAN_POINT ( 'NONE',  ( 7.749480817862238524, 14.85497772329518895, 9.403735324607438884 ) ) ;
#10761 = VECTOR ( 'NONE', #2897, 1000.000000000000000 ) ;
#10762 = CARTESIAN_POINT ( 'NONE',  ( 15.62858259096121216, -5.755205073598614440, -9.683996418299976483 ) ) ;
#10763 = FACE_OUTER_BOUND ( 'NONE', #21919, .T. ) ;
#10764 = CARTESIAN_POINT ( 'NONE',  ( -86.69597344681494633, 1.750000000000009992, 160.8182875569279702 ) ) ;
#10765 = VECTOR ( 'NONE', #27173, 1000.000000000000000 ) ;
#10766 = ORIENTED_EDGE ( 'NONE', *, *, #12405, .F. ) ;
#10767 = ADVANCED_FACE ( 'NONE', ( #38522 ), #12072, .F. ) ;
#10768 = CARTESIAN_POINT ( 'NONE',  ( -48.44597344681495343, 0.000000000000000000, 122.5682875569279702 ) ) ;
#10769 = ORIENTED_EDGE ( 'NONE', *, *, #37161, .T. ) ;
#10770 = EDGE_CURVE ( 'NONE', #37345, #5556, #6278, .T. ) ;
#10771 = CARTESIAN_POINT ( 'NONE',  ( -15.00000000000001421, 16.00000000000000000, -90.00000000000000000 ) ) ;
#10772 = ORIENTED_EDGE ( 'NONE', *, *, #46373, .T. ) ;
#10773 = CARTESIAN_POINT ( 'NONE',  ( 339.9999999999998863, -181.0000000000001990, -356.0000000000003411 ) ) ;
#10774 = ADVANCED_FACE ( 'NONE', ( #20010 ), #7206, .T. ) ;
#10775 = DIRECTION ( 'NONE',  ( 0.000000000000000000, -0.000000000000000000, -1.000000000000000000 ) ) ;
#10776 = AXIS2_PLACEMENT_3D ( 'NONE', #20813, #5163, #36240 ) ;
#10777 = ORIENTED_EDGE ( 'NONE', *, *, #28205, .F. ) ;
#10778 = PRESENTATION_STYLE_ASSIGNMENT (( #22833 ) ) ;
#10779 = EDGE_LOOP ( 'NONE', ( #11239, #17743, #38510, #35016 ) ) ;
#10780 = EDGE_CURVE ( 'NONE', #48126, #38712, #15659, .T. ) ;
#10781 = EDGE_CURVE ( 'NONE', #48255, #13701, #19762, .T. ) ;
#10782 = CARTESIAN_POINT ( 'NONE',  ( 191.5540265531850537, -1.025126265847089879, 82.56828755692798438 ) ) ;
#10783 = EDGE_LOOP ( 'NONE', ( #27144, #17980, #25449, #21626 ) ) ;
#10784 = CARTESIAN_POINT ( 'NONE',  ( 183.0000000000000000, 6.000000000000060396, 339.9999999999998295 ) ) ;
#10785 = CARTESIAN_POINT ( 'NONE',  ( 169.0000000000000000, -174.9999999999999716, -97.00000000000014211 ) ) ;
#10786 = ORIENTED_EDGE ( 'NONE', *, *, #18236, .T. ) ;
#10787 = CARTESIAN_POINT ( 'NONE',  ( 1.011271242968683648, 0.7347315653655930312, 10.00000000000000000 ) ) ;
#10788 = LINE ( 'NONE', #26438, #30832 ) ;
#10789 = LINE ( 'NONE', #50242, #42099 ) ;
#10790 = ORIENTED_EDGE ( 'NONE', *, *, #24617, .F. ) ;
#10791 = ORIENTED_EDGE ( 'NONE', *, *, #23813, .T. ) ;
#10792 = CARTESIAN_POINT ( 'NONE',  ( -0.3862712429686809279, -1.188820645368943163, 10.00000000000000000 ) ) ;
#10793 = EDGE_LOOP ( 'NONE', ( #7268, #42612, #25063, #15459 ) ) ;
#10794 = DIRECTION ( 'NONE',  ( 1.942330104924128867E-32, 0.000000000000000000, 1.000000000000000000 ) ) ;
#10795 = PLANE ( 'NONE',  #11406 ) ;
#10796 = VERTEX_POINT ( 'NONE', #19495 ) ;
#10797 = CARTESIAN_POINT ( 'NONE',  ( -1.052829316634559920, -0.8818324942353437113, 9.946805383069644790 ) ) ;
#10798 = AXIS2_PLACEMENT_3D ( 'NONE', #11321, #26217, #38544 ) ;
#10799 = B_SPLINE_CURVE_WITH_KNOTS ( 'NONE', 3,
 ( #4348, #39507, #38743, #43584 ),
 .UNSPECIFIED., .F., .F.,
 ( 4, 4 ),
 ( 0.003717747231047226469, 0.009855833117593325310 ),
 .UNSPECIFIED. ) ;
#10800 = CARTESIAN_POINT ( 'NONE',  ( -207.7210997126620384, 1.750000000000009548, -78.15658617722490931 ) ) ;
#10801 = EDGE_CURVE ( 'NONE', #4426, #21356, #29154, .T. ) ;
#10802 = ORIENTED_EDGE ( 'NONE', *, *, #42123, .T. ) ;
#10803 = EDGE_CURVE ( 'NONE', #18563, #21707, #7720, .T. ) ;
#10804 = CARTESIAN_POINT ( 'NONE',  ( 35.05402655318504657, -1.025126265847088991, -157.4317124430720582 ) ) ;
#10805 = CARTESIAN_POINT ( 'NONE',  ( 193.3040265531851105, 1.750000000000010658, 120.8182875569279702 ) ) ;
#10806 = CARTESIAN_POINT ( 'NONE',  ( 350.0000000000001137, 165.0000000000000000, 343.9999999999997726 ) ) ;
#10807 = LINE ( 'NONE', #23115, #32955 ) ;
#10808 = EDGE_CURVE ( 'NONE', #8324, #14373, #11050, .T. ) ;
#10809 = ADVANCED_FACE ( 'NONE', ( #23359 ), #42587, .T. ) ;
#10810 = VECTOR ( 'NONE', #35732, 1000.000000000000000 ) ;
#10811 = ORIENTED_EDGE ( 'NONE', *, *, #40157, .T. ) ;
#10812 = DIRECTION ( 'NONE',  ( 0.000000000000000000, -1.000000000000000000, 0.000000000000000000 ) ) ;
#10813 = EDGE_CURVE ( 'NONE', #47424, #49568, #47174, .T. ) ;
#10814 = CARTESIAN_POINT ( 'NONE',  ( -35.51846793572368455, 35.99772139009146343, 7.906207997025717304 ) ) ;
#10815 = EDGE_CURVE ( 'NONE', #28808, #22009, #3515, .T. ) ;
#10816 = CARTESIAN_POINT ( 'NONE',  ( 12.15085308559846844, -11.68662139125803989, 2.590526750877053086 ) ) ;
#10817 = ORIENTED_EDGE ( 'NONE', *, *, #21100, .T. ) ;
#10818 = ORIENTED_EDGE ( 'NONE', *, *, #10217, .T. ) ;
#10819 = DIRECTION ( 'NONE',  ( 3.491481338843035537E-15, 1.000000000000000000, -1.396592535537255866E-14 ) ) ;
#10820 = DIRECTION ( 'NONE',  ( 1.000000000000000000, -0.000000000000000000, 0.000000000000000000 ) ) ;
#10821 = CARTESIAN_POINT ( 'NONE',  ( -194.9999999999999432, 164.9999999999999716, 372.0000000000000000 ) ) ;
#10822 = DIRECTION ( 'NONE',  ( -0.000000000000000000, -0.000000000000000000, 1.000000000000000000 ) ) ;
#10823 = CYLINDRICAL_SURFACE ( 'NONE', #18478, 1.750000000000008438 ) ;
#10824 = PLANE ( 'NONE',  #29868 ) ;
#10825 = CARTESIAN_POINT ( 'NONE',  ( -582.5000000000000000, -72.50000000000001421, -58.60000000000003695 ) ) ;
#10826 = ORIENTED_EDGE ( 'NONE', *, *, #37488, .F. ) ;
#10827 = CARTESIAN_POINT ( 'NONE',  ( -165.0000000000000284, 17.00000000000000000, -90.00000000000000000 ) ) ;
#10828 = DIRECTION ( 'NONE',  ( -0.7233555441435720601, -0.6904757466825006684, 0.000000000000000000 ) ) ;
#10829 = EDGE_CURVE ( 'NONE', #27666, #7870, #18988, .T. ) ;
#10830 = EDGE_CURVE ( 'NONE', #45408, #33571, #15154, .T. ) ;
#10831 = FACE_OUTER_BOUND ( 'NONE', #17866, .T. ) ;
#10832 = ORIENTED_EDGE ( 'NONE', *, *, #40011, .F. ) ;
#10833 = EDGE_CURVE ( 'NONE', #44983, #20782, #35255, .T. ) ;
#10834 = VECTOR ( 'NONE', #28609, 1000.000000000000000 ) ;
#10835 = LINE ( 'NONE', #31370, #20438 ) ;
#10836 = VERTEX_POINT ( 'NONE', #34933 ) ;
#10837 = DIRECTION ( 'NONE',  ( 0.000000000000000000, 0.000000000000000000, 1.000000000000000000 ) ) ;
#10838 = VECTOR ( 'NONE', #48128, 1000.000000000000000 ) ;
#10839 = DIRECTION ( 'NONE',  ( -1.000000000000000000, -0.000000000000000000, -0.000000000000000000 ) ) ;
#10840 = CARTESIAN_POINT ( 'NONE',  ( 193.3040265531851105, -1.750000000000009992, -159.1817124430720298 ) ) ;
#10841 = VERTEX_POINT ( 'NONE', #31067 ) ;
#10842 = COLOUR_RGB ( '',0.7921568627450980005, 0.8196078431372548767, 0.9333333333333333481 ) ;
#10843 = FACE_OUTER_BOUND ( 'NONE', #23138, .T. ) ;
#10844 = VERTEX_POINT ( 'NONE', #46667 ) ;
#10845 = CARTESIAN_POINT ( 'NONE',  ( -0.3862712429686977478, 1.188820645368937390, 3.333333333333333481 ) ) ;
#10846 = LINE ( 'NONE', #41137, #22909 ) ;
#10847 = LINE ( 'NONE', #11620, #1276 ) ;
#10848 = EDGE_CURVE ( 'NONE', #24997, #15604, #46916, .T. ) ;
#10849 = VERTEX_POINT ( 'NONE', #27968 ) ;
#10850 = EDGE_LOOP ( 'NONE', ( #15242, #15535, #34405 ) ) ;
#10851 = CARTESIAN_POINT ( 'NONE',  ( 35.00000000000152767, 17.00000000000000000, 35.00000000000000000 ) ) ;
#10852 = LINE ( 'NONE', #14704, #4191 ) ;
#10853 = VERTEX_POINT ( 'NONE', #28228 ) ;
#10854 = EDGE_LOOP ( 'NONE', ( #36656, #31780, #33923, #26999, #2398, #49852 ) ) ;
#10855 = CARTESIAN_POINT ( 'NONE',  ( 74.32915281903215998, -1.750000000000009548, 161.8434138227750907 ) ) ;
#10856 = DIRECTION ( 'NONE',  ( -1.000000000000000000, -0.000000000000000000, -0.000000000000000000 ) ) ;
#10857 = CARTESIAN_POINT ( 'NONE',  ( -164.9459734468149463, -1.025126265847088991, -157.4317124430720582 ) ) ;
#10858 = ADVANCED_FACE ( 'NONE', ( #36445 ), #33002, .T. ) ;
#10859 = VERTEX_POINT ( 'NONE', #1533 ) ;
#10860 = DIRECTION ( 'NONE',  ( 0.000000000000000000, 1.000000000000000000, -2.537652627714642000E-15 ) ) ;
#10861 = EDGE_LOOP ( 'NONE', ( #49701, #30502, #32988, #7346 ) ) ;
#10862 = VECTOR ( 'NONE', #7792, 1000.000000000000000 ) ;
#10863 = CARTESIAN_POINT ( 'NONE',  ( 358.0000000000000000, -169.0000000000001137, -349.9999999999998863 ) ) ;
#10864 = DIRECTION ( 'NONE',  ( 0.000000000000000000, 5.664403186863042467E-17, 1.000000000000000000 ) ) ;
#10865 = CARTESIAN_POINT ( 'NONE',  ( 1.249999999999999778, 0.000000000000000000, 10.00000000000000000 ) ) ;
#10866 = EDGE_CURVE ( 'NONE', #15922, #26103, #25136, .T. ) ;
#10868 = ORIENTED_EDGE ( 'NONE', *, *, #38076, .F. ) ;
#10867 = EDGE_CURVE ( 'NONE', #16553, #32197, #21876, .T. ) ;
#10869 = ORIENTED_EDGE ( 'NONE', *, *, #28043, .T. ) ;
#10870 = ORIENTED_EDGE ( 'NONE', *, *, #7959, .F. ) ;
#10871 = CARTESIAN_POINT ( 'NONE',  ( 6.204997580903516941, -7.388441598285492518, 230.0000000000000000 ) ) ;
#10872 = VECTOR ( 'NONE', #23058, 1000.000000000000000 ) ;
#10873 = CARTESIAN_POINT ( 'NONE',  ( -45.42829307628559832, -21.98948915213271960, 8.356839323120299312 ) ) ;
#10874 = EDGE_CURVE ( 'NONE', #43954, #3318, #36187, .T. ) ;
#10875 = ORIENTED_EDGE ( 'NONE', *, *, #37487, .F. ) ;
#10876 = DIRECTION ( 'NONE',  ( 0.000000000000000000, 0.000000000000000000, 1.000000000000000000 ) ) ;
#10877 = ORIENTED_EDGE ( 'NONE', *, *, #46137, .T. ) ;
#10878 = VECTOR ( 'NONE', #13354, 1000.000000000000000 ) ;
#10879 = EDGE_CURVE ( 'NONE', #23358, #3329, #40280, .T. ) ;
#10880 = ORIENTED_EDGE ( 'NONE', *, *, #34146, .F. ) ;
#10881 = ADVANCED_FACE ( 'NONE', ( #20764, #13062 ), #28729, .T. ) ;
#10882 = CARTESIAN_POINT ( 'NONE',  ( 155.0540265531850537, 2.143131898507890731E-16, 165.0000000000000000 ) ) ;
#10883 = LINE ( 'NONE', #30394, #5558 ) ;
#10884 = FACE_OUTER_BOUND ( 'NONE', #27356, .T. ) ;
#10885 = FACE_OUTER_BOUND ( 'NONE', #41197, .T. ) ;
#10886 = VECTOR ( 'NONE', #16522, 1000.000000000000000 ) ;
#10887 = CARTESIAN_POINT ( 'NONE',  ( 31.55402655318503236, 0.000000000000000000, -77.43171244307198720 ) ) ;
#10888 = ORIENTED_EDGE ( 'NONE', *, *, #7021, .T. ) ;
#10889 = CARTESIAN_POINT ( 'NONE',  ( 153.3040265531850537, -1.750000000000010658, 120.8182875569279702 ) ) ;
#10890 = CARTESIAN_POINT ( 'NONE',  ( 154.3291528190321458, -1.750000000000009548, 161.8434138227750907 ) ) ;
#10891 = EDGE_CURVE ( 'NONE', #20980, #7223, #48441, .T. ) ;
#10892 =( BOUNDED_CURVE ( )  B_SPLINE_CURVE ( 3, ( #17747, #9289, #13872, #17245 ),
 .UNSPECIFIED., .F., .F. ) 
 B_SPLINE_CURVE_WITH_KNOTS ( ( 4, 4 ),
 ( 3.141592653589793116, 4.712388980384689674 ),
 .UNSPECIFIED. ) 
 CURVE ( )  GEOMETRIC_REPRESENTATION_ITEM ( )  RATIONAL_B_SPLINE_CURVE ( ( 1.000000000000000000, 0.8047378541243649375, 0.8047378541243649375, 1.000000000000000000 ) ) 
 REPRESENTATION_ITEM ( '' )  );
#10893 = B_SPLINE_SURFACE_WITH_KNOTS ( 'NONE', 3, 3, ( 
 ( #28310, #32420, #48015, #44192 ),
 ( #24723, #40370, #20856, #36539 ),
 ( #48264, #28816, #44437, #9313 ),
 ( #24975, #9806, #45183, #18004 ) ),
 .UNSPECIFIED., .F., .F., .F.,
 ( 4, 4 ),
 ( 4, 4 ),
 ( 0.000000000000000000, 1.000000000000000000 ),
 ( 0.000000000000000000, 1.000000000000000000 ),
 .UNSPECIFIED. ) ;
#10894 = DIRECTION ( 'NONE',  ( 0.000000000000000000, 0.000000000000000000, 1.000000000000000000 ) ) ;
#10895 = CYLINDRICAL_SURFACE ( 'NONE', #49494, 4.000000000000003553 ) ;
#10896 = CARTESIAN_POINT ( 'NONE',  ( -5.000000000000000000, 184.8000000000000114, 340.1999999999997044 ) ) ;
#10897 = CARTESIAN_POINT ( 'NONE',  ( 153.3040265531850537, -1.750000000000009992, 0.8182875569279768335 ) ) ;
#10898 = DIRECTION ( 'NONE',  ( -0.000000000000000000, -0.000000000000000000, -1.000000000000000000 ) ) ;
#10899 = LINE ( 'NONE', #2690, #27128 ) ;
#10900 = ORIENTED_EDGE ( 'NONE', *, *, #16846, .F. ) ;
#10901 = CARTESIAN_POINT ( 'NONE',  ( 3.441214337941712387, -1.549069628443871860, 9.865049507598753209 ) ) ;
#10902 = PLANE ( 'NONE',  #19673 ) ;
#10903 = AXIS2_PLACEMENT_3D ( 'NONE', #27137, #35613, #42755 ) ;
#10904 = APPLICATION_CONTEXT ( 'automotive_design' ) ;
#10905 = CARTESIAN_POINT ( 'NONE',  ( 331.7552636306688214, 248.6897383013408387, 297.1446280767819985 ) ) ;
#10906 = VERTEX_POINT ( 'NONE', #4855 ) ;
#10907 = VERTEX_POINT ( 'NONE', #20516 ) ;
#10908 = CARTESIAN_POINT ( 'NONE',  ( -10.00000000000000000, 0.000000000000000000, 0.000000000000000000 ) ) ;
#10910 = ADVANCED_FACE ( 'NONE', ( #24877, #32334 ), #40528, .T. ) ;
#10909 = VECTOR ( 'NONE', #45581, 1000.000000000000000 ) ;
#10911 = CARTESIAN_POINT ( 'NONE',  ( 71.55402655318505367, -1.025126265847089657, 119.0682875569279560 ) ) ;
#10912 = ORIENTED_EDGE ( 'NONE', *, *, #35665, .T. ) ;
#10913 = VECTOR ( 'NONE', #22440, 1000.000000000000000 ) ;
#10914 = ORIENTED_EDGE ( 'NONE', *, *, #21144, .F. ) ;
#10915 = DIRECTION ( 'NONE',  ( -0.000000000000000000, -1.000000000000000000, -0.000000000000000000 ) ) ;
#10916 = LINE ( 'NONE', #46284, #37240 ) ;
#10917 = PLANE ( 'NONE',  #16874 ) ;
#10918 = EDGE_LOOP ( 'NONE', ( #14148, #36766, #10544, #40916, #33946, #28719 ) ) ;
#10919 = ORIENTED_EDGE ( 'NONE', *, *, #25664, .T. ) ;
#10920 = ORIENTED_EDGE ( 'NONE', *, *, #23584, .T. ) ;
#10921 = LINE ( 'NONE', #38396, #11054 ) ;
#10922 = CARTESIAN_POINT ( 'NONE',  ( -119.9999999999984652, 16.00000000000000000, 35.00000000000000000 ) ) ;
#10923 = CARTESIAN_POINT ( 'NONE',  ( -15.42815683172655028, -34.17926237904570996, 7.697694107796190899 ) ) ;
#10924 = ORIENTED_EDGE ( 'NONE', *, *, #23317, .F. ) ;
#10925 = EDGE_CURVE ( 'NONE', #14108, #41530, #43605, .T. ) ;
#10926 = CARTESIAN_POINT ( 'NONE',  ( 181.0000000000000000, 175.0000000000000284, -360.0000000000001705 ) ) ;
#10927 = EDGE_CURVE ( 'NONE', #50487, #40728, #14424, .T. ) ;
#10928 = CARTESIAN_POINT ( 'NONE',  ( 31.55402655318503236, -1.025126265847089879, 82.56828755692798438 ) ) ;
#10929 = CARTESIAN_POINT ( 'NONE',  ( 31.55402655318503236, 0.000000000000000000, -37.43171244307200141 ) ) ;
#10930 = ORIENTED_EDGE ( 'NONE', *, *, #50551, .F. ) ;
#10931 = EDGE_LOOP ( 'NONE', ( #49545, #30264, #10715, #5625, #16523, #7393 ) ) ;
#10932 = LINE ( 'NONE', #26591, #2501 ) ;
#10933 = CARTESIAN_POINT ( 'NONE',  ( 210.0000000000000568, 0.000000000000000000, -39.18171244307202983 ) ) ;
#10934 = CARTESIAN_POINT ( 'NONE',  ( 151.5540265531850537, -1.025126265847089657, 119.0682875569279560 ) ) ;
#10935 = ADVANCED_FACE ( 'NONE', ( #13312 ), #16174, .F. ) ;
#10936 = VERTEX_POINT ( 'NONE', #4624 ) ;
#10937 = ORIENTED_EDGE ( 'NONE', *, *, #23023, .T. ) ;
#10938 = ADVANCED_FACE ( 'NONE', ( #26124 ), #45605, .F. ) ;
#10939 = CARTESIAN_POINT ( 'NONE',  ( 14.29087950072012170, 9.652079258044652832, 8.727788335465566760 ) ) ;
#10940 = FACE_OUTER_BOUND ( 'NONE', #31001, .T. ) ;
#10941 = ADVANCED_FACE ( 'NONE', ( #45345 ), #6628, .T. ) ;
#10942 = DIRECTION ( 'NONE',  ( 0.000000000000000000, -1.000000000000000000, 1.822804496942680012E-16 ) ) ;
#10943 = CARTESIAN_POINT ( 'NONE',  ( -44.94597344681493922, 2.143131898507880377E-16, 165.0000000000000000 ) ) ;
#10944 = VECTOR ( 'NONE', #49990, 1000.000000000000000 ) ;
#10945 = CARTESIAN_POINT ( 'NONE',  ( -204.9459734468149463, 2.143131898507880377E-16, -77.43171244307204404 ) ) ;
#10946 = ORIENTED_EDGE ( 'NONE', *, *, #6036, .F. ) ;
#10948 = EDGE_CURVE ( 'NONE', #34658, #10187, #40782, .T. ) ;
#10947 = SURFACE_STYLE_USAGE ( .BOTH. , #46055 ) ;
#10949 = VECTOR ( 'NONE', #30200, 1000.000000000000000 ) ;
#10950 = CARTESIAN_POINT ( 'NONE',  ( 113.3040265531850537, -1.749999999999996891, 0.8182875569279768335 ) ) ;
#10951 = CARTESIAN_POINT ( 'NONE',  ( -14.99999999999782041, 16.00000000000000000, 115.0000000000000142 ) ) ;
#10952 = DIRECTION ( 'NONE',  ( 0.000000000000000000, -1.000000000000000000, 0.000000000000000000 ) ) ;
#10953 = VECTOR ( 'NONE', #40822, 1000.000000000000114 ) ;
#10954 = CIRCLE ( 'NONE', #39648, 3.750000000000000000 ) ;
#10955 = CARTESIAN_POINT ( 'NONE',  ( 16.73672383626881199, 2.341008440548109970, -9.008049429158102583 ) ) ;
#10956 = CARTESIAN_POINT ( 'NONE',  ( 155.0540265531850537, 2.143131898507880377E-16, -157.4317124430720582 ) ) ;
#10957 = ORIENTED_EDGE ( 'NONE', *, *, #3765, .F. ) ;
#10958 = CARTESIAN_POINT ( 'NONE',  ( 7.576114424932982594, -50.00000000000000711, 7.906207997025717304 ) ) ;
#10959 = CARTESIAN_POINT ( 'NONE',  ( -6.174150299305392053, 33.14591993373988998, 8.807470649214879543 ) ) ;
#10960 = DIRECTION ( 'NONE',  ( -0.000000000000000000, -1.000000000000000000, -0.000000000000000000 ) ) ;
#10961 = VERTEX_POINT ( 'NONE', #10231 ) ;
#10962 = CARTESIAN_POINT ( 'NONE',  ( -126.6959734468149321, 0.000000000000000000, 165.0000000000000000 ) ) ;
#10963 = VECTOR ( 'NONE', #42927, 1000.000000000000000 ) ;
#10964 = DIRECTION ( 'NONE',  ( -1.000000000000000000, 0.000000000000000000, 0.000000000000000000 ) ) ;
#10965 =( BOUNDED_CURVE ( )  B_SPLINE_CURVE ( 3, ( #46035, #22725, #29667, #26580 ),
 .UNSPECIFIED., .F., .F. ) 
 B_SPLINE_CURVE_WITH_KNOTS ( ( 4, 4 ),
 ( 4.712388980384689674, 6.283185307179586232 ),
 .UNSPECIFIED. ) 
 CURVE ( )  GEOMETRIC_REPRESENTATION_ITEM ( )  RATIONAL_B_SPLINE_CURVE ( ( 1.000000000000000000, 0.8047378541243649375, 0.8047378541243649375, 1.000000000000000000 ) ) 
 REPRESENTATION_ITEM ( '' )  );
#10966 = EDGE_LOOP ( 'NONE', ( #43301, #13050, #16203, #22838, #50684, #43431 ) ) ;
#10967 = CARTESIAN_POINT ( 'NONE',  ( -84.94597344681494633, 2.143131898507880377E-16, -77.43171244307204404 ) ) ;
#10968 = CARTESIAN_POINT ( 'NONE',  ( 0.000000000000000000, -180.9999999999999716, -358.0000000000002274 ) ) ;
#10969 = DIRECTION ( 'NONE',  ( -1.586032880504786307E-16, 1.654361225106055350E-24, -1.000000000000000000 ) ) ;
#10970 = CARTESIAN_POINT ( 'NONE',  ( 26.25702031264353664, -26.77347351953840615, 8.914903342594564961 ) ) ;
#10971 = ADVANCED_FACE ( 'NONE', ( #25380 ), #37211, .F. ) ;
#10972 = ORIENTED_EDGE ( 'NONE', *, *, #19516, .T. ) ;
#10973 =( LENGTH_UNIT ( ) NAMED_UNIT ( * ) SI_UNIT ( .MILLI., .METRE. ) );
#10974 = ORIENTED_EDGE ( 'NONE', *, *, #10709, .T. ) ;
#10975 = VERTEX_POINT ( 'NONE', #41030 ) ;
#10976 = EDGE_CURVE ( 'NONE', #17617, #15072, #20222, .T. ) ;
#10977 = DIRECTION ( 'NONE',  ( -0.000000000000000000, -0.000000000000000000, -1.000000000000000000 ) ) ;
#10978 = EDGE_LOOP ( 'NONE', ( #43092, #33177, #43985, #35389 ) ) ;
#10980 = AXIS2_PLACEMENT_3D ( 'NONE', #9973, #13310, #48172 ) ;
#10979 = DIRECTION ( 'NONE',  ( 0.000000000000000000, 0.000000000000000000, -1.000000000000000000 ) ) ;
#10981 = CARTESIAN_POINT ( 'NONE',  ( -47.88254548617756967, 14.43607691413558669, -3.760136334089591248 ) ) ;
#10982 = AXIS2_PLACEMENT_3D ( 'NONE', #19940, #12493, #20704 ) ;
#10983 = CARTESIAN_POINT ( 'NONE',  ( 14.29087950072012170, 9.652079258044652832, 8.727788335465566760 ) ) ;
#10984 = AXIS2_PLACEMENT_3D ( 'NONE', #39080, #19539, #16473 ) ;
#10985 = LINE ( 'NONE', #38213, #28435 ) ;
#10986 = VERTEX_POINT ( 'NONE', #5874 ) ;
#10987 = VECTOR ( 'NONE', #40201, 1000.000000000000000 ) ;
#10988 = CARTESIAN_POINT ( 'NONE',  ( 0.4400426740873927822, -2.015233077865103972, 9.886433018048071730 ) ) ;
#10989 = CARTESIAN_POINT ( 'NONE',  ( -87.72109971266203843, 1.750000000000009548, 81.84341382277507648 ) ) ;
#10990 = DIRECTION ( 'NONE',  ( -1.586032880504786307E-16, 1.654361225106055350E-24, -1.000000000000000000 ) ) ;
#10991 = DIRECTION ( 'NONE',  ( 0.000000000000000000, -0.000000000000000000, -1.000000000000000000 ) ) ;
#10992 = ORIENTED_EDGE ( 'NONE', *, *, #43931, .T. ) ;
#10993 = CARTESIAN_POINT ( 'NONE',  ( -6.695973446814940111, -1.750000000000024203, 80.81828755692798438 ) ) ;
#10994 = DIRECTION ( 'NONE',  ( 0.000000000000000000, 0.000000000000000000, 1.000000000000000000 ) ) ;
#10995 = EDGE_LOOP ( 'NONE', ( #43594, #20599, #24573, #46147, #36648, #42124 ) ) ;
#10996 = EDGE_LOOP ( 'NONE', ( #26411, #42940, #12290, #33205 ) ) ;
#10997 = ORIENTED_EDGE ( 'NONE', *, *, #12488, .T. ) ;
#10998 = CARTESIAN_POINT ( 'NONE',  ( 1.011271242968694084, -0.7347315653655782652, -10.00000000000000000 ) ) ;
#10999 = DIRECTION ( 'NONE',  ( 1.000000000000000000, 0.000000000000000000, 0.000000000000000000 ) ) ;
#11000 = B_SPLINE_SURFACE_WITH_KNOTS ( 'NONE', 3, 3, ( 
 ( #7058, #27579, #8079, #2929 ),
 ( #26550, #11663, #49833, #18581 ),
 ( #19089, #50092, #31173, #7826 ),
 ( #27315, #15757, #15006, #43214 ) ),
 .UNSPECIFIED., .F., .F., .F.,
 ( 4, 4 ),
 ( 4, 4 ),
 ( 0.000000000000000000, 1.000000000000000000 ),
 ( 0.000000000000000000, 1.000000000000000000 ),
 .UNSPECIFIED. ) ;
#11001 = ORIENTED_EDGE ( 'NONE', *, *, #933, .F. ) ;
#11002 = DIRECTION ( 'NONE',  ( 0.000000000000000000, 1.000000000000000000, 0.000000000000000000 ) ) ;
#11003 = CARTESIAN_POINT ( 'NONE',  ( 224.9999999999999716, 175.0000000000000284, 499.9999999999998863 ) ) ;
#11004 = CARTESIAN_POINT ( 'NONE',  ( 7.216980890441427654, -6.922079660550236824, 0.000000000000000000 ) ) ;
#11005 = VECTOR ( 'NONE', #11214, 1000.000000000000114 ) ;
#11006 = CARTESIAN_POINT ( 'NONE',  ( 1.250000000000000222, 0.000000000000000000, 10.00000000000000000 ) ) ;
#11007 = CARTESIAN_POINT ( 'NONE',  ( -88.44597344681494633, -1.025126265847089879, 82.56828755692798438 ) ) ;
#11008 = CARTESIAN_POINT ( 'NONE',  ( 9.999626982420835475, 0.09954095390207136351, 8.968381510274435087 ) ) ;
#11010 = ADVANCED_FACE ( 'NONE', ( #13807 ), #49179, .F. ) ;
#11009 = CARTESIAN_POINT ( 'NONE',  ( 7.398363427652525637, -15.19415887381133246, -9.008049429158100807 ) ) ;
#11011 = CARTESIAN_POINT ( 'NONE',  ( 35.00000000000061107, 16.00000000000000000, -54.99999999999999289 ) ) ;
#11012 = ORIENTED_EDGE ( 'NONE', *, *, #41707, .T. ) ;
#11013 = DIRECTION ( 'NONE',  ( 0.000000000000000000, -0.2981428420003837121, -0.9545212652235329776 ) ) ;
#11014 = DIRECTION ( 'NONE',  ( -0.000000000000000000, -1.000000000000000000, -0.000000000000000000 ) ) ;
#11015 = AXIS2_PLACEMENT_3D ( 'NONE', #49056, #10605, #26269 ) ;
#11016 = DIRECTION ( 'NONE',  ( -0.000000000000000000, -1.000000000000000000, -0.000000000000000000 ) ) ;
#11017 = DIRECTION ( 'NONE',  ( 0.000000000000000000, -1.000000000000000000, 0.000000000000000000 ) ) ;
#11018 = ORIENTED_EDGE ( 'NONE', *, *, #15933, .F. ) ;
#11019 = LINE ( 'NONE', #15386, #23888 ) ;
#11020 = AXIS2_PLACEMENT_3D ( 'NONE', #21257, #36946, #1763 ) ;
#11021 = LINE ( 'NONE', #15387, #798 ) ;
#11022 = CARTESIAN_POINT ( 'NONE',  ( -29.61572577327014955, -16.11461842845715253, 8.807470649214879543 ) ) ;
#11023 = CARTESIAN_POINT ( 'NONE',  ( 0.8285222815141930486, 1.889008401827334094, 9.886433018048068178 ) ) ;
#11025 = B_SPLINE_CURVE_WITH_KNOTS ( 'NONE', 3,
 ( #23797, #43530, #28151, #8892 ),
 .UNSPECIFIED., .F., .F.,
 ( 4, 4 ),
 ( 0.9895749839358304323, 1.000000000000000000 ),
 .UNSPECIFIED. ) ;
#11024 = AXIS2_PLACEMENT_3D ( 'NONE', #1465, #9901, #48352 ) ;
#11026 = DIRECTION ( 'NONE',  ( 0.000000000000000000, 0.000000000000000000, 1.000000000000000000 ) ) ;
#11027 =( BOUNDED_CURVE ( )  B_SPLINE_CURVE ( 3, ( #38455, #33261, #15443, #40943 ),
 .UNSPECIFIED., .F., .F. ) 
 B_SPLINE_CURVE_WITH_KNOTS ( ( 4, 4 ),
 ( 1.570796326794896558, 3.141592653589793116 ),
 .UNSPECIFIED. ) 
 CURVE ( )  GEOMETRIC_REPRESENTATION_ITEM ( )  RATIONAL_B_SPLINE_CURVE ( ( 1.000000000000000000, 0.8047378541243649375, 0.8047378541243649375, 1.000000000000000000 ) ) 
 REPRESENTATION_ITEM ( '' )  );
#11028 = EDGE_LOOP ( 'NONE', ( #25500, #21412, #23274, #13786, #15362, #15842 ) ) ;
#11029 = CARTESIAN_POINT ( 'NONE',  ( -6.619412807845042046, 7.495556955913086128, 9.646707543097347681 ) ) ;
#11030 = ORIENTED_EDGE ( 'NONE', *, *, #1749, .T. ) ;
#11031 = DIRECTION ( 'NONE',  ( 0.000000000000000000, 1.000000000000000000, 0.000000000000000000 ) ) ;
#11032 = VERTEX_POINT ( 'NONE', #26383 ) ;
#11033 = CARTESIAN_POINT ( 'NONE',  ( 135.0000000000006253, 16.00000000000000000, -54.99999999999999289 ) ) ;
#11034 = CARTESIAN_POINT ( 'NONE',  ( 73.30402655318508209, -1.750000000000010214, -39.18171244307202983 ) ) ;
#11035 =( BOUNDED_CURVE ( )  B_SPLINE_CURVE ( 3, ( #4422, #16226, #47483, #15455 ),
 .UNSPECIFIED., .F., .F. ) 
 B_SPLINE_CURVE_WITH_KNOTS ( ( 4, 4 ),
 ( 3.141592653590070672, 4.712388980384703885 ),
 .UNSPECIFIED. ) 
 CURVE ( )  GEOMETRIC_REPRESENTATION_ITEM ( )  RATIONAL_B_SPLINE_CURVE ( ( 1.000000000000000000, 0.8047378541244271100, 0.8047378541244271100, 1.000000000000000000 ) ) 
 REPRESENTATION_ITEM ( '' )  );
#11036 = ORIENTED_EDGE ( 'NONE', *, *, #26643, .T. ) ;
#11037 = DIRECTION ( 'NONE',  ( -1.000000000000000000, -0.000000000000000000, -0.000000000000000000 ) ) ;
#11038 = ORIENTED_EDGE ( 'NONE', *, *, #30205, .F. ) ;
#11039 = VECTOR ( 'NONE', #7555, 1000.000000000000000 ) ;
#11040 = VERTEX_POINT ( 'NONE', #25635 ) ;
#11041 = CARTESIAN_POINT ( 'NONE',  ( 75.05402655318509630, 1.025126265847089879, -77.43171244307200141 ) ) ;
#11042 = DIRECTION ( 'NONE',  ( 0.000000000000000000, 2.537652627714642000E-15, 1.000000000000000000 ) ) ;
#11043 = CIRCLE ( 'NONE', #49525, 1.750000000000001554 ) ;
#11044 = VERTEX_POINT ( 'NONE', #48922 ) ;
#11045 = CARTESIAN_POINT ( 'NONE',  ( -8.001683061421429599, -5.997755262142646870, 9.282506307616484875 ) ) ;
#11046 = LINE ( 'NONE', #11303, #20158 ) ;
#11047 = DIRECTION ( 'NONE',  ( -1.000000000000000000, 0.000000000000000000, 0.000000000000000000 ) ) ;
#11048 = ORIENTED_EDGE ( 'NONE', *, *, #16222, .F. ) ;
#11049 = ORIENTED_EDGE ( 'NONE', *, *, #19864, .T. ) ;
#11050 = LINE ( 'NONE', #31587, #5416 ) ;
#11051 = CARTESIAN_POINT ( 'NONE',  ( 151.5540265531850537, 1.025126265847088991, 2.568287556927986159 ) ) ;
#11052 = VERTEX_POINT ( 'NONE', #44845 ) ;
#11053 = LINE ( 'NONE', #34420, #25112 ) ;
#11054 = VECTOR ( 'NONE', #25827, 1000.000000000000000 ) ;
#11055 = CARTESIAN_POINT ( 'NONE',  ( 115.0540265531850395, 2.143131898507847836E-16, 159.0682875569279702 ) ) ;
#11056 = ORIENTED_EDGE ( 'NONE', *, *, #22216, .T. ) ;
#11057 = CARTESIAN_POINT ( 'NONE',  ( -1.025617443042918353, -1.003000432359008487, 9.950105812514305370 ) ) ;
#11058 = DIRECTION ( 'NONE',  ( -0.000000000000000000, -1.000000000000000000, -0.000000000000000000 ) ) ;
#11059 = EDGE_LOOP ( 'NONE', ( #37773, #41139, #44429, #7001, #34543, #28666 ) ) ;
#11060 = PLANE ( 'NONE',  #515 ) ;
#11061 = CARTESIAN_POINT ( 'NONE',  ( 155.0540265531850537, 1.025126265847089879, -117.4317124430720156 ) ) ;
#11062 = DIRECTION ( 'NONE',  ( -1.000000000000000000, 0.000000000000000000, 0.000000000000000000 ) ) ;
#11063 = CARTESIAN_POINT ( 'NONE',  ( 0.6538612634419860292, 1.160398818844859958, 9.951893257059996500 ) ) ;
#11064 = ORIENTED_EDGE ( 'NONE', *, *, #45295, .T. ) ;
#11065 = CARTESIAN_POINT ( 'NONE',  ( 85.00000000000056843, 16.00000000000000000, -54.99999999999999289 ) ) ;
#11067 = EDGE_CURVE ( 'NONE', #17053, #50485, #30896, .T. ) ;
#11066 = CARTESIAN_POINT ( 'NONE',  ( 358.0000000000000000, -169.0000000000001137, -344.0000000000002842 ) ) ;
#11068 = LINE ( 'NONE', #42362, #33818 ) ;
#11069 = ORIENTED_EDGE ( 'NONE', *, *, #5194, .F. ) ;
#11070 = EDGE_CURVE ( 'NONE', #18711, #4028, #26780, .T. ) ;
#11071 = EDGE_LOOP ( 'NONE', ( #13031, #28160, #2124, #24857, #5737, #16254 ) ) ;
#11072 = DIRECTION ( 'NONE',  ( -0.7524306361317540937, 0.6539796711687702047, 0.07847756054026462647 ) ) ;
#11073 = ADVANCED_FACE ( 'NONE', ( #22282 ), #45097, .F. ) ;
#11074 = CARTESIAN_POINT ( 'NONE',  ( 9.185112145816566098, 4.082484168683570285E-15, -33.33601305720110020 ) ) ;
#11075 = CARTESIAN_POINT ( 'NONE',  ( -1.697332391510605554, -0.8495613812372067031, 9.900811091504550632 ) ) ;
#11076 = LINE ( 'NONE', #46185, #40616 ) ;
#11077 = VECTOR ( 'NONE', #7901, 1000.000000000000000 ) ;
#11078 = CARTESIAN_POINT ( 'NONE',  ( 130.0000000000005684, 16.00000000000000000, -54.99999999999999289 ) ) ;
#11079 = CARTESIAN_POINT ( 'NONE',  ( -8.445973446814976526, 0.000000000000000000, 165.0000000000000000 ) ) ;
#11080 = VECTOR ( 'NONE', #25108, 1000.000000000000000 ) ;
#11081 = DIRECTION ( 'NONE',  ( 1.000000000000000000, 0.000000000000000000, 0.000000000000000000 ) ) ;
#11082 = EDGE_LOOP ( 'NONE', ( #6284, #44033, #17687, #3361 ) ) ;
#11083 = CARTESIAN_POINT ( 'NONE',  ( 15.98719783915691650, -4.501063718205879916, 3.266473740018926541 ) ) ;
#11084 = EDGE_CURVE ( 'NONE', #20395, #20947, #15381, .T. ) ;
#11085 = EDGE_CURVE ( 'NONE', #36453, #18948, #30232, .T. ) ;
#11086 = CARTESIAN_POINT ( 'NONE',  ( -33.01266944765060174, 5.813986777101691317, 1.847720168420772691 ) ) ;
#11087 = DIRECTION ( 'NONE',  ( -1.000000000000000000, -8.881784197001252323E-16, 0.000000000000000000 ) ) ;
#11088 = EDGE_CURVE ( 'NONE', #40814, #2042, #1302, .T. ) ;
#11089=STYLED_ITEM('',(#50747),#22493);
#11090 = ORIENTED_EDGE ( 'NONE', *, *, #9820, .T. ) ;
#11091 =( GEOMETRIC_REPRESENTATION_CONTEXT ( 3 ) GLOBAL_UNCERTAINTY_ASSIGNED_CONTEXT ( ( #42900 ) ) GLOBAL_UNIT_ASSIGNED_CONTEXT ( ( #50597, #27566, #39371 ) ) REPRESENTATION_CONTEXT ( 'NONE', 'WORKASPACE' ) );
#11092 = VECTOR ( 'NONE', #11511, 1000.000000000000000 ) ;
#11093 = CARTESIAN_POINT ( 'NONE',  ( -1.011271242968688533, 0.7347315653655859258, 3.333333333333333481 ) ) ;
#11094 = VERTEX_POINT ( 'NONE', #18167 ) ;
#11095 = LINE ( 'NONE', #41889, #39375 ) ;
#11096 = CARTESIAN_POINT ( 'NONE',  ( 339.9999999999999432, -168.9999999999999432, -358.0000000000002274 ) ) ;
#11097 = EDGE_CURVE ( 'NONE', #41339, #10712, #14577, .T. ) ;
#11098 = CARTESIAN_POINT ( 'NONE',  ( 115.0540265531850395, 1.025126265847081442, -0.9317124430720195027 ) ) ;
#11099 = EDGE_CURVE ( 'NONE', #47768, #16759, #46825, .T. ) ;
#11100 = AXIS2_PLACEMENT_3D ( 'NONE', #241, #43314, #23577 ) ;
#11101 = EDGE_LOOP ( 'NONE', ( #45921, #36318 ) ) ;
#11102 = EDGE_CURVE ( 'NONE', #8469, #32098, #14323, .T. ) ;
#11103 = EDGE_CURVE ( 'NONE', #20217, #17284, #50702, .T. ) ;
#11104 = CARTESIAN_POINT ( 'NONE',  ( -164.9459734468149463, -1.025126265847089657, -80.93171244307201562 ) ) ;
#11105 = CARTESIAN_POINT ( 'NONE',  ( -125.6708471809678542, 1.749999999999996225, 161.8434138227750907 ) ) ;
#11106 = VERTEX_POINT ( 'NONE', #12007 ) ;
#11107 = CARTESIAN_POINT ( 'NONE',  ( 6.619412807845094449, -7.495556955913033725, 9.646707543097347681 ) ) ;
#11108 = FACE_OUTER_BOUND ( 'NONE', #3778, .T. ) ;
#11109 = EDGE_CURVE ( 'NONE', #9910, #8725, #14831, .T. ) ;
#11110 = DIRECTION ( 'NONE',  ( 0.6805276818820362728, 0.4944323023722117516, -0.5407575913134976542 ) ) ;
#11111 = EDGE_CURVE ( 'NONE', #48546, #1481, #43289, .T. ) ;
#11112 = ORIENTED_EDGE ( 'NONE', *, *, #35984, .F. ) ;
#11113 = ORIENTED_EDGE ( 'NONE', *, *, #8769, .T. ) ;
#11114 = LINE ( 'NONE', #49551, #8702 ) ;
#11115 = VECTOR ( 'NONE', #7257, 1000.000000000000000 ) ;
#11116 = ORIENTED_EDGE ( 'NONE', *, *, #12043, .T. ) ;
#11117 = ORIENTED_EDGE ( 'NONE', *, *, #24960, .T. ) ;
#11118 = CARTESIAN_POINT ( 'NONE',  ( 75.05402655318509630, 2.143131898507880377E-16, -0.9317124430720524764 ) ) ;
#11119 = CARTESIAN_POINT ( 'NONE',  ( 191.5540265531851105, 0.000000000000000000, 39.06828755692798438 ) ) ;
#11120 = CARTESIAN_POINT ( 'NONE',  ( 4.999999999999999112, 175.0000000000000284, -350.0000000000002274 ) ) ;
#11121 = AXIS2_PLACEMENT_3D ( 'NONE', #30377, #27025, #6766 ) ;
#11122 = ORIENTED_EDGE ( 'NONE', *, *, #6120, .F. ) ;
#11123 = DIRECTION ( 'NONE',  ( -0.000000000000000000, -1.000000000000000000, -0.000000000000000000 ) ) ;
#11124 = VERTEX_POINT ( 'NONE', #3793 ) ;
#11125 = VECTOR ( 'NONE', #13095, 1000.000000000000000 ) ;
#11126 = CARTESIAN_POINT ( 'NONE',  ( 166.9999999999999716, -256.4999999999999432, -349.9999999999999432 ) ) ;
#11127 = ADVANCED_FACE ( 'NONE', ( #30485 ), #18670, .F. ) ;
#11128 = DIRECTION ( 'NONE',  ( -0.000000000000000000, -1.000000000000000000, -0.000000000000000000 ) ) ;
#11130 = AXIS2_PLACEMENT_3D ( 'NONE', #39726, #7654, #3527 ) ;
#11129 = LINE ( 'NONE', #6767, #36210 ) ;
#11131 = EDGE_CURVE ( 'NONE', #9299, #25919, #8162, .T. ) ;
#11132 = VERTEX_POINT ( 'NONE', #27148 ) ;
#11133 = EDGE_CURVE ( 'NONE', #27742, #49858, #10985, .T. ) ;
#11134 = VERTEX_POINT ( 'NONE', #39213 ) ;
#11135 = PRESENTATION_LAYER_ASSIGNMENT (  '', '', ( #2942 ) ) ;
#11136 = ORIENTED_EDGE ( 'NONE', *, *, #32928, .F. ) ;
#11138 = EDGE_CURVE ( 'NONE', #47505, #17018, #26638, .T. ) ;
#11137 = SURFACE_STYLE_FILL_AREA ( #6772 ) ;
#11139 = CARTESIAN_POINT ( 'NONE',  ( -168.4459734468149747, 1.025126265847089657, -120.9317124430720440 ) ) ;
#11140 = VERTEX_POINT ( 'NONE', #42775 ) ;
#11141 = CARTESIAN_POINT ( 'NONE',  ( 34.32915281903212446, 1.750000000000010214, 121.8434138227750623 ) ) ;
#11142 = EDGE_LOOP ( 'NONE', ( #41161, #38667, #41903, #7324, #21124 ) ) ;
#11143 = AXIS2_PLACEMENT_3D ( 'NONE', #31989, #47831, #47584 ) ;
#11144 = EDGE_CURVE ( 'NONE', #24745, #48433, #34346, .T. ) ;
#11145 = VECTOR ( 'NONE', #21959, 1000.000000000000000 ) ;
#11146 = CARTESIAN_POINT ( 'NONE',  ( 194.9999999999999432, 173.0000000000000000, 231.9999999999999716 ) ) ;
#11147 = ORIENTED_EDGE ( 'NONE', *, *, #22363, .T. ) ;
#11148 = CARTESIAN_POINT ( 'NONE',  ( -25.04522487443065160, 22.77512090857326754, 8.356839323120299312 ) ) ;
#11149 = DIRECTION ( 'NONE',  ( 0.000000000000000000, -0.000000000000000000, 1.000000000000000000 ) ) ;
#11150 = CARTESIAN_POINT ( 'NONE',  ( 6.508636631827673824, 15.75743548351451295, 8.953103998512858652 ) ) ;
#11151 = DIRECTION ( 'NONE',  ( -0.000000000000000000, -0.000000000000000000, -1.000000000000000000 ) ) ;
#11152 = CARTESIAN_POINT ( 'NONE',  ( 31.55402655318503236, 0.000000000000000000, 122.5682875569279702 ) ) ;
#11153 = ORIENTED_EDGE ( 'NONE', *, *, #50000, .T. ) ;
#11154 = DIRECTION ( 'NONE',  ( 0.000000000000000000, 0.9749645535258955054, -0.2223603367690637767 ) ) ;
#11155 = DIRECTION ( 'NONE',  ( 0.000000000000000000, 0.000000000000000000, 1.000000000000000000 ) ) ;
#11156 = LINE ( 'NONE', #27051, #8914 ) ;
#11157 = CARTESIAN_POINT ( 'NONE',  ( -16.52264463346130796, 2.779753662172870232, 9.403735324607438884 ) ) ;
#11158 = EDGE_CURVE ( 'NONE', #26037, #26846, #7710, .T. ) ;
#11159 = VECTOR ( 'NONE', #9215, 1000.000000000000000 ) ;
#11160 = CARTESIAN_POINT ( 'NONE',  ( 35.00000000000091660, 17.00000000000000000, 0.000000000000000000 ) ) ;
#11161 = AXIS2_PLACEMENT_3D ( 'NONE', #1848, #21336, #10045 ) ;
#11162 = EDGE_CURVE ( 'NONE', #36434, #16542, #37457, .T. ) ;
#11163 = VECTOR ( 'NONE', #15992, 1000.000000000000000 ) ;
#11164 = FACE_OUTER_BOUND ( 'NONE', #10725, .T. ) ;
#11165 = VERTEX_POINT ( 'NONE', #31518 ) ;
#11166 = CARTESIAN_POINT ( 'NONE',  ( -88.44597344681497475, 0.000000000000000000, -117.4317124430720156 ) ) ;
#11167 = DIRECTION ( 'NONE',  ( -1.000000000000000000, 0.000000000000000000, 0.000000000000000000 ) ) ;
#11168 = ORIENTED_EDGE ( 'NONE', *, *, #38287, .F. ) ;
#11169 = VECTOR ( 'NONE', #18997, 1000.000000000000000 ) ;
#11170 = EDGE_CURVE ( 'NONE', #42215, #38406, #8349, .T. ) ;
#11171 = EDGE_CURVE ( 'NONE', #6144, #35686, #28120, .T. ) ;
#11172 = CARTESIAN_POINT ( 'NONE',  ( 113.3040265531850537, 1.749999999999996891, -159.1817124430720298 ) ) ;
#11173 = VECTOR ( 'NONE', #37234, 1000.000000000000000 ) ;
#11174 = CARTESIAN_POINT ( 'NONE',  ( 0.3443084382174765312, 1.609917862996832705, 9.927568724237749720 ) ) ;
#11175 = ADVANCED_FACE ( 'NONE', ( #30750 ), #46358, .F. ) ;
#11176 = CARTESIAN_POINT ( 'NONE',  ( 130.0000000000008811, 16.00000000000000000, -24.99999999999999289 ) ) ;
#11177 = EDGE_CURVE ( 'NONE', #21648, #45351, #50445, .T. ) ;
#11178 = VERTEX_POINT ( 'NONE', #19176 ) ;
#11179 = ORIENTED_EDGE ( 'NONE', *, *, #39039, .F. ) ;
#11180 = CARTESIAN_POINT ( 'NONE',  ( 360.0000000000001137, 169.0000000000000000, 343.9999999999998295 ) ) ;
#11181 = AXIS2_PLACEMENT_3D ( 'NONE', #44655, #32643, #44411 ) ;
#11182 = EDGE_CURVE ( 'NONE', #25320, #16028, #31262, .T. ) ;
#11183 = DIRECTION ( 'NONE',  ( 0.000000000000000000, 0.000000000000000000, -1.000000000000000000 ) ) ;
#11184 =( BOUNDED_CURVE ( )  B_SPLINE_CURVE ( 3, ( #29102, #45716, #49552, #5992 ),
 .UNSPECIFIED., .F., .F. ) 
 B_SPLINE_CURVE_WITH_KNOTS ( ( 4, 4 ),
 ( 1.570796326794896558, 3.141592653589793116 ),
 .UNSPECIFIED. ) 
 CURVE ( )  GEOMETRIC_REPRESENTATION_ITEM ( )  RATIONAL_B_SPLINE_CURVE ( ( 1.000000000000000000, 0.8047378541243649375, 0.8047378541243649375, 1.000000000000000000 ) ) 
 REPRESENTATION_ITEM ( '' )  );
#11185 = ORIENTED_EDGE ( 'NONE', *, *, #3918, .T. ) ;
#11186 = ORIENTED_EDGE ( 'NONE', *, *, #4728, .F. ) ;
#11187 = LINE ( 'NONE', #42217, #14097 ) ;
#11188 = CARTESIAN_POINT ( 'NONE',  ( 210.0000000000000568, 0.000000000000000000, 160.8182875569279702 ) ) ;
#11189 = LINE ( 'NONE', #7328, #15267 ) ;
#11190 = VERTEX_POINT ( 'NONE', #48112 ) ;
#11191 = ORIENTED_EDGE ( 'NONE', *, *, #34594, .F. ) ;
#11192 = VERTEX_POINT ( 'NONE', #48366 ) ;
#11193 = CARTESIAN_POINT ( 'NONE',  ( 0.000000000000000000, -180.9999999999999716, -342.0000000000001705 ) ) ;
#11194 = DIRECTION ( 'NONE',  ( 0.000000000000000000, 0.000000000000000000, -1.000000000000000000 ) ) ;
#11195 = VERTEX_POINT ( 'NONE', #12756 ) ;
#11196 = DIRECTION ( 'NONE',  ( -1.000000000000000000, -0.000000000000000000, -0.000000000000000000 ) ) ;
#11197 = AXIS2_PLACEMENT_3D ( 'NONE', #39981, #23816, #36132 ) ;
#11198 = EDGE_CURVE ( 'NONE', #17256, #5743, #31428, .T. ) ;
#11199 = DIRECTION ( 'NONE',  ( 0.000000000000000000, 0.000000000000000000, 1.000000000000000000 ) ) ;
#11200 = LINE ( 'NONE', #34289, #7348 ) ;
#11201 = ORIENTED_EDGE ( 'NONE', *, *, #49342, .T. ) ;
#11202 = COLOUR_RGB ( '',0.7921568627450980005, 0.8196078431372548767, 0.9333333333333333481 ) ;
#11203 = EDGE_LOOP ( 'NONE', ( #20133, #11503, #38606, #31756, #11153, #29546, #36713, #32702 ) ) ;
#11204 = CARTESIAN_POINT ( 'NONE',  ( 0.000000000000000000, 167.0000000000000000, 355.9999999999997726 ) ) ;
#11205 = CARTESIAN_POINT ( 'NONE',  ( -208.4459734468148611, 1.025126265847088991, 162.5682875569279133 ) ) ;
#11206 =( BOUNDED_CURVE ( )  B_SPLINE_CURVE ( 3, ( #43312, #11775, #15375, #8183 ),
 .UNSPECIFIED., .F., .F. ) 
 B_SPLINE_CURVE_WITH_KNOTS ( ( 4, 4 ),
 ( 4.712388980384689674, 6.283185307179586232 ),
 .UNSPECIFIED. ) 
 CURVE ( )  GEOMETRIC_REPRESENTATION_ITEM ( )  RATIONAL_B_SPLINE_CURVE ( ( 1.000000000000000000, 0.8047378541243649375, 0.8047378541243649375, 1.000000000000000000 ) ) 
 REPRESENTATION_ITEM ( '' )  );
#11207 = CARTESIAN_POINT ( 'NONE',  ( 3.888415560953717431, 9.227494953140064737, 3.092310436554745134 ) ) ;
#11208 = ORIENTED_EDGE ( 'NONE', *, *, #39641, .T. ) ;
#11209 = ORIENTED_EDGE ( 'NONE', *, *, #34056, .F. ) ;
#11210 = CARTESIAN_POINT ( 'NONE',  ( 14.86945752723346637, 7.944783388879009145, 2.590526750877053086 ) ) ;
#11211 = CARTESIAN_POINT ( 'NONE',  ( 0.000000000000000000, 0.000000000000000000, 900.0000000000000000 ) ) ;
#11212 = CARTESIAN_POINT ( 'NONE',  ( 193.3040265531851105, 0.000000000000000000, 165.0000000000000000 ) ) ;
#11213 = LINE ( 'NONE', #22492, #12998 ) ;
#11214 = DIRECTION ( 'NONE',  ( -0.8411784753765542133, -0.000000000000000000, -0.5407575913134976542 ) ) ;
#11215 = VERTEX_POINT ( 'NONE', #20445 ) ;
#11216 = LINE ( 'NONE', #14538, #27591 ) ;
#11217 = EDGE_CURVE ( 'NONE', #19049, #22510, #1476, .T. ) ;
#11218 = DIRECTION ( 'NONE',  ( -0.000000000000000000, -0.000000000000000000, -1.000000000000000000 ) ) ;
#11219 = DIRECTION ( 'NONE',  ( -1.000000000000000000, 0.000000000000000000, 0.000000000000000000 ) ) ;
#11220 = CARTESIAN_POINT ( 'NONE',  ( 0.7849184246612691540, -1.242376769536456704, 9.958264684458541183 ) ) ;
#11221 = AXIS2_PLACEMENT_3D ( 'NONE', #32272, #35628, #466 ) ;
#11222 = DIRECTION ( 'NONE',  ( -0.000000000000000000, -0.000000000000000000, -1.000000000000000000 ) ) ;
#11223 = CARTESIAN_POINT ( 'NONE',  ( -2.637606039711253736, -0.1407378881970645645, 9.847478953136990398 ) ) ;
#11224 = ORIENTED_EDGE ( 'NONE', *, *, #25597, .F. ) ;
#11225 = CARTESIAN_POINT ( 'NONE',  ( -225.0000000000000568, 164.9999999999999716, 252.0000000000000000 ) ) ;
#11226 = CARTESIAN_POINT ( 'NONE',  ( 31.55402655318503236, -1.025126265847089657, 79.06828755692797017 ) ) ;
#11227 = ORIENTED_EDGE ( 'NONE', *, *, #3396, .F. ) ;
#11228 = CARTESIAN_POINT ( 'NONE',  ( 344.0000000000000000, 167.0000000000001990, -342.0000000000002842 ) ) ;
#11229 = ADVANCED_FACE ( 'NONE', ( #36651 ), #20207, .T. ) ;
#11230 = EDGE_CURVE ( 'NONE', #18563, #28991, #19942, .T. ) ;
#11231 = VECTOR ( 'NONE', #46299, 1000.000000000000000 ) ;
#11232 = DIRECTION ( 'NONE',  ( -1.000000000000000000, 0.000000000000000000, -1.612977847700450206E-50 ) ) ;
#11233 = ORIENTED_EDGE ( 'NONE', *, *, #47464, .T. ) ;
#11234 = LINE ( 'NONE', #14815, #23082 ) ;
#11235 = CARTESIAN_POINT ( 'NONE',  ( -124.9459734468149463, 2.143131898507847836E-16, 122.5682875569279560 ) ) ;
#11236 = DIRECTION ( 'NONE',  ( 1.000000000000000000, 0.000000000000000000, -4.758098676964956461E-16 ) ) ;
#11237 = CARTESIAN_POINT ( 'NONE',  ( 194.9999999999999432, 173.0000000000000000, 112.0000000000000000 ) ) ;
#11238 = EDGE_CURVE ( 'NONE', #14892, #4637, #23808, .T. ) ;
#11239 = ORIENTED_EDGE ( 'NONE', *, *, #9359, .T. ) ;
#11240 = CARTESIAN_POINT ( 'NONE',  ( -10.69268279052439574, -12.77266927778454964, -2.870787844569587133 ) ) ;
#11241 = ORIENTED_EDGE ( 'NONE', *, *, #24293, .F. ) ;
#11242 = ORIENTED_EDGE ( 'NONE', *, *, #26808, .T. ) ;
#11243 = EDGE_CURVE ( 'NONE', #30326, #9775, #18139, .T. ) ;
#11244 = LINE ( 'NONE', #26631, #30378 ) ;
#11245 = EDGE_CURVE ( 'NONE', #28209, #17293, #37703, .T. ) ;
#11246 = ORIENTED_EDGE ( 'NONE', *, *, #1060, .T. ) ;
#11247 = CYLINDRICAL_SURFACE ( 'NONE', #3288, 1.750000000000001554 ) ;
#11248 = CARTESIAN_POINT ( 'NONE',  ( 210.0000000000000568, 2.143131898507890731E-16, 159.0682875569279702 ) ) ;
#11249 = DIRECTION ( 'NONE',  ( 0.000000000000000000, -0.000000000000000000, 1.000000000000000000 ) ) ;
#11250 = EDGE_CURVE ( 'NONE', #40512, #18367, #43546, .T. ) ;
#11251 = DIRECTION ( 'NONE',  ( 0.000000000000000000, 0.9230769230769231282, 0.3846153846153844702 ) ) ;
#11252 = EDGE_LOOP ( 'NONE', ( #4720, #30211, #30486, #9451 ) ) ;
#11253 = CARTESIAN_POINT ( 'NONE',  ( 135.0000000000021600, 17.00000000000000000, 115.0000000000000142 ) ) ;
#11254 = CARTESIAN_POINT ( 'NONE',  ( 349.9999999999999432, -180.9999999999999716, 357.9999999999997726 ) ) ;
#11255 = ORIENTED_EDGE ( 'NONE', *, *, #30061, .T. ) ;
#11256 = PLANE ( 'NONE',  #17746 ) ;
#11257 = DIRECTION ( 'NONE',  ( 1.000000000000000000, -0.000000000000000000, -0.000000000000000000 ) ) ;
#11258 = ORIENTED_EDGE ( 'NONE', *, *, #25879, .T. ) ;
#11259 = EDGE_LOOP ( 'NONE', ( #18527, #35353, #15772, #36057 ) ) ;
#11260 = ORIENTED_EDGE ( 'NONE', *, *, #44982, .T. ) ;
#11261 = DIRECTION ( 'NONE',  ( -1.000000000000000000, 0.000000000000000000, 4.625929269271542120E-16 ) ) ;
#11262 = DIRECTION ( 'NONE',  ( -0.000000000000000000, -1.000000000000000000, -0.000000000000000000 ) ) ;
#11263 = ORIENTED_EDGE ( 'NONE', *, *, #15820, .F. ) ;
#11264 = CARTESIAN_POINT ( 'NONE',  ( -1.249999999999999778, 0.000000000000000000, -3.333333333333333481 ) ) ;
#11265 = LINE ( 'NONE', #30769, #37062 ) ;
#11266 = DIRECTION ( 'NONE',  ( 0.000000000000000000, 5.664403186863042467E-17, 1.000000000000000000 ) ) ;
#11267 = CARTESIAN_POINT ( 'NONE',  ( -128.4459734468149463, 1.025126265847081886, 119.0682875569279702 ) ) ;
#11268 = VECTOR ( 'NONE', #32064, 1000.000000000000000 ) ;
#11269 = PLANE ( 'NONE',  #47894 ) ;
#11270 = DIRECTION ( 'NONE',  ( -1.000000000000000000, 0.000000000000000000, 1.860490536778032451E-50 ) ) ;
#11271 = FILL_AREA_STYLE_COLOUR ( '', #43144 ) ;
#11272 = PLANE ( 'NONE',  #11100 ) ;
#11273 = CARTESIAN_POINT ( 'NONE',  ( 1.104213410210670876, 0.6509177773818231039, 9.976582533991679824 ) ) ;
#11274 = EDGE_CURVE ( 'NONE', #30452, #24759, #35876, .T. ) ;
#11275 = ORIENTED_EDGE ( 'NONE', *, *, #37546, .T. ) ;
#11276 = DIRECTION ( 'NONE',  ( 0.000000000000000000, 0.000000000000000000, 1.000000000000000000 ) ) ;
#11277 = CARTESIAN_POINT ( 'NONE',  ( 181.0000000000000000, -270.4999999999999432, -349.9999999999999432 ) ) ;
#11278 =( BOUNDED_CURVE ( )  B_SPLINE_CURVE ( 3, ( #6313, #41708, #21955, #2696 ),
 .UNSPECIFIED., .F., .F. ) 
 B_SPLINE_CURVE_WITH_KNOTS ( ( 4, 4 ),
 ( 3.141592653589793116, 4.712388980384689674 ),
 .UNSPECIFIED. ) 
 CURVE ( )  GEOMETRIC_REPRESENTATION_ITEM ( )  RATIONAL_B_SPLINE_CURVE ( ( 1.000000000000000000, 0.8047378541243649375, 0.8047378541243649375, 1.000000000000000000 ) ) 
 REPRESENTATION_ITEM ( '' )  );
#11279 = LINE ( 'NONE', #45877, #29816 ) ;
#11280 = DIRECTION ( 'NONE',  ( 3.172065745548403743E-16, 1.000000000000000000, 0.000000000000000000 ) ) ;
#11281 = ORIENTED_EDGE ( 'NONE', *, *, #42546, .F. ) ;
#11282 = FACE_OUTER_BOUND ( 'NONE', #29594, .T. ) ;
#11283 = CARTESIAN_POINT ( 'NONE',  ( 46.11867747200574286, -19.86470446310233129, -8.016098858316205167 ) ) ;
#11284 = CARTESIAN_POINT ( 'NONE',  ( 17.23491422248386584, -0.5912720620000816441, 8.727788335465566760 ) ) ;
#11285 = CARTESIAN_POINT ( 'NONE',  ( -114.9999999999991047, 17.00000000000000000, 0.000000000000000000 ) ) ;
#11286 = B_SPLINE_CURVE_WITH_KNOTS ( 'NONE', 3,
 ( #7293, #7558, #38617, #31167 ),
 .UNSPECIFIED., .F., .F.,
 ( 4, 4 ),
 ( 0.001152428489661412592, 0.001623376834729782633 ),
 .UNSPECIFIED. ) ;
#11287 = ORIENTED_EDGE ( 'NONE', *, *, #44046, .F. ) ;
#11288 = DIRECTION ( 'NONE',  ( -0.000000000000000000, -1.000000000000000000, 2.537652627714643577E-15 ) ) ;
#11289 = ORIENTED_EDGE ( 'NONE', *, *, #10168, .F. ) ;
#11290 = DIRECTION ( 'NONE',  ( 1.000000000000000000, 0.000000000000000000, -0.000000000000000000 ) ) ;
#11291 = EDGE_LOOP ( 'NONE', ( #38732, #23193, #40320, #47664, #7383, #45127 ) ) ;
#11292 = DIRECTION ( 'NONE',  ( 0.000000000000000000, -1.000000000000000000, 0.000000000000000000 ) ) ;
#11293 = PLANE ( 'NONE',  #45383 ) ;
#11294 = VERTEX_POINT ( 'NONE', #36385 ) ;
#11295 = ORIENTED_EDGE ( 'NONE', *, *, #36336, .F. ) ;
#11296 = ADVANCED_FACE ( 'NONE', ( #36126 ), #44285, .F. ) ;
#11297 = AXIS2_PLACEMENT_3D ( 'NONE', #21730, #17632, #41740 ) ;
#11298 = VERTEX_POINT ( 'NONE', #20966 ) ;
#11299 = CARTESIAN_POINT ( 'NONE',  ( -84.94597344681493212, 1.025126265847089657, -37.43171244307202272 ) ) ;
#11300 = CARTESIAN_POINT ( 'NONE',  ( 191.5540265531851105, 0.000000000000000000, 162.5682875569279702 ) ) ;
#11301 = ORIENTED_EDGE ( 'NONE', *, *, #27508, .F. ) ;
#11302 = CARTESIAN_POINT ( 'NONE',  ( 340.0000000000000568, 181.0000000000000284, 343.9999999999997726 ) ) ;
#11303 = CARTESIAN_POINT ( 'NONE',  ( -14.99999999999845812, 17.00000000000000000, 35.00000000000000000 ) ) ;
#11304 = ADVANCED_FACE ( 'NONE', ( #40213 ), #39721, .T. ) ;
#11305 = CARTESIAN_POINT ( 'NONE',  ( -8.445973446814976526, 0.000000000000000000, -80.93171244307204404 ) ) ;
#11306 = EDGE_LOOP ( 'NONE', ( #441, #4479, #2873, #38032 ) ) ;
#11307 = ORIENTED_EDGE ( 'NONE', *, *, #49756, .T. ) ;
#11308 = CARTESIAN_POINT ( 'NONE',  ( 1.193089574352119264, 0.2545860991493882342, 9.963925895596188909 ) ) ;
#11309 = LINE ( 'NONE', #48554, #23117 ) ;
#11310 = ORIENTED_EDGE ( 'NONE', *, *, #49595, .T. ) ;
#11311 = DIRECTION ( 'NONE',  ( 0.000000000000000000, 0.000000000000000000, 1.000000000000000000 ) ) ;
#11312 = DIRECTION ( 'NONE',  ( 0.000000000000000000, 0.000000000000000000, 1.000000000000000000 ) ) ;
#11313 = VERTEX_POINT ( 'NONE', #28418 ) ;
#11314 = CARTESIAN_POINT ( 'NONE',  ( 169.0000000000000284, 175.0000000000000284, 343.9999999999998863 ) ) ;
#11315 = CARTESIAN_POINT ( 'NONE',  ( 50.00000000000002132, 0.000000000000000000, 899.9999999999998863 ) ) ;
#11316 = B_SPLINE_SURFACE_WITH_KNOTS ( 'NONE', 3, 3, ( 
 ( #22726, #50638, #15541, #3207 ),
 ( #26835, #9113, #47559, #39660 ),
 ( #8854, #47049, #8609, #1172 ),
 ( #4499, #655, #31454, #11955 ) ),
 .UNSPECIFIED., .F., .F., .F.,
 ( 4, 4 ),
 ( 4, 4 ),
 ( 0.000000000000000000, 1.000000000000000000 ),
 ( 0.000000000000000000, 1.000000000000000000 ),
 .UNSPECIFIED. ) ;
#11317 = VERTEX_POINT ( 'NONE', #31771 ) ;
#11318 = CARTESIAN_POINT ( 'NONE',  ( 191.5540265531851105, 2.143131898507880377E-16, -160.9317124430720298 ) ) ;
#11319 = CARTESIAN_POINT ( 'NONE',  ( 73.30402655318508209, 1.750000000000009992, 160.8182875569279702 ) ) ;
#11320 = CARTESIAN_POINT ( 'NONE',  ( 153.2026953830863647, -97.72914955339486198, -17.31629813440246579 ) ) ;
#11321 = CARTESIAN_POINT ( 'NONE',  ( 210.0000000000000568, 0.000000000000000000, 0.8182875569279768335 ) ) ;
#11322 = ORIENTED_EDGE ( 'NONE', *, *, #18621, .F. ) ;
#11323 = CARTESIAN_POINT ( 'NONE',  ( -0.3370904143228963812, 0.2449105217885287067, 10.00000000000000000 ) ) ;
#11324 = CARTESIAN_POINT ( 'NONE',  ( 112.2789002873379758, -1.749999999999996669, 1.843413822775057609 ) ) ;
#11325 = CARTESIAN_POINT ( 'NONE',  ( -128.4459734468149179, 2.143131898507880377E-16, -160.9317124430720298 ) ) ;
#11326 = ORIENTED_EDGE ( 'NONE', *, *, #3052, .T. ) ;
#11327 = ADVANCED_FACE ( 'NONE', ( #32020 ), #4555, .F. ) ;
#11328 = ORIENTED_EDGE ( 'NONE', *, *, #19813, .T. ) ;
#11329 =( NAMED_UNIT ( * ) PLANE_ANGLE_UNIT ( ) SI_UNIT ( $, .RADIAN. ) );
#11330 = CARTESIAN_POINT ( 'NONE',  ( -168.4459734468149463, 0.000000000000000000, 165.0000000000000000 ) ) ;
#11331 =( BOUNDED_CURVE ( )  B_SPLINE_CURVE ( 3, ( #48632, #25588, #16887, #44303 ),
 .UNSPECIFIED., .F., .F. ) 
 B_SPLINE_CURVE_WITH_KNOTS ( ( 4, 4 ),
 ( 1.570796326794896558, 3.141592653589793116 ),
 .UNSPECIFIED. ) 
 CURVE ( )  GEOMETRIC_REPRESENTATION_ITEM ( )  RATIONAL_B_SPLINE_CURVE ( ( 1.000000000000000000, 0.8047378541243649375, 0.8047378541243649375, 1.000000000000000000 ) ) 
 REPRESENTATION_ITEM ( '' )  );
#11332 = DIRECTION ( 'NONE',  ( -1.000000000000000000, 0.000000000000000000, 0.000000000000000000 ) ) ;
#11333 = B_SPLINE_CURVE_WITH_KNOTS ( 'NONE', 3,
 ( #6698, #46164, #38533, #34423 ),
 .UNSPECIFIED., .F., .F.,
 ( 4, 4 ),
 ( 0.7998230999345287140, 0.9869080488566183140 ),
 .UNSPECIFIED. ) ;
#11334 = VECTOR ( 'NONE', #7884, 1000.000000000000000 ) ;
#11335 = LINE ( 'NONE', #35211, #42964 ) ;
#11336 = CARTESIAN_POINT ( 'NONE',  ( 32.27890028733795447, 1.750000000000009548, -40.20683870891912193 ) ) ;
#11337 = ORIENTED_EDGE ( 'NONE', *, *, #34666, .T. ) ;
#11338 = CARTESIAN_POINT ( 'NONE',  ( 45.88383801556798147, -6.205508426776791708, 7.455576670931136185 ) ) ;
#11339 =( BOUNDED_CURVE ( )  B_SPLINE_CURVE ( 3, ( #17418, #33086, #9713, #36438 ),
 .UNSPECIFIED., .F., .F. ) 
 B_SPLINE_CURVE_WITH_KNOTS ( ( 4, 4 ),
 ( 0.000000000000000000, 1.570796326794896558 ),
 .UNSPECIFIED. ) 
 CURVE ( )  GEOMETRIC_REPRESENTATION_ITEM ( )  RATIONAL_B_SPLINE_CURVE ( ( 1.000000000000000000, 0.8047378541243649375, 0.8047378541243649375, 1.000000000000000000 ) ) 
 REPRESENTATION_ITEM ( '' )  );
#11340 = CARTESIAN_POINT ( 'NONE',  ( 0.5280496040173446870, -0.6453736966177778811, 9.985671801905168010 ) ) ;
#11341 = CARTESIAN_POINT ( 'NONE',  ( -49.75871208702130133, 40.58472229863599523, -5.000000000000000000 ) ) ;
#11342 =( NAMED_UNIT ( * ) SI_UNIT ( $, .STERADIAN. ) SOLID_ANGLE_UNIT ( ) );
#11343 = VERTEX_POINT ( 'NONE', #16869 ) ;
#11344 = CARTESIAN_POINT ( 'NONE',  ( 71.55402655318505367, 0.000000000000000000, 159.0682875569279702 ) ) ;
#11345 = CARTESIAN_POINT ( 'NONE',  ( 0.3370904143228981575, -0.2449105217885261532, 10.00000000000000000 ) ) ;
#11346 = ORIENTED_EDGE ( 'NONE', *, *, #49970, .F. ) ;
#11347 = CARTESIAN_POINT ( 'NONE',  ( -13.35436367797847801, -31.26996044524040741, 7.906207997025717304 ) ) ;
#11348 = CARTESIAN_POINT ( 'NONE',  ( 210.0000000000000568, 0.000000000000000000, 42.56828755692799149 ) ) ;
#11349 = DIRECTION ( 'NONE',  ( 0.000000000000000000, 0.000000000000000000, 1.000000000000000000 ) ) ;
#11350 = EDGE_LOOP ( 'NONE', ( #15039, #25372, #21533, #27221 ) ) ;
#11351 = DIRECTION ( 'NONE',  ( 1.132880637372608740E-16, 4.718402560806925739E-50, 1.000000000000000000 ) ) ;
#11352 = DIRECTION ( 'NONE',  ( -1.000000000000000000, -0.000000000000000000, -0.000000000000000000 ) ) ;
#11353 = ORIENTED_EDGE ( 'NONE', *, *, #22820, .T. ) ;
#11354 = DIRECTION ( 'NONE',  ( -1.000000000000000000, 0.000000000000000000, 0.000000000000000000 ) ) ;
#11355 = FACE_OUTER_BOUND ( 'NONE', #21072, .T. ) ;
#11356 = CARTESIAN_POINT ( 'NONE',  ( 181.0000000000000000, -182.9999999999999716, -340.0000000000001137 ) ) ;
#11357 = EDGE_CURVE ( 'NONE', #11761, #4874, #28165, .T. ) ;
#11358 = ORIENTED_EDGE ( 'NONE', *, *, #39075, .T. ) ;
#11359 = ORIENTED_EDGE ( 'NONE', *, *, #39646, .T. ) ;
#11360 = CARTESIAN_POINT ( 'NONE',  ( 177.5000000000000284, -112.5000000000000000, -10.00000000000000000 ) ) ;
#11361 = DIRECTION ( 'NONE',  ( 0.000000000000000000, 1.000000000000000000, 0.000000000000000000 ) ) ;
#11362 = VECTOR ( 'NONE', #23716, 1000.000000000000000 ) ;
#11363 = ORIENTED_EDGE ( 'NONE', *, *, #32837, .F. ) ;
#11364 = ORIENTED_EDGE ( 'NONE', *, *, #19964, .T. ) ;
#11365 = CARTESIAN_POINT ( 'NONE',  ( -44.94597344681493922, 2.143131898507880377E-16, -77.43171244307198720 ) ) ;
#11366 = CARTESIAN_POINT ( 'NONE',  ( 344.0000000000000000, 185.0000000000000284, -360.0000000000002274 ) ) ;
#11367 = CARTESIAN_POINT ( 'NONE',  ( 35.05402655318504657, 2.143131898507880377E-16, 39.06828755692798438 ) ) ;
#11368 = EDGE_LOOP ( 'NONE', ( #2819, #29190, #47311, #38314 ) ) ;
#11369 = CARTESIAN_POINT ( 'NONE',  ( 1.011271242968688311, -0.7347315653655855927, 10.00000000000000000 ) ) ;
#11370 = ORIENTED_EDGE ( 'NONE', *, *, #44123, .F. ) ;
#11371 = EDGE_CURVE ( 'NONE', #28673, #9737, #6512, .T. ) ;
#11372 = LINE ( 'NONE', #23441, #50026 ) ;
#11373 = AXIS2_PLACEMENT_3D ( 'NONE', #48760, #37294, #10320 ) ;
#11374 = LINE ( 'NONE', #2895, #45514 ) ;
#11375 = ADVANCED_FACE ( 'NONE', ( #4791 ), #30118, .F. ) ;
#11376 = DIRECTION ( 'NONE',  ( -4.758098676964956461E-16, -1.000000000000000000, 0.000000000000000000 ) ) ;
#11377 = ORIENTED_EDGE ( 'NONE', *, *, #49483, .F. ) ;
#11378 = ORIENTED_EDGE ( 'NONE', *, *, #23372, .F. ) ;
#11379 = ORIENTED_EDGE ( 'NONE', *, *, #38427, .F. ) ;
#11380 = CARTESIAN_POINT ( 'NONE',  ( 7.884183412771418986, -42.26678417219199702, 893.0811050474360400 ) ) ;
#11381 = CARTESIAN_POINT ( 'NONE',  ( 356.0000000000001137, 185.0000000000000284, 359.9999999999998295 ) ) ;
#11382 = CARTESIAN_POINT ( 'NONE',  ( -18.37190376999613761, -32.73290680288455690, 1.982731392810413773 ) ) ;
#11383 = ORIENTED_EDGE ( 'NONE', *, *, #2412, .T. ) ;
#11384 = CARTESIAN_POINT ( 'NONE',  ( 0.000000000000000000, 0.000000000000000000, 10.00000000000000000 ) ) ;
#11385 = EDGE_CURVE ( 'NONE', #38545, #3838, #6760, .T. ) ;
#11386 = EDGE_CURVE ( 'NONE', #49071, #42092, #15232, .T. ) ;
#11387 = VERTEX_POINT ( 'NONE', #29864 ) ;
#11388 = DIRECTION ( 'NONE',  ( 0.000000000000000000, 1.604368532695312981E-16, 1.000000000000000000 ) ) ;
#11389 = ORIENTED_EDGE ( 'NONE', *, *, #47410, .T. ) ;
#11390 = ADVANCED_FACE ( 'NONE', ( #41663 ), #42155, .T. ) ;
#11391 = LINE ( 'NONE', #3945, #44867 ) ;
#11392 = CARTESIAN_POINT ( 'NONE',  ( -8.445973446814976526, 0.000000000000000000, 119.0682875569279418 ) ) ;
#11393 = DIRECTION ( 'NONE',  ( 0.000000000000000000, 0.000000000000000000, -1.000000000000000000 ) ) ;
#11394 = ADVANCED_FACE ( 'NONE', ( #22408 ), #45478, .F. ) ;
#11395 = DIRECTION ( 'NONE',  ( 0.000000000000000000, 0.000000000000000000, -1.000000000000000000 ) ) ;
#11396 = EDGE_LOOP ( 'NONE', ( #10647, #28454, #597, #50035 ) ) ;
#11397 = VERTEX_POINT ( 'NONE', #38592 ) ;
#11398 = CARTESIAN_POINT ( 'NONE',  ( 155.0540265531850537, -1.025126265847089657, 119.0682875569279560 ) ) ;
#11399 = CARTESIAN_POINT ( 'NONE',  ( 168.9999999999999716, -272.4999999999999432, -355.9999999999999432 ) ) ;
#11400 = CARTESIAN_POINT ( 'NONE',  ( -26.25702031264333058, 26.77347351953860155, 8.914903342594559632 ) ) ;
#11401 = CARTESIAN_POINT ( 'NONE',  ( -33.43156050989129824, 4.370686678976795747, 8.807470649214879543 ) ) ;
#11402 = AXIS2_PLACEMENT_3D ( 'NONE', #47459, #48214, #16964 ) ;
#11403 = CARTESIAN_POINT ( 'NONE',  ( 166.9999999999999716, -81.49999999999997158, -340.0000000000001137 ) ) ;
#11404 = CARTESIAN_POINT ( 'NONE',  ( 194.3291528190321742, -1.750000000000010436, 79.79316129108087807 ) ) ;
#11405 = VECTOR ( 'NONE', #27990, 1000.000000000000000 ) ;
#11406 = AXIS2_PLACEMENT_3D ( 'NONE', #45669, #42091, #26713 ) ;
#11407 = ORIENTED_EDGE ( 'NONE', *, *, #21373, .T. ) ;
#11408 = AXIS2_PLACEMENT_3D ( 'NONE', #2502, #41502, #37928 ) ;
#11409 = CARTESIAN_POINT ( 'NONE',  ( 357.9999999999999432, 174.9999999999996589, -356.0000000000003411 ) ) ;
#11410 = EDGE_CURVE ( 'NONE', #24755, #35217, #2408, .T. ) ;
#11411 = DIRECTION ( 'NONE',  ( 0.000000000000000000, -1.000000000000000000, -3.186989995019654210E-49 ) ) ;
#11412 = ORIENTED_EDGE ( 'NONE', *, *, #48984, .F. ) ;
#11413 = VECTOR ( 'NONE', #1336, 1000.000000000000000 ) ;
#11414 = EDGE_CURVE ( 'NONE', #48563, #17047, #50317, .T. ) ;
#11415 = EDGE_CURVE ( 'NONE', #29419, #9900, #38339, .T. ) ;
#11416 = CYLINDRICAL_SURFACE ( 'NONE', #32804, 1.750000000000008438 ) ;
#11417 = CARTESIAN_POINT ( 'NONE',  ( 181.0000000000000284, -180.9999999999999716, -115.0000000000001279 ) ) ;
#11418 = CARTESIAN_POINT ( 'NONE',  ( 135.0000000000009663, 16.00000000000000000, -24.99999999999999289 ) ) ;
#11419 = EDGE_CURVE ( 'NONE', #39174, #50425, #18043, .T. ) ;
#11420 = ORIENTED_EDGE ( 'NONE', *, *, #8105, .T. ) ;
#11421 = PRODUCT_DEFINITION_SHAPE ( 'NONE', 'NONE',  #50731 ) ;
#11422 = ORIENTED_EDGE ( 'NONE', *, *, #15552, .F. ) ;
#11423 = CARTESIAN_POINT ( 'NONE',  ( 2.595273106918288164, 2.906811120256387326, 9.741991644047248045 ) ) ;
#11424 = EDGE_CURVE ( 'NONE', #5524, #1440, #10106, .T. ) ;
#11425 = CARTESIAN_POINT ( 'NONE',  ( -4.395207584381336297, -3.942437227415910073, 9.586754400234161366 ) ) ;
#11426 = VERTEX_POINT ( 'NONE', #22164 ) ;
#11427 = ORIENTED_EDGE ( 'NONE', *, *, #32148, .F. ) ;
#11428 = CARTESIAN_POINT ( 'NONE',  ( 0.2257686176849521831, -1.281370980887823974, 9.986087673579140400 ) ) ;
#11429 = LINE ( 'NONE', #35559, #3615 ) ;
#11430 = CARTESIAN_POINT ( 'NONE',  ( -1.249999999999999778, 0.000000000000000000, 10.00000000000000000 ) ) ;
#11431 = ORIENTED_EDGE ( 'NONE', *, *, #42525, .F. ) ;
#11432 = ORIENTED_EDGE ( 'NONE', *, *, #47722, .T. ) ;
#11433 = ORIENTED_EDGE ( 'NONE', *, *, #10588, .T. ) ;
#11434 = AXIS2_PLACEMENT_3D ( 'NONE', #28473, #5867, #1773 ) ;
#11435 = CARTESIAN_POINT ( 'NONE',  ( 112.2789002873379758, -1.749999999999996669, -38.15658617722495194 ) ) ;
#11436 = VECTOR ( 'NONE', #8208, 1000.000000000000000 ) ;
#11437 = LINE ( 'NONE', #35072, #24295 ) ;
#11438 = ORIENTED_EDGE ( 'NONE', *, *, #27102, .T. ) ;
#11439 = VECTOR ( 'NONE', #3126, 1000.000000000000000 ) ;
#11440 = CARTESIAN_POINT ( 'NONE',  ( 2.961022939495062900, -16.59676755884084187, 2.590526750877053086 ) ) ;
#11441 = CARTESIAN_POINT ( 'NONE',  ( 155.0540265531850537, 2.143131898507880377E-16, 165.0000000000000000 ) ) ;
#11442 = CARTESIAN_POINT ( 'NONE',  ( 111.5540265531850679, 0.000000000000000000, -117.4317124430720725 ) ) ;
#11443 = ORIENTED_EDGE ( 'NONE', *, *, #40636, .T. ) ;
#11444 = EDGE_CURVE ( 'NONE', #6332, #17123, #8495, .T. ) ;
#11445 = ORIENTED_EDGE ( 'NONE', *, *, #11890, .F. ) ;
#11446 = DIRECTION ( 'NONE',  ( 1.000000000000000000, -4.758098676964957447E-16, -1.586032892321651989E-16 ) ) ;
#11447 = AXIS2_PLACEMENT_3D ( 'NONE', #29299, #36770, #1600 ) ;
#11448 = ORIENTED_EDGE ( 'NONE', *, *, #29146, .T. ) ;
#11449 = EDGE_CURVE ( 'NONE', #14316, #31951, #14463, .T. ) ;
#11450 = ORIENTED_EDGE ( 'NONE', *, *, #35715, .T. ) ;
#11451 = CARTESIAN_POINT ( 'NONE',  ( 151.5540265531850537, 1.025126265847089657, -120.9317124430720440 ) ) ;
#11452 = VECTOR ( 'NONE', #31498, 1000.000000000000000 ) ;
#11453 = ADVANCED_FACE ( 'NONE', ( #2652 ), #33970, .T. ) ;
#11454 = DIRECTION ( 'NONE',  ( 1.000000000000000000, -4.758098676964957447E-16, 2.958228394578795584E-31 ) ) ;
#11455 = CARTESIAN_POINT ( 'NONE',  ( 71.55402655318505367, 0.000000000000000000, -157.4317124430720014 ) ) ;
#11456 = DIRECTION ( 'NONE',  ( 1.000000000000000000, 0.000000000000000000, 0.000000000000000000 ) ) ;
#11457 = ADVANCED_FACE ( 'NONE', ( #26273 ), #34230, .F. ) ;
#11458 = CARTESIAN_POINT ( 'NONE',  ( 33.16902712922644270, -37.70469005304286725, 1.847720168420772691 ) ) ;
#11459 = ORIENTED_EDGE ( 'NONE', *, *, #4252, .F. ) ;
#11460 = ADVANCED_FACE ( 'NONE', ( #26517 ), #3150, .F. ) ;
#11461 = CARTESIAN_POINT ( 'NONE',  ( 135.0000000000012790, 16.00000000000000000, 30.00000000000000000 ) ) ;
#11462 = EDGE_CURVE ( 'NONE', #39156, #26957, #16241, .T. ) ;
#11463 = CYLINDRICAL_SURFACE ( 'NONE', #10107, 1.750000000000001554 ) ;
#11464 = CARTESIAN_POINT ( 'NONE',  ( 0.9599924130074096729, -0.8495346730527926216, 9.948547179989617462 ) ) ;
#11465 = DIRECTION ( 'NONE',  ( -0.000000000000000000, -0.000000000000000000, -1.000000000000000000 ) ) ;
#11466 = ORIENTED_EDGE ( 'NONE', *, *, #50322, .F. ) ;
#11467 = CYLINDRICAL_SURFACE ( 'NONE', #787, 1.750000000000015543 ) ;
#11468 = CARTESIAN_POINT ( 'NONE',  ( -2.569099690548740877, 50.00000000000000711, 3.199614146704519602 ) ) ;
#11469 = VECTOR ( 'NONE', #41203, 999.9999999999998863 ) ;
#11470 = LINE ( 'NONE', #11724, #45110 ) ;
#11471 = AXIS2_PLACEMENT_3D ( 'NONE', #36568, #23982, #15765 ) ;
#11472 =( BOUNDED_CURVE ( )  B_SPLINE_CURVE ( 3, ( #31245, #42751, #49907, #18903 ),
 .UNSPECIFIED., .F., .F. ) 
 B_SPLINE_CURVE_WITH_KNOTS ( ( 4, 4 ),
 ( 1.570796326794896558, 3.141592653589793116 ),
 .UNSPECIFIED. ) 
 CURVE ( )  GEOMETRIC_REPRESENTATION_ITEM ( )  RATIONAL_B_SPLINE_CURVE ( ( 1.000000000000000000, 0.8047378541243649375, 0.8047378541243649375, 1.000000000000000000 ) ) 
 REPRESENTATION_ITEM ( '' )  );
#11473 = VERTEX_POINT ( 'NONE', #23683 ) ;
#11474 = CARTESIAN_POINT ( 'NONE',  ( -4.945973446814903696, 2.143131898507912917E-16, 159.0682875569279418 ) ) ;
#11475 = EDGE_CURVE ( 'NONE', #29839, #25245, #3668, .T. ) ;
#11476 = CARTESIAN_POINT ( 'NONE',  ( -126.6959734468149321, 1.749999999999997113, -39.18171244307202983 ) ) ;
#11477 = EDGE_LOOP ( 'NONE', ( #8173, #11902, #11646, #8726 ) ) ;
#11478 = FACE_OUTER_BOUND ( 'NONE', #7099, .T. ) ;
#11479 = CYLINDRICAL_SURFACE ( 'NONE', #10696, 2.000000000000001776 ) ;
#11480 = PLANE ( 'NONE',  #13358 ) ;
#11481 = AXIS2_PLACEMENT_3D ( 'NONE', #41984, #49635, #14526 ) ;
#11482 = CARTESIAN_POINT ( 'NONE',  ( -1.011271242968687867, 0.7347315653655861478, 9.972675548442463622 ) ) ;
#11483 =( BOUNDED_CURVE ( )  B_SPLINE_CURVE ( 3, ( #29550, #42358, #14139, #18241 ),
 .UNSPECIFIED., .F., .F. ) 
 B_SPLINE_CURVE_WITH_KNOTS ( ( 4, 4 ),
 ( 3.141592653589793116, 4.712388980384689674 ),
 .UNSPECIFIED. ) 
 CURVE ( )  GEOMETRIC_REPRESENTATION_ITEM ( )  RATIONAL_B_SPLINE_CURVE ( ( 1.000000000000000000, 0.8047378541243649375, 0.8047378541243649375, 1.000000000000000000 ) ) 
 REPRESENTATION_ITEM ( '' )  );
#11484 = VECTOR ( 'NONE', #20283, 1000.000000000000000 ) ;
#11485 = ORIENTED_EDGE ( 'NONE', *, *, #25235, .T. ) ;
#11486 = CARTESIAN_POINT ( 'NONE',  ( -14.48769039275601145, -30.44468701195584970, 8.807470649214879543 ) ) ;
#11487 = PRODUCT_RELATED_PRODUCT_CATEGORY ( 'part', '', ( #10156 ) ) ;
#11488 = VERTEX_POINT ( 'NONE', #27284 ) ;
#11489 = ORIENTED_EDGE ( 'NONE', *, *, #32741, .F. ) ;
#11490 = CYLINDRICAL_SURFACE ( 'NONE', #10694, 1.750000000000008438 ) ;
#11491 = VECTOR ( 'NONE', #8474, 1000.000000000000000 ) ;
#11492 = VERTEX_POINT ( 'NONE', #50575 ) ;
#11493 = LINE ( 'NONE', #3517, #46668 ) ;
#11494 = DIRECTION ( 'NONE',  ( 0.000000000000000000, 0.000000000000000000, 1.000000000000000000 ) ) ;
#11495 = B_SPLINE_CURVE_WITH_KNOTS ( 'NONE', 3,
 ( #40584, #5421, #21073, #36758 ),
 .UNSPECIFIED., .F., .F.,
 ( 4, 4 ),
 ( 0.000000000000000000, 2.647279941188460280E-05 ),
 .UNSPECIFIED. ) ;
#11496 = EDGE_CURVE ( 'NONE', #46434, #3051, #16165, .T. ) ;
#11497 =( BOUNDED_CURVE ( )  B_SPLINE_CURVE ( 3, ( #8686, #48880, #34052, #33799 ),
 .UNSPECIFIED., .F., .F. ) 
 B_SPLINE_CURVE_WITH_KNOTS ( ( 4, 4 ),
 ( 6.280369834734837385E-16, 1.570796326794924758 ),
 .UNSPECIFIED. ) 
 CURVE ( )  GEOMETRIC_REPRESENTATION_ITEM ( )  RATIONAL_B_SPLINE_CURVE ( ( 1.000000000000000000, 0.8047378541243583872, 0.8047378541243583872, 1.000000000000000000 ) ) 
 REPRESENTATION_ITEM ( '' )  );
#11498 = DIRECTION ( 'NONE',  ( -0.000000000000000000, -0.000000000000000000, -1.000000000000000000 ) ) ;
#11499 = ORIENTED_EDGE ( 'NONE', *, *, #35251, .F. ) ;
#11500 = CARTESIAN_POINT ( 'NONE',  ( -115.0000000000000284, 16.00000000000000000, -114.9999999999999858 ) ) ;
#11501 = CARTESIAN_POINT ( 'NONE',  ( 350.0000000000001137, 169.0000000000000000, 359.9999999999997726 ) ) ;
#11502 = DIRECTION ( 'NONE',  ( 1.000000000000000000, 0.000000000000000000, -1.586032892321651989E-16 ) ) ;
#11503 = ORIENTED_EDGE ( 'NONE', *, *, #15272, .T. ) ;
#11504 = CYLINDRICAL_SURFACE ( 'NONE', #4677, 1.750000000000008438 ) ;
#11505 = CARTESIAN_POINT ( 'NONE',  ( 349.9999999999999432, -182.9999999999999716, 355.9999999999997726 ) ) ;
#11506 = EDGE_LOOP ( 'NONE', ( #31069, #11799, #8027, #12826, #39281, #42263, #9530, #8528 ) ) ;
#11507 = EDGE_CURVE ( 'NONE', #10961, #40535, #27021, .T. ) ;
#11508 = VERTEX_POINT ( 'NONE', #20336 ) ;
#11509 = ORIENTED_EDGE ( 'NONE', *, *, #36233, .T. ) ;
#11510 = CARTESIAN_POINT ( 'NONE',  ( 135.0000000000006253, 17.00000000000000000, -30.00000000000000000 ) ) ;
#11511 = DIRECTION ( 'NONE',  ( -1.000000000000000000, -0.000000000000000000, -0.000000000000000000 ) ) ;
#11512 = ORIENTED_EDGE ( 'NONE', *, *, #13177, .T. ) ;
#11513 = AXIS2_PLACEMENT_3D ( 'NONE', #4289, #35610, #17093 ) ;
#11514 = LINE ( 'NONE', #39487, #20879 ) ;
#11515 = CARTESIAN_POINT ( 'NONE',  ( 33.89193117067290473, 21.24469349090191983, 910.0000000000000000 ) ) ;
#11516 = CARTESIAN_POINT ( 'NONE',  ( 0.000000000000000000, 17.00000000000000000, 0.000000000000000000 ) ) ;
#11517 = ADVANCED_FACE ( 'NONE', ( #46987 ), #23437, .F. ) ;
#11518 = VECTOR ( 'NONE', #26750, 1000.000000000000000 ) ;
#11519 = LINE ( 'NONE', #27172, #21071 ) ;
#11520 = CARTESIAN_POINT ( 'NONE',  ( -64.99999999999909051, 16.00000000000000000, 0.000000000000000000 ) ) ;
#11521 = EDGE_CURVE ( 'NONE', #31056, #32520, #8877, .T. ) ;
#11522 = LINE ( 'NONE', #45865, #35701 ) ;
#11523 = CARTESIAN_POINT ( 'NONE',  ( -5.000000000000000000, 165.2000000000000171, -340.2000000000001592 ) ) ;
#11524 = LINE ( 'NONE', #42803, #39062 ) ;
#11525 = VECTOR ( 'NONE', #30702, 1000.000000000000000 ) ;
#11526 = DIRECTION ( 'NONE',  ( 0.000000000000000000, 0.000000000000000000, -1.000000000000000000 ) ) ;
#11527 = VECTOR ( 'NONE', #19391, 1000.000000000000000 ) ;
#11528 = EDGE_CURVE ( 'NONE', #49308, #36027, #12380, .T. ) ;
#11529 = FACE_OUTER_BOUND ( 'NONE', #26711, .T. ) ;
#11530 = VECTOR ( 'NONE', #7951, 1000.000000000000000 ) ;
#11531 = B_SPLINE_CURVE_WITH_KNOTS ( 'NONE', 3,
 ( #9999, #25402, #1306, #16954 ),
 .UNSPECIFIED., .F., .F.,
 ( 4, 4 ),
 ( 0.9895749839358307653, 1.000000000000000000 ),
 .UNSPECIFIED. ) ;
#11532 = ORIENTED_EDGE ( 'NONE', *, *, #3241, .F. ) ;
#11533 = EDGE_CURVE ( 'NONE', #46777, #12549, #4872, .T. ) ;
#11534 = EDGE_CURVE ( 'NONE', #26183, #35621, #851, .T. ) ;
#11535 = DIRECTION ( 'NONE',  ( -1.000000000000000000, 0.000000000000000000, 4.625929269271635797E-16 ) ) ;
#11536 = CARTESIAN_POINT ( 'NONE',  ( 210.0000000000000568, 0.000000000000000000, 40.81828755692798438 ) ) ;
#11537 = CARTESIAN_POINT ( 'NONE',  ( -88.44597344681494633, -1.025126265847089213, -0.9317124430720324924 ) ) ;
#11538 = ORIENTED_EDGE ( 'NONE', *, *, #26445, .T. ) ;
#11539 = CARTESIAN_POINT ( 'NONE',  ( -30.22736451279196856, -39.84193304692609416, -2.408242355805840784 ) ) ;
#11540 = FACE_OUTER_BOUND ( 'NONE', #41201, .T. ) ;
#11541 = EDGE_CURVE ( 'NONE', #16449, #24983, #42914, .T. ) ;
#11542 = CARTESIAN_POINT ( 'NONE',  ( -45.21167770612412085, -22.65616271077779942, 7.906207997025717304 ) ) ;
#11543 = FACE_OUTER_BOUND ( 'NONE', #34422, .T. ) ;
#11544 = CARTESIAN_POINT ( 'NONE',  ( 46.10908423965007330, 19.89422939639137766, 1.847720168420772691 ) ) ;
#11545 = VERTEX_POINT ( 'NONE', #4695 ) ;
#11546 = DIRECTION ( 'NONE',  ( -1.000000000000000000, -0.000000000000000000, -0.000000000000000000 ) ) ;
#11547 = VERTEX_POINT ( 'NONE', #36010 ) ;
#11548 = CARTESIAN_POINT ( 'NONE',  ( 0.000000000000000000, 169.0000000000000000, 359.9999999999997726 ) ) ;
#11549 = ORIENTED_EDGE ( 'NONE', *, *, #31539, .F. ) ;
#11550 = CARTESIAN_POINT ( 'NONE',  ( -5.000000000000000000, 165.2000000000000171, 340.1999999999997044 ) ) ;
#11551 = CARTESIAN_POINT ( 'NONE',  ( 4.999999999999999112, -175.0000000000000284, -350.0000000000002274 ) ) ;
#11552 = ORIENTED_EDGE ( 'NONE', *, *, #31825, .F. ) ;
#11553 =( NAMED_UNIT ( * ) SI_UNIT ( $, .STERADIAN. ) SOLID_ANGLE_UNIT ( ) );
#11554 = ORIENTED_EDGE ( 'NONE', *, *, #49299, .T. ) ;
#11555 = AXIS2_PLACEMENT_3D ( 'NONE', #22012, #29722, #34094 ) ;
#11556 = VECTOR ( 'NONE', #47979, 1000.000000000000000 ) ;
#11557 = ORIENTED_EDGE ( 'NONE', *, *, #44926, .F. ) ;
#11558 = CARTESIAN_POINT ( 'NONE',  ( 15.00000000000000000, 12.98684210526315752, 19.37312575500900280 ) ) ;
#11559 = CARTESIAN_POINT ( 'NONE',  ( -23.79193388295331602, -28.98609808354994044, -9.422646554964178023 ) ) ;
#11560 = ORIENTED_EDGE ( 'NONE', *, *, #10598, .T. ) ;
#11561 = CARTESIAN_POINT ( 'NONE',  ( -1.011271242968683426, -0.7347315653655928092, -3.333333333333333481 ) ) ;
#11562 = CARTESIAN_POINT ( 'NONE',  ( -1.347864860736281756, -0.3239901621376108931, 9.960033073700792272 ) ) ;
#11563 = DIRECTION ( 'NONE',  ( 0.000000000000000000, -1.000000000000000000, -0.000000000000000000 ) ) ;
#11564 = ORIENTED_EDGE ( 'NONE', *, *, #17707, .F. ) ;
#11565 = VECTOR ( 'NONE', #39949, 1000.000000000000000 ) ;
#11566 = DIRECTION ( 'NONE',  ( -1.000000000000000000, -0.000000000000000000, -0.000000000000000000 ) ) ;
#11567 = EDGE_CURVE ( 'NONE', #47489, #15143, #35502, .T. ) ;
#11568 = DIRECTION ( 'NONE',  ( -1.586032892321652236E-16, -1.000000000000000000, -6.853681917100419162E-49 ) ) ;
#11569 = ORIENTED_EDGE ( 'NONE', *, *, #11766, .T. ) ;
#11570 = CARTESIAN_POINT ( 'NONE',  ( 164.9999999999999716, 17.00000000000000000, 59.99999999999999289 ) ) ;
#11571 = CARTESIAN_POINT ( 'NONE',  ( -9.696760411816217839, -2.443938934554997999, 0.000000000000000000 ) ) ;
#11572 = ORIENTED_EDGE ( 'NONE', *, *, #3490, .F. ) ;
#11573 = LINE ( 'NONE', #33109, #42563 ) ;
#11574 = FACE_OUTER_BOUND ( 'NONE', #7403, .T. ) ;
#11575 = ORIENTED_EDGE ( 'NONE', *, *, #21603, .T. ) ;
#11576 = PLANE ( 'NONE',  #1351 ) ;
#11577 = CARTESIAN_POINT ( 'NONE',  ( 130.0000000000008811, 16.00000000000000000, 0.000000000000000000 ) ) ;
#11578 = FACE_OUTER_BOUND ( 'NONE', #39591, .T. ) ;
#11579 = DIRECTION ( 'NONE',  ( -4.759647537211363479E-16, 5.772796816983493182E-42, -1.000000000000000000 ) ) ;
#11580 = EDGE_CURVE ( 'NONE', #19058, #15809, #18587, .T. ) ;
#11581 = ADVANCED_FACE ( 'NONE', ( #11633 ), #2682, .T. ) ;
#11582 = ORIENTED_EDGE ( 'NONE', *, *, #12792, .F. ) ;
#11583 =( BOUNDED_CURVE ( )  B_SPLINE_CURVE ( 3, ( #47384, #4342, #39501, #741 ),
 .UNSPECIFIED., .F., .F. ) 
 B_SPLINE_CURVE_WITH_KNOTS ( ( 4, 4 ),
 ( 4.712388980384689674, 6.283185307179586232 ),
 .UNSPECIFIED. ) 
 CURVE ( )  GEOMETRIC_REPRESENTATION_ITEM ( )  RATIONAL_B_SPLINE_CURVE ( ( 1.000000000000000000, 0.8047378541243649375, 0.8047378541243649375, 1.000000000000000000 ) ) 
 REPRESENTATION_ITEM ( '' )  );
#11584 = CARTESIAN_POINT ( 'NONE',  ( -12.78770032058971395, -31.68259716188267916, 7.455576670931136185 ) ) ;
#11585 = FACE_OUTER_BOUND ( 'NONE', #44344, .T. ) ;
#11586 = DIRECTION ( 'NONE',  ( 1.000000000000000000, 0.000000000000000000, 0.000000000000000000 ) ) ;
#11587 = VERTEX_POINT ( 'NONE', #20585 ) ;
#11589 = ORIENTED_EDGE ( 'NONE', *, *, #42773, .F. ) ;
#11588 = VECTOR ( 'NONE', #16752, 1000.000000000000000 ) ;
#11590 = EDGE_CURVE ( 'NONE', #48199, #42713, #29758, .T. ) ;
#11591 = EDGE_CURVE ( 'NONE', #5571, #19596, #17248, .T. ) ;
#11592 = DIRECTION ( 'NONE',  ( 3.172065745548403743E-16, 1.000000000000000000, 0.000000000000000000 ) ) ;
#11593 = FILL_AREA_STYLE_COLOUR ( '', #24253 ) ;
#11594 = CARTESIAN_POINT ( 'NONE',  ( 50.00000000000000000, -50.00000000000000000, 900.0000000000000000 ) ) ;
#11595 = CARTESIAN_POINT ( 'NONE',  ( 0.000000000000000000, 17.00000000000000000, 0.000000000000000000 ) ) ;
#11596 = EDGE_LOOP ( 'NONE', ( #16940, #15100, #32530, #5356, #27897, #5139 ) ) ;
#11597 = B_SPLINE_CURVE_WITH_KNOTS ( 'NONE', 3,
 ( #33234, #9614, #48816, #13703 ),
 .UNSPECIFIED., .F., .F.,
 ( 4, 4 ),
 ( 0.003855596587714113684, 0.009994105792438251826 ),
 .UNSPECIFIED. ) ;
#11598 = EDGE_CURVE ( 'NONE', #34075, #28181, #39966, .T. ) ;
#11599 = CARTESIAN_POINT ( 'NONE',  ( 193.3040265531851105, -1.750000000000010658, 120.8182875569279702 ) ) ;
#11600 = VECTOR ( 'NONE', #49654, 1000.000000000000000 ) ;
#11602 = CIRCLE ( 'NONE', #9974, 1.750000000000008438 ) ;
#11601 = CARTESIAN_POINT ( 'NONE',  ( -0.3862712429686809279, -1.188820645368943163, 10.00000000000000000 ) ) ;
#11603 = DIRECTION ( 'NONE',  ( 0.000000000000000000, 0.000000000000000000, 1.000000000000000000 ) ) ;
#11604 = SURFACE_SIDE_STYLE ('',( #16207 ) ) ;
#11605 = ORIENTED_EDGE ( 'NONE', *, *, #48140, .F. ) ;
#11606 = ORIENTED_EDGE ( 'NONE', *, *, #3581, .F. ) ;
#11607 = FACE_OUTER_BOUND ( 'NONE', #47098, .T. ) ;
#11608 = FACE_OUTER_BOUND ( 'NONE', #2700, .T. ) ;
#11609 = ORIENTED_EDGE ( 'NONE', *, *, #21739, .F. ) ;
#11610 = CARTESIAN_POINT ( 'NONE',  ( -88.44597344681491791, 2.143131898507880377E-16, -160.9317124430720298 ) ) ;
#11611 = CARTESIAN_POINT ( 'NONE',  ( -54.99999999999997868, 52.49999999999999289, 5.000000000000000000 ) ) ;
#11612 = CARTESIAN_POINT ( 'NONE',  ( -8.445973446814914354, 0.000000000000000000, 162.5682875569279702 ) ) ;
#11613 = ORIENTED_EDGE ( 'NONE', *, *, #17860, .F. ) ;
#11614 = DIRECTION ( 'NONE',  ( -0.000000000000000000, -1.000000000000000000, -0.000000000000000000 ) ) ;
#11615 = PLANE ( 'NONE',  #27074 ) ;
#11616 = ORIENTED_EDGE ( 'NONE', *, *, #26864, .F. ) ;
#11617 = DIRECTION ( 'NONE',  ( 1.000000000000000000, 0.000000000000000000, 0.000000000000000000 ) ) ;
#11618 = CARTESIAN_POINT ( 'NONE',  ( 34.32915281903212446, 1.750000000000010214, 81.84341382277507648 ) ) ;
#11619 = UNCERTAINTY_MEASURE_WITH_UNIT (LENGTH_MEASURE( 1.000000000000000082E-05 ), #8724, 'distance_accuracy_value', 'NONE');
#11620 = CARTESIAN_POINT ( 'NONE',  ( 31.55402655318503236, 0.000000000000000000, 165.0000000000000000 ) ) ;
#11621 = AXIS2_PLACEMENT_3D ( 'NONE', #17369, #9669, #6070 ) ;
#11622 = EDGE_LOOP ( 'NONE', ( #10044, #17983, #47493, #42144 ) ) ;
#11623 = EDGE_LOOP ( 'NONE', ( #21465, #30913, #28501, #21446 ) ) ;
#11624 = DIRECTION ( 'NONE',  ( -1.000000000000000000, 0.000000000000000000, -0.000000000000000000 ) ) ;
#11625 = CARTESIAN_POINT ( 'NONE',  ( 339.9999999999999432, -169.0000000000001137, -344.0000000000002842 ) ) ;
#11626 = EDGE_CURVE ( 'NONE', #49290, #41616, #38534, .T. ) ;
#11627 = ORIENTED_EDGE ( 'NONE', *, *, #11716, .F. ) ;
#11628 = AXIS2_PLACEMENT_3D ( 'NONE', #28823, #44444, #9322 ) ;
#11629 = DIRECTION ( 'NONE',  ( -1.000000000000000000, -0.000000000000000000, -0.000000000000000000 ) ) ;
#11630 = CARTESIAN_POINT ( 'NONE',  ( 358.0000000000000000, 165.0000000000000000, -106.0000000000001990 ) ) ;
#11631 = CARTESIAN_POINT ( 'NONE',  ( -119.9999999999981668, 17.00000000000000000, 65.00000000000000000 ) ) ;
#11632 = ORIENTED_EDGE ( 'NONE', *, *, #32563, .F. ) ;
#11633 = FACE_OUTER_BOUND ( 'NONE', #32708, .T. ) ;
#11634 = EDGE_LOOP ( 'NONE', ( #6748, #7122, #27921, #204 ) ) ;
#11635 = FACE_OUTER_BOUND ( 'NONE', #3093, .T. ) ;
#11636 = CARTESIAN_POINT ( 'NONE',  ( -126.6959734468149321, -1.749999999999997113, -39.18171244307202983 ) ) ;
#11637 =( BOUNDED_CURVE ( )  B_SPLINE_CURVE ( 3, ( #30023, #41055, #29254, #49210 ),
 .UNSPECIFIED., .F., .F. ) 
 B_SPLINE_CURVE_WITH_KNOTS ( ( 4, 4 ),
 ( 1.570796326794896558, 3.141592653589793116 ),
 .UNSPECIFIED. ) 
 CURVE ( )  GEOMETRIC_REPRESENTATION_ITEM ( )  RATIONAL_B_SPLINE_CURVE ( ( 1.000000000000000000, 0.8047378541243649375, 0.8047378541243649375, 1.000000000000000000 ) ) 
 REPRESENTATION_ITEM ( '' )  );
#11638 = DIRECTION ( 'NONE',  ( 0.000000000000000000, 0.000000000000000000, 1.000000000000000000 ) ) ;
#11639 = VERTEX_POINT ( 'NONE', #24704 ) ;
#11640 = EDGE_LOOP ( 'NONE', ( #18726, #26186, #37435, #3528 ) ) ;
#11641 = ORIENTED_EDGE ( 'NONE', *, *, #34464, .T. ) ;
#11642 = CYLINDRICAL_SURFACE ( 'NONE', #34520, 1.750000000000015543 ) ;
#11643 = DIRECTION ( 'NONE',  ( -0.000000000000000000, -0.000000000000000000, -1.000000000000000000 ) ) ;
#11644 =( BOUNDED_CURVE ( )  B_SPLINE_CURVE ( 3, ( #1436, #44498, #4764, #28122 ),
 .UNSPECIFIED., .F., .F. ) 
 B_SPLINE_CURVE_WITH_KNOTS ( ( 4, 4 ),
 ( 4.712388980384689674, 6.283185307179586232 ),
 .UNSPECIFIED. ) 
 CURVE ( )  GEOMETRIC_REPRESENTATION_ITEM ( )  RATIONAL_B_SPLINE_CURVE ( ( 1.000000000000000000, 0.8047378541243649375, 0.8047378541243649375, 1.000000000000000000 ) ) 
 REPRESENTATION_ITEM ( '' )  );
#11645 = LINE ( 'NONE', #27298, #10963 ) ;
#11646 = ORIENTED_EDGE ( 'NONE', *, *, #34991, .T. ) ;
#11647 = CARTESIAN_POINT ( 'NONE',  ( 195.0540265531851105, 2.143131898507880377E-16, 39.06828755692798438 ) ) ;
#11648 = VERTEX_POINT ( 'NONE', #48496 ) ;
#11649 = PLANE ( 'NONE',  #46292 ) ;
#11650 = VERTEX_POINT ( 'NONE', #33168 ) ;
#11651 = DIRECTION ( 'NONE',  ( -0.000000000000000000, -0.000000000000000000, -1.000000000000000000 ) ) ;
#11652 = FACE_OUTER_BOUND ( 'NONE', #18192, .T. ) ;
#11653 = FACE_BOUND ( 'NONE', #34978, .T. ) ;
#11654 = CARTESIAN_POINT ( 'NONE',  ( 2.961022939495062900, -16.59676755884084187, 2.590526750877053086 ) ) ;
#11655 = VERTEX_POINT ( 'NONE', #9543 ) ;
#11656 = ORIENTED_EDGE ( 'NONE', *, *, #27730, .T. ) ;
#11657 = EDGE_CURVE ( 'NONE', #15177, #11925, #1851, .T. ) ;
#11658 = CARTESIAN_POINT ( 'NONE',  ( -28.97821631107938245, -35.56709536735906596, -9.367992836599951190 ) ) ;
#11659 = AXIS2_PLACEMENT_3D ( 'NONE', #4136, #19509, #27234 ) ;
#11660 = DIRECTION ( 'NONE',  ( 1.132880637372608740E-16, 4.718402560806925739E-50, 1.000000000000000000 ) ) ;
#11661 = CARTESIAN_POINT ( 'NONE',  ( -31.93002621080269421, -9.285431160462335853, -2.408242355805840784 ) ) ;
#11662=STYLED_ITEM('',(#50747),#38377);
#11663 = CARTESIAN_POINT ( 'NONE',  ( -33.64889274059387958, 3.704246042440976439, 8.356839323120299312 ) ) ;
#11664 = AXIS2_PLACEMENT_3D ( 'NONE', #20012, #3858, #282 ) ;
#11665 = DIRECTION ( 'NONE',  ( 0.000000000000000000, 0.000000000000000000, 1.000000000000000000 ) ) ;
#11666 = VERTEX_POINT ( 'NONE', #9292 ) ;
#11667 = DIRECTION ( 'NONE',  ( 0.000000000000000000, 0.000000000000000000, -1.000000000000000000 ) ) ;
#11668 = PLANE ( 'NONE',  #10740 ) ;
#11669 = VERTEX_POINT ( 'NONE', #40349 ) ;
#11670 = CARTESIAN_POINT ( 'NONE',  ( 114.3291528190321173, -1.749999999999996669, -160.2068387089191219 ) ) ;
#11671 = DIRECTION ( 'NONE',  ( 0.000000000000000000, -0.000000000000000000, 1.000000000000000000 ) ) ;
#11672 = VECTOR ( 'NONE', #25764, 1000.000000000000000 ) ;
#11673 = ORIENTED_EDGE ( 'NONE', *, *, #29003, .F. ) ;
#11674 = ORIENTED_EDGE ( 'NONE', *, *, #41643, .T. ) ;
#11675 = CARTESIAN_POINT ( 'NONE',  ( -86.69597344681496054, 0.000000000000000000, 165.0000000000000000 ) ) ;
#11676 = CARTESIAN_POINT ( 'NONE',  ( -4.763548243873389154, 16.57409059453848599, 8.727788335465566760 ) ) ;
#11677 = VERTEX_POINT ( 'NONE', #44907 ) ;
#11678 = VERTEX_POINT ( 'NONE', #25193 ) ;
#11679 = CARTESIAN_POINT ( 'NONE',  ( 194.3291528190321742, -1.750000000000009326, -158.1565861772249377 ) ) ;
#11680 = CARTESIAN_POINT ( 'NONE',  ( -126.6959734468149321, -1.749999999999996891, -159.1817124430720298 ) ) ;
#11681 = LINE ( 'NONE', #15027, #31653 ) ;
#11682 = DIRECTION ( 'NONE',  ( 0.000000000000000000, -1.000000000000000000, 2.537652627714643577E-15 ) ) ;
#11683 = VECTOR ( 'NONE', #12457, 1000.000000000000000 ) ;
#11684 = VERTEX_POINT ( 'NONE', #36262 ) ;
#11685 = EDGE_LOOP ( 'NONE', ( #41933, #6386, #33913, #47716, #3158, #7138, #16904, #32036 ) ) ;
#11686 = ORIENTED_EDGE ( 'NONE', *, *, #13992, .F. ) ;
#11687 = AXIS2_PLACEMENT_3D ( 'NONE', #49725, #23591, #31309 ) ;
#11688 = CARTESIAN_POINT ( 'NONE',  ( -5.000000000000000000, 184.8000000000000114, -340.2000000000001592 ) ) ;
#11689 = CARTESIAN_POINT ( 'NONE',  ( 1.468446590252912465, 0.3226319952343980058, 9.953784399990622589 ) ) ;
#11690 = ORIENTED_EDGE ( 'NONE', *, *, #19101, .F. ) ;
#11691 = CARTESIAN_POINT ( 'NONE',  ( 2.462075149652696027, -16.57295996686994499, 9.403735324607438884 ) ) ;
#11692 = VECTOR ( 'NONE', #34199, 1000.000000000000000 ) ;
#11693 = CYLINDRICAL_SURFACE ( 'NONE', #13479, 1.749999999999987566 ) ;
#11694 = CARTESIAN_POINT ( 'NONE',  ( 113.3040265531850537, 1.749999999999997335, -119.1817124430720440 ) ) ;
#11695 = EDGE_LOOP ( 'NONE', ( #10868, #25158, #44901, #32406 ) ) ;
#11696 = ORIENTED_EDGE ( 'NONE', *, *, #38792, .F. ) ;
#11697 = PLANE ( 'NONE',  #5759 ) ;
#11698 = CARTESIAN_POINT ( 'NONE',  ( -207.7210997126620384, 1.750000000000009326, 161.8434138227750907 ) ) ;
#11699 = PLANE ( 'NONE',  #36378 ) ;
#11700 = UNCERTAINTY_MEASURE_WITH_UNIT (LENGTH_MEASURE( 1.000000000000000082E-05 ), #951, 'distance_accuracy_value', 'NONE');
#11701 = ORIENTED_EDGE ( 'NONE', *, *, #34184, .T. ) ;
#11702 = ORIENTED_EDGE ( 'NONE', *, *, #48789, .T. ) ;
#11703 = PLANE ( 'NONE',  #15167 ) ;
#11704 = CARTESIAN_POINT ( 'NONE',  ( -1.011271242968688533, 0.7347315653655859258, 10.00000000000000000 ) ) ;
#11705 = ORIENTED_EDGE ( 'NONE', *, *, #22067, .F. ) ;
#11706 = DIRECTION ( 'NONE',  ( 1.000000000000000000, 0.000000000000000000, -0.000000000000000000 ) ) ;
#11707 = CARTESIAN_POINT ( 'NONE',  ( -194.9999999999999432, 164.9999999999999716, 500.0000000000000000 ) ) ;
#11708 = CARTESIAN_POINT ( 'NONE',  ( 177.5000000000000000, -112.5000000000000000, -9.999999999999973355 ) ) ;
#11709 = EDGE_CURVE ( 'NONE', #29240, #1237, #26209, .T. ) ;
#11710 = DIRECTION ( 'NONE',  ( -0.000000000000000000, -0.000000000000000000, -1.000000000000000000 ) ) ;
#11711 = EDGE_LOOP ( 'NONE', ( #47855, #4087, #15393, #45401, #48375, #15700 ) ) ;
#11712 = EDGE_CURVE ( 'NONE', #48164, #16958, #6419, .T. ) ;
#11713 = CARTESIAN_POINT ( 'NONE',  ( 2.188678504086826848, -0.3267089737525829540, 9.881002359080282460 ) ) ;
#11714 = CARTESIAN_POINT ( 'NONE',  ( 343.9999999999999432, -185.0000000000001421, -360.0000000000003979 ) ) ;
#11715 = CARTESIAN_POINT ( 'NONE',  ( 1.024768877994822525, -0.8112356146995051143, 9.945465957785110334 ) ) ;
#11716 = EDGE_CURVE ( 'NONE', #950, #42829, #25450, .T. ) ;
#11717 = CARTESIAN_POINT ( 'NONE',  ( -46.69597344681494633, 0.000000000000000000, 165.0000000000000000 ) ) ;
#11718 = EDGE_CURVE ( 'NONE', #26763, #38804, #32147, .T. ) ;
#11719 = ORIENTED_EDGE ( 'NONE', *, *, #12666, .T. ) ;
#11720 = DIRECTION ( 'NONE',  ( 0.000000000000000000, 0.000000000000000000, 1.000000000000000000 ) ) ;
#11721 = VECTOR ( 'NONE', #243, 1000.000000000000000 ) ;
#11722 = EDGE_CURVE ( 'NONE', #22827, #1115, #37028, .T. ) ;
#11723 = DIRECTION ( 'NONE',  ( 1.000000000000000000, 0.000000000000000000, 0.000000000000000000 ) ) ;
#11724 = CARTESIAN_POINT ( 'NONE',  ( -64.99999999999909051, 17.00000000000000000, 0.000000000000000000 ) ) ;
#11725 = VECTOR ( 'NONE', #50156, 1000.000000000000000 ) ;
#11726 = EDGE_LOOP ( 'NONE', ( #37971, #32681, #14504, #36088 ) ) ;
#11727 = PLANE ( 'NONE',  #34672 ) ;
#11728 = VECTOR ( 'NONE', #17334, 1000.000000000000000 ) ;
#11729 = CARTESIAN_POINT ( 'NONE',  ( 73.30402655318508209, -1.750000000000009992, 0.8182875569279768335 ) ) ;
#11730 = ORIENTED_EDGE ( 'NONE', *, *, #47843, .F. ) ;
#11731 = CARTESIAN_POINT ( 'NONE',  ( -54.99999999999997868, 52.49999999999999289, 5.000000000000000000 ) ) ;
#11732 = CARTESIAN_POINT ( 'NONE',  ( 2.538055338523173443, 33.28424297489108596, -9.367992836599951190 ) ) ;
#11733 = DIRECTION ( 'NONE',  ( 0.000000000000000000, 1.000000000000000000, 0.000000000000000000 ) ) ;
#11734 = DIRECTION ( 'NONE',  ( -0.000000000000000000, -0.000000000000000000, -1.000000000000000000 ) ) ;
#11735 = ORIENTED_EDGE ( 'NONE', *, *, #25201, .F. ) ;
#11736 = CARTESIAN_POINT ( 'NONE',  ( 0.8155877869298099325, 0.9072449372238458043, 9.963925895597341764 ) ) ;
#11737 = B_SPLINE_SURFACE_WITH_KNOTS ( 'NONE', 3, 3, ( 
 ( #41815, #17948, #2069, #45131 ),
 ( #14878, #10015, #18461, #18705 ),
 ( #2309, #42322, #13844, #33631 ),
 ( #33382, #30527, #46127, #48954 ) ),
 .UNSPECIFIED., .F., .F., .F.,
 ( 4, 4 ),
 ( 4, 4 ),
 ( 0.000000000000000000, 1.000000000000000000 ),
 ( 0.000000000000000000, 1.000000000000000000 ),
 .UNSPECIFIED. ) ;
#11738 = ADVANCED_FACE ( 'NONE', ( #12882 ), #32395, .F. ) ;
#11740 = VERTEX_POINT ( 'NONE', #40600 ) ;
#11739 = ADVANCED_FACE ( 'NONE', ( #28797 ), #24952, .T. ) ;
#11741 = ORIENTED_EDGE ( 'NONE', *, *, #37602, .T. ) ;
#11742 = LINE ( 'NONE', #39461, #25908 ) ;
#11743 = DIRECTION ( 'NONE',  ( 0.000000000000000000, -1.000000000000000000, -0.000000000000000000 ) ) ;
#11744 = ADVANCED_FACE ( 'NONE', ( #5435 ), #21339, .F. ) ;
#11745 = EDGE_CURVE ( 'NONE', #12553, #14822, #36077, .T. ) ;
#11746 = ORIENTED_EDGE ( 'NONE', *, *, #7316, .F. ) ;
#11747 = DIRECTION ( 'NONE',  ( 0.000000000000000000, 0.000000000000000000, 1.000000000000000000 ) ) ;
#11748 = LINE ( 'NONE', #4552, #12624 ) ;
#11749 = EDGE_CURVE ( 'NONE', #40397, #13851, #49751, .T. ) ;
#11750 = EDGE_CURVE ( 'NONE', #47505, #7355, #13720, .T. ) ;
#11751 = DIRECTION ( 'NONE',  ( -0.000000000000000000, -0.000000000000000000, -1.000000000000000000 ) ) ;
#11752 = ORIENTED_EDGE ( 'NONE', *, *, #20969, .T. ) ;
#11753 = DIRECTION ( 'NONE',  ( 0.000000000000000000, 1.000000000000000000, 1.544785076050074834E-48 ) ) ;
#11754 = CARTESIAN_POINT ( 'NONE',  ( 50.24128791297869867, 41.04536285977714982, 5.000000000000000000 ) ) ;
#11755 = SURFACE_STYLE_USAGE ( .BOTH. , #34868 ) ;
#11756 = ORIENTED_EDGE ( 'NONE', *, *, #3567, .F. ) ;
#11757 = CARTESIAN_POINT ( 'NONE',  ( 36.08557433729230723, -35.58569447144768105, 7.455576670931136185 ) ) ;
#11758 = CIRCLE ( 'NONE', #10138, 2.000000000000001776 ) ;
#11759 = ORIENTED_EDGE ( 'NONE', *, *, #14623, .T. ) ;
#11760 = ORIENTED_EDGE ( 'NONE', *, *, #7601, .F. ) ;
#11761 = VERTEX_POINT ( 'NONE', #3094 ) ;
#11762 = CARTESIAN_POINT ( 'NONE',  ( -26.25702031264333058, 26.77347351953860155, 8.914903342594559632 ) ) ;
#11763 = AXIS2_PLACEMENT_3D ( 'NONE', #35347, #39689, #28129 ) ;
#11764 = LINE ( 'NONE', #19452, #43867 ) ;
#11765 = VERTEX_POINT ( 'NONE', #6444 ) ;
#11766 = EDGE_CURVE ( 'NONE', #41541, #20063, #25861, .T. ) ;
#11767 = LINE ( 'NONE', #50195, #28287 ) ;
#11768 = FACE_OUTER_BOUND ( 'NONE', #13353, .T. ) ;
#11769 = DIRECTION ( 'NONE',  ( 0.000000000000000000, -0.000000000000000000, -1.000000000000000000 ) ) ;
#11770 = EDGE_CURVE ( 'NONE', #14892, #50433, #10634, .T. ) ;
#11771 = CARTESIAN_POINT ( 'NONE',  ( -128.4459734468149463, 1.025126265847081219, -157.4317124430720582 ) ) ;
#11772 = EDGE_CURVE ( 'NONE', #22529, #8610, #2586, .T. ) ;
#11773 = AXIS2_PLACEMENT_3D ( 'NONE', #16026, #31689, #4966 ) ;
#11774 = DIRECTION ( 'NONE',  ( -1.000000000000000000, -0.000000000000000000, -0.000000000000000000 ) ) ;
#11775 = CARTESIAN_POINT ( 'NONE',  ( -207.7210997126620384, 1.750000000000009548, 39.79316129108089228 ) ) ;
#11776 = LINE ( 'NONE', #27934, #21832 ) ;
#11777 = CARTESIAN_POINT ( 'NONE',  ( -164.9999999999994031, 17.00000000000000000, -30.00000000000000000 ) ) ;
#11778 = DIRECTION ( 'NONE',  ( 1.000000000000000000, 0.000000000000000000, 0.000000000000000000 ) ) ;
#11779 = EDGE_CURVE ( 'NONE', #19115, #47355, #11333, .T. ) ;
#11780 = ORIENTED_EDGE ( 'NONE', *, *, #41446, .T. ) ;
#11781 = CARTESIAN_POINT ( 'NONE',  ( 210.0000000000000568, 0.000000000000000000, 82.56828755692799859 ) ) ;
#11782 =( BOUNDED_CURVE ( )  B_SPLINE_CURVE ( 3, ( #21428, #45259, #17335, #13482 ),
 .UNSPECIFIED., .F., .F. ) 
 B_SPLINE_CURVE_WITH_KNOTS ( ( 4, 4 ),
 ( 1.570796326794896558, 3.141592653589793116 ),
 .UNSPECIFIED. ) 
 CURVE ( )  GEOMETRIC_REPRESENTATION_ITEM ( )  RATIONAL_B_SPLINE_CURVE ( ( 1.000000000000000000, 0.8047378541243649375, 0.8047378541243649375, 1.000000000000000000 ) ) 
 REPRESENTATION_ITEM ( '' )  );
#11783 = CARTESIAN_POINT ( 'NONE',  ( -14.49999999999999822, -46.12433806312137108, -6.404467680894764925 ) ) ;
#11784 = CIRCLE ( 'NONE', #33117, 2.000000000000001776 ) ;
#11785 = DIRECTION ( 'NONE',  ( 0.000000000000000000, -0.9749645535258959494, 0.2223603367690620558 ) ) ;
#11786 = CARTESIAN_POINT ( 'NONE',  ( -210.0000000000000568, 0.000000000000000000, 160.8182875569279702 ) ) ;
#11787 = EDGE_LOOP ( 'NONE', ( #37573, #42010, #7245, #32965, #35867, #44418 ) ) ;
#11788 = CARTESIAN_POINT ( 'NONE',  ( -1.011271242968683426, -0.7347315653655928092, 10.00000000000000000 ) ) ;
#11789 =( BOUNDED_CURVE ( )  B_SPLINE_CURVE ( 3, ( #14987, #38862, #50076, #3685 ),
 .UNSPECIFIED., .F., .F. ) 
 B_SPLINE_CURVE_WITH_KNOTS ( ( 4, 4 ),
 ( 1.570796326794896558, 3.141592653589793116 ),
 .UNSPECIFIED. ) 
 CURVE ( )  GEOMETRIC_REPRESENTATION_ITEM ( )  RATIONAL_B_SPLINE_CURVE ( ( 1.000000000000000000, 0.8047378541243649375, 0.8047378541243649375, 1.000000000000000000 ) ) 
 REPRESENTATION_ITEM ( '' )  );
#11790 = CARTESIAN_POINT ( 'NONE',  ( 0.9870575514054733546, 1.980598328282569653, 9.881002359080278907 ) ) ;
#11791 = LINE ( 'NONE', #11285, #11931 ) ;
#11792 = CARTESIAN_POINT ( 'NONE',  ( -0.1287570809895602630, -0.3962735484563142396, 10.00000000000000000 ) ) ;
#11793 = ORIENTED_EDGE ( 'NONE', *, *, #39046, .T. ) ;
#11794 = CARTESIAN_POINT ( 'NONE',  ( -42.99990394833793772, 47.95759300784327905, 5.000000000000000000 ) ) ;
#11795 = ORIENTED_EDGE ( 'NONE', *, *, #27860, .F. ) ;
#11796 = CARTESIAN_POINT ( 'NONE',  ( 80.00000000000216005, 16.00000000000000000, 95.00000000000000000 ) ) ;
#11797 = AXIS2_PLACEMENT_3D ( 'NONE', #44343, #45092, #44840 ) ;
#11798 = EDGE_CURVE ( 'NONE', #35326, #22662, #22345, .T. ) ;
#11799 = ORIENTED_EDGE ( 'NONE', *, *, #12370, .T. ) ;
#11800 = DIRECTION ( 'NONE',  ( -1.000000000000000000, -0.000000000000000000, -0.000000000000000000 ) ) ;
#11801 = AXIS2_PLACEMENT_3D ( 'NONE', #31038, #10507, #46632 ) ;
#11802 = CARTESIAN_POINT ( 'NONE',  ( -19.99999999999908695, 17.00000000000000000, -24.99999999999999289 ) ) ;
#11803 =( BOUNDED_CURVE ( )  B_SPLINE_CURVE ( 3, ( #36663, #5570, #982, #5827 ),
 .UNSPECIFIED., .F., .F. ) 
 B_SPLINE_CURVE_WITH_KNOTS ( ( 4, 4 ),
 ( 4.712388980384689674, 6.283185307179586232 ),
 .UNSPECIFIED. ) 
 CURVE ( )  GEOMETRIC_REPRESENTATION_ITEM ( )  RATIONAL_B_SPLINE_CURVE ( ( 1.000000000000000000, 0.8047378541243649375, 0.8047378541243649375, 1.000000000000000000 ) ) 
 REPRESENTATION_ITEM ( '' )  );
#11804 = ORIENTED_EDGE ( 'NONE', *, *, #36530, .F. ) ;
#11805 = DIRECTION ( 'NONE',  ( -1.000000000000000000, -0.000000000000000000, -0.000000000000000000 ) ) ;
#11806 = VERTEX_POINT ( 'NONE', #49504 ) ;
#11807 = AXIS2_PLACEMENT_3D ( 'NONE', #451, #16094, #693 ) ;
#11808 = CIRCLE ( 'NONE', #4406, 6.000000000000000888 ) ;
#11809 = EDGE_CURVE ( 'NONE', #8304, #24192, #41322, .T. ) ;
#11810 = EDGE_CURVE ( 'NONE', #43432, #41850, #33914, .T. ) ;
#11811 = ORIENTED_EDGE ( 'NONE', *, *, #19868, .T. ) ;
#11812 = CARTESIAN_POINT ( 'NONE',  ( 72.27890028733797578, -1.750000000000009548, 161.8434138227750907 ) ) ;
#11813 = CARTESIAN_POINT ( 'NONE',  ( -6.695973446814940111, -1.750000000000023315, 160.8182875569279702 ) ) ;
#11814 = VERTEX_POINT ( 'NONE', #6957 ) ;
#11815 = CARTESIAN_POINT ( 'NONE',  ( -20.40054609052957701, 26.26366202847989229, -3.760136334089591248 ) ) ;
#11816 = PLANE ( 'NONE',  #43083 ) ;
#11817 = CARTESIAN_POINT ( 'NONE',  ( -27.33593271309441519, 41.94268121623345280, -9.367992836599951190 ) ) ;
#11818 = VERTEX_POINT ( 'NONE', #6206 ) ;
#11819 = EDGE_CURVE ( 'NONE', #36390, #24051, #20506, .T. ) ;
#11820 = DIRECTION ( 'NONE',  ( 0.000000000000000000, 0.000000000000000000, -1.000000000000000000 ) ) ;
#11821 = EDGE_CURVE ( 'NONE', #33571, #32944, #14008, .T. ) ;
#11822 = EDGE_CURVE ( 'NONE', #47056, #50485, #38286, .T. ) ;
#11823 = VECTOR ( 'NONE', #8695, 1000.000000000000000 ) ;
#11824 = ORIENTED_EDGE ( 'NONE', *, *, #19223, .F. ) ;
#11825 = CARTESIAN_POINT ( 'NONE',  ( 2.462075149652696027, -16.57295996686994499, 9.403735324607438884 ) ) ;
#11826 = DIRECTION ( 'NONE',  ( -0.000000000000000000, -0.000000000000000000, -1.000000000000000000 ) ) ;
#11827 = ORIENTED_EDGE ( 'NONE', *, *, #15312, .F. ) ;
#11828 = DIRECTION ( 'NONE',  ( 0.000000000000000000, -1.000000000000000000, 0.000000000000000000 ) ) ;
#11829 = LINE ( 'NONE', #4636, #38255 ) ;
#11830 = ORIENTED_EDGE ( 'NONE', *, *, #38137, .T. ) ;
#11831 = CARTESIAN_POINT ( 'NONE',  ( -1.011271242968683204, -0.7347315653655928092, 9.972675548442467175 ) ) ;
#11832 = CARTESIAN_POINT ( 'NONE',  ( -16.26331699892973148, -3.800463913881070077, -9.458680755252684591 ) ) ;
#11833 = CARTESIAN_POINT ( 'NONE',  ( 343.9999999999999432, -181.0000000000001421, -349.9999999999998863 ) ) ;
#11834 = CARTESIAN_POINT ( 'NONE',  ( 73.30402655318508209, -1.750000000000010658, -79.18171244307201562 ) ) ;
#11835 = EDGE_CURVE ( 'NONE', #44684, #29600, #17022, .T. ) ;
#11836 = ORIENTED_EDGE ( 'NONE', *, *, #29635, .T. ) ;
#11837 = AXIS2_PLACEMENT_3D ( 'NONE', #45600, #10720, #37693 ) ;
#11838 = DIRECTION ( 'NONE',  ( -1.000000000000000000, -0.000000000000000000, -0.000000000000000000 ) ) ;
#11839 = CARTESIAN_POINT ( 'NONE',  ( 356.0000000000002274, 185.0000000000000284, -360.0000000000002274 ) ) ;
#11840 = AXIS2_PLACEMENT_3D ( 'NONE', #19294, #10839, #34210 ) ;
#11841 = CARTESIAN_POINT ( 'NONE',  ( 75.05402655318509630, 1.025126265847089657, 79.06828755692797017 ) ) ;
#11842 = VERTEX_POINT ( 'NONE', #14908 ) ;
#11843 = CIRCLE ( 'NONE', #16742, 10.00000000000000000 ) ;
#11844 = ORIENTED_EDGE ( 'NONE', *, *, #19842, .F. ) ;
#11845 = CARTESIAN_POINT ( 'NONE',  ( -86.69597344681496054, 0.000000000000000000, -165.0000000000000000 ) ) ;
#11846 = CARTESIAN_POINT ( 'NONE',  ( 1.721971274562253740, 0.09408549481334846365, 9.928159647716247704 ) ) ;
#11847 = CARTESIAN_POINT ( 'NONE',  ( 85.00000000000029843, 17.00000000000000000, -84.99999999999998579 ) ) ;
#11848 = CARTESIAN_POINT ( 'NONE',  ( -64.99999999999877787, 16.00000000000000000, 5.000000000000004441 ) ) ;
#11849 =( BOUNDED_CURVE ( )  B_SPLINE_CURVE ( 3, ( #35208, #7744, #39301, #34697 ),
 .UNSPECIFIED., .F., .F. ) 
 B_SPLINE_CURVE_WITH_KNOTS ( ( 4, 4 ),
 ( 4.712388980384689674, 6.283185307179586232 ),
 .UNSPECIFIED. ) 
 CURVE ( )  GEOMETRIC_REPRESENTATION_ITEM ( )  RATIONAL_B_SPLINE_CURVE ( ( 1.000000000000000000, 0.8047378541243649375, 0.8047378541243649375, 1.000000000000000000 ) ) 
 REPRESENTATION_ITEM ( '' )  );
#11850 = DIRECTION ( 'NONE',  ( 1.000000000000000000, 0.000000000000000000, 0.000000000000000000 ) ) ;
#11851 = ORIENTED_EDGE ( 'NONE', *, *, #5106, .F. ) ;
#11852 = CARTESIAN_POINT ( 'NONE',  ( 32.36066692128250821, -7.813306791042813337, 3.199614146704519602 ) ) ;
#11853 = CARTESIAN_POINT ( 'NONE',  ( 14.49999999999999822, 12.98684210526315752, 19.87312575500900280 ) ) ;
#11854 = CARTESIAN_POINT ( 'NONE',  ( 181.0000000000000000, -95.49999999999998579, -350.0000000000001705 ) ) ;
#11855 = ORIENTED_EDGE ( 'NONE', *, *, #16786, .F. ) ;
#11856 = CIRCLE ( 'NONE', #48678, 1.750000000000001554 ) ;
#11857 = DIRECTION ( 'NONE',  ( 1.000000000000000000, 0.000000000000000000, -0.000000000000000000 ) ) ;
#11858 = EDGE_LOOP ( 'NONE', ( #27871, #26653, #48685, #31166, #11012, #843, #11337, #22832 ) ) ;
#11859 = CARTESIAN_POINT ( 'NONE',  ( -9.998889670239194061, -0.1490146381531308739, 9.282506307616474217 ) ) ;
#11860 = VECTOR ( 'NONE', #50207, 1000.000000000000000 ) ;
#11861 = ORIENTED_EDGE ( 'NONE', *, *, #39399, .T. ) ;
#11862 = DIRECTION ( 'NONE',  ( 0.000000000000000000, -2.265761274745217480E-16, 1.000000000000000000 ) ) ;
#11863 = CARTESIAN_POINT ( 'NONE',  ( 15.73090589902275482, 29.60029367929053024, 1.847720168420772691 ) ) ;
#11864 = CARTESIAN_POINT ( 'NONE',  ( 80.00000000000122213, 16.00000000000000000, 30.00000000000000000 ) ) ;
#11865 = ORIENTED_EDGE ( 'NONE', *, *, #47561, .F. ) ;
#11866 = ADVANCED_FACE ( 'NONE', ( #25966 ), #29543, .F. ) ;
#11867 = CARTESIAN_POINT ( 'NONE',  ( 0.000000000000000000, 17.00000000000000000, 0.000000000000000000 ) ) ;
#11868 = EDGE_CURVE ( 'NONE', #40379, #43927, #49172, .T. ) ;
#11869 = CARTESIAN_POINT ( 'NONE',  ( -31.44259251615275019, -38.95901822126145220, -9.367992836599951190 ) ) ;
#11870 = VERTEX_POINT ( 'NONE', #49246 ) ;
#11871 = CARTESIAN_POINT ( 'NONE',  ( 432.7825420346616170, -112.5000000000000000, -9.999999999999973355 ) ) ;
#11872 = AXIS2_PLACEMENT_3D ( 'NONE', #36583, #8602, #16550 ) ;
#11873 = CARTESIAN_POINT ( 'NONE',  ( -165.0000000000000284, 16.00000000000000000, -114.9999999999999858 ) ) ;
#11874 = LINE ( 'NONE', #19046, #42604 ) ;
#11875 = CARTESIAN_POINT ( 'NONE',  ( -204.9459734468149463, 2.143131898507880377E-16, -0.9317124430720247208 ) ) ;
#11876 = ORIENTED_EDGE ( 'NONE', *, *, #31746, .T. ) ;
#11877 = ADVANCED_FACE ( 'NONE', ( #39282 ), #39540, .F. ) ;
#11878 = ORIENTED_EDGE ( 'NONE', *, *, #47402, .F. ) ;
#11879 = FACE_OUTER_BOUND ( 'NONE', #13245, .T. ) ;
#11880 = VECTOR ( 'NONE', #419, 1000.000000000000000 ) ;
#11881 = EDGE_CURVE ( 'NONE', #26878, #41657, #26958, .T. ) ;
#11882 = EDGE_CURVE ( 'NONE', #39413, #1790, #23618, .T. ) ;
#11883 = ORIENTED_EDGE ( 'NONE', *, *, #10175, .T. ) ;
#11884 = CARTESIAN_POINT ( 'NONE',  ( -164.9459734468149463, 2.143131898507880377E-16, 39.06828755692798438 ) ) ;
#11885 = CARTESIAN_POINT ( 'NONE',  ( 31.55402655318503236, 0.000000000000000000, 165.0000000000000000 ) ) ;
#11886 =( BOUNDED_CURVE ( )  B_SPLINE_CURVE ( 3, ( #39117, #11141, #15249, #14726 ),
 .UNSPECIFIED., .F., .F. ) 
 B_SPLINE_CURVE_WITH_KNOTS ( ( 4, 4 ),
 ( 1.570796326794896558, 3.141592653589793116 ),
 .UNSPECIFIED. ) 
 CURVE ( )  GEOMETRIC_REPRESENTATION_ITEM ( )  RATIONAL_B_SPLINE_CURVE ( ( 1.000000000000000000, 0.8047378541243649375, 0.8047378541243649375, 1.000000000000000000 ) ) 
 REPRESENTATION_ITEM ( '' )  );
#11887 = ORIENTED_EDGE ( 'NONE', *, *, #4642, .T. ) ;
#11888 = CARTESIAN_POINT ( 'NONE',  ( -25.60949810002096783, -43.19700938445173932, 1.847720168420772691 ) ) ;
#11889 = EDGE_LOOP ( 'NONE', ( #48669, #17921, #3906, #28103, #8555, #6966 ) ) ;
#11890 = EDGE_CURVE ( 'NONE', #34485, #14566, #20621, .T. ) ;
#11891 = DIRECTION ( 'NONE',  ( -1.000000000000000000, 0.000000000000000000, -1.612977847700450206E-50 ) ) ;
#11892 = CARTESIAN_POINT ( 'NONE',  ( -114.9999999999997158, 17.00000000000000000, -84.99999999999998579 ) ) ;
#11893 = CARTESIAN_POINT ( 'NONE',  ( 2.499999999999945377, -224.9999999999999716, -240.0000000000000000 ) ) ;
#11894 = VECTOR ( 'NONE', #47851, 1000.000000000000000 ) ;
#11895 = ORIENTED_EDGE ( 'NONE', *, *, #7214, .T. ) ;
#11896 = ORIENTED_EDGE ( 'NONE', *, *, #35080, .F. ) ;
#11897 = ORIENTED_EDGE ( 'NONE', *, *, #15854, .T. ) ;
#11898 = CIRCLE ( 'NONE', #36487, 1.750000000000015543 ) ;
#11899 = DIRECTION ( 'NONE',  ( 0.000000000000000000, 0.000000000000000000, 1.000000000000000000 ) ) ;
#11900 = CARTESIAN_POINT ( 'NONE',  ( 357.1715728752537871, 183.0000000000000000, -358.0000000000001705 ) ) ;
#11901 = CARTESIAN_POINT ( 'NONE',  ( 0.1265591857323814795, 1.213367045380162823, 9.963925895596176474 ) ) ;
#11902 = ORIENTED_EDGE ( 'NONE', *, *, #10646, .T. ) ;
#11903 = CARTESIAN_POINT ( 'NONE',  ( -14.99999999999782041, 17.00000000000000000, 95.00000000000000000 ) ) ;
#11904 = ORIENTED_EDGE ( 'NONE', *, *, #19967, .F. ) ;
#11905 = FACE_OUTER_BOUND ( 'NONE', #34844, .T. ) ;
#11906 = EDGE_LOOP ( 'NONE', ( #31769, #27455, #15439, #8808, #15851 ) ) ;
#11907 = DIRECTION ( 'NONE',  ( 0.000000000000000000, -1.000000000000000000, 0.000000000000000000 ) ) ;
#11908 = CARTESIAN_POINT ( 'NONE',  ( -48.44597344681496054, -1.025126265847089879, 82.56828755692798438 ) ) ;
#11909 = AXIS2_PLACEMENT_3D ( 'NONE', #16765, #32424, #48018 ) ;
#11910 = FACE_OUTER_BOUND ( 'NONE', #21833, .T. ) ;
#11911 = CARTESIAN_POINT ( 'NONE',  ( -165.3973046169136012, -98.56198943095992604, -17.65743994998277699 ) ) ;
#11912 = VECTOR ( 'NONE', #4793, 1000.000000000000000 ) ;
#11913 = DIRECTION ( 'NONE',  ( -1.132880637372608740E-16, -4.718402560806925739E-50, -1.000000000000000000 ) ) ;
#11914 = CARTESIAN_POINT ( 'NONE',  ( 0.3370904143228924954, 0.2449105217885333141, 10.00000000000000000 ) ) ;
#11915 = ORIENTED_EDGE ( 'NONE', *, *, #11371, .F. ) ;
#11916 = ORIENTED_EDGE ( 'NONE', *, *, #35597, .F. ) ;
#11917 = CARTESIAN_POINT ( 'NONE',  ( 5.551115123125782702E-14, -168.9999999999999432, 357.9999999999997726 ) ) ;
#11918 = PRODUCT_DEFINITION_FORMATION_WITH_SPECIFIED_SOURCE ( 'ANY', '', #49848, .NOT_KNOWN. ) ;
#11919 = PLANE ( 'NONE',  #40061 ) ;
#11920 = CARTESIAN_POINT ( 'NONE',  ( -9.760995290733800900, 2.173239732351794462, 9.646707543097347681 ) ) ;
#11921 = VECTOR ( 'NONE', #29560, 1000.000000000000000 ) ;
#11922 = EDGE_CURVE ( 'NONE', #39269, #13970, #35445, .T. ) ;
#11923 = FACE_OUTER_BOUND ( 'NONE', #23963, .T. ) ;
#11924 = CARTESIAN_POINT ( 'NONE',  ( 154.1026953830863420, 70.03596893647589638, -94.69675437945477370 ) ) ;
#11925 = VERTEX_POINT ( 'NONE', #18995 ) ;
#11926 = CARTESIAN_POINT ( 'NONE',  ( -0.2455008416098019286, -1.553107091521327865, 9.945241992664895392 ) ) ;
#11927 = DIRECTION ( 'NONE',  ( 0.000000000000000000, 0.000000000000000000, 1.000000000000000000 ) ) ;
#11928 = ORIENTED_EDGE ( 'NONE', *, *, #6175, .F. ) ;
#11929 = AXIS2_PLACEMENT_3D ( 'NONE', #15714, #46977, #43172 ) ;
#11930 = DIRECTION ( 'NONE',  ( 0.000000000000000000, 0.000000000000000000, 1.000000000000000000 ) ) ;
#11931 = VECTOR ( 'NONE', #42567, 1000.000000000000000 ) ;
#11932 = LINE ( 'NONE', #23983, #25371 ) ;
#11933 = CARTESIAN_POINT ( 'NONE',  ( 5.880995097349652312, 0.9650023149932013267, 5.692061405548898279E-16 ) ) ;
#11934 = B_SPLINE_CURVE_WITH_KNOTS ( 'NONE', 3,
 ( #238, #15877, #19969, #12273 ),
 .UNSPECIFIED., .F., .F.,
 ( 4, 4 ),
 ( 0.9895749839358302102, 1.000000000000000000 ),
 .UNSPECIFIED. ) ;
#11935 = VECTOR ( 'NONE', #10333, 1000.000000000000000 ) ;
#11936 = ORIENTED_EDGE ( 'NONE', *, *, #33042, .F. ) ;
#11937 = ORIENTED_EDGE ( 'NONE', *, *, #16528, .T. ) ;
#11938 = CARTESIAN_POINT ( 'NONE',  ( -177.4999999999999716, 57.49999999999996447, -130.5992382549688671 ) ) ;
#11939 = CARTESIAN_POINT ( 'NONE',  ( -1.249999999999999778, 0.000000000000000000, 10.00000000000000000 ) ) ;
#11940 =( BOUNDED_CURVE ( )  B_SPLINE_CURVE ( 3, ( #46301, #6834, #6580, #21975 ),
 .UNSPECIFIED., .F., .F. ) 
 B_SPLINE_CURVE_WITH_KNOTS ( ( 4, 4 ),
 ( 1.570796326794896558, 3.141592653589793116 ),
 .UNSPECIFIED. ) 
 CURVE ( )  GEOMETRIC_REPRESENTATION_ITEM ( )  RATIONAL_B_SPLINE_CURVE ( ( 1.000000000000000000, 0.8047378541243649375, 0.8047378541243649375, 1.000000000000000000 ) ) 
 REPRESENTATION_ITEM ( '' )  );
#11941 = COLOUR_RGB ( '',0.7921568627450980005, 0.8196078431372548767, 0.9333333333333333481 ) ;
#11942 = ORIENTED_EDGE ( 'NONE', *, *, #31827, .F. ) ;
#11943 = ORIENTED_EDGE ( 'NONE', *, *, #41215, .T. ) ;
#11944 = CARTESIAN_POINT ( 'NONE',  ( -125.6708471809678542, -1.749999999999996891, 39.79316129108089228 ) ) ;
#11945 = CARTESIAN_POINT ( 'NONE',  ( 0.3370904143228924954, 0.2449105217885333141, 10.00000000000000000 ) ) ;
#11946 = DIRECTION ( 'NONE',  ( -1.000000000000000000, 0.000000000000000000, 0.000000000000000000 ) ) ;
#11947 = CARTESIAN_POINT ( 'NONE',  ( -22.82242230425432439, -2.816136035261162185, 230.0000000000000000 ) ) ;
#11948 = CIRCLE ( 'NONE', #6190, 4.000000000000003553 ) ;
#11949 = VERTEX_POINT ( 'NONE', #19248 ) ;
#11950 = ORIENTED_EDGE ( 'NONE', *, *, #17102, .F. ) ;
#11951 = ADVANCED_FACE ( 'NONE', ( #31596 ), #12080, .T. ) ;
#11952 = ORIENTED_EDGE ( 'NONE', *, *, #1438, .F. ) ;
#11953 =( BOUNDED_CURVE ( )  B_SPLINE_CURVE ( 3, ( #12777, #48383, #36407, #35897 ),
 .UNSPECIFIED., .F., .F. ) 
 B_SPLINE_CURVE_WITH_KNOTS ( ( 4, 4 ),
 ( 1.570796326794896558, 3.141592653589793116 ),
 .UNSPECIFIED. ) 
 CURVE ( )  GEOMETRIC_REPRESENTATION_ITEM ( )  RATIONAL_B_SPLINE_CURVE ( ( 1.000000000000000000, 0.8047378541243649375, 0.8047378541243649375, 1.000000000000000000 ) ) 
 REPRESENTATION_ITEM ( '' )  );
#11954 = VECTOR ( 'NONE', #19664, 1000.000000000000000 ) ;
#11955 = CARTESIAN_POINT ( 'NONE',  ( -0.3862712429686809279, -1.188820645368943163, 10.00000000000000000 ) ) ;
#11956 = ORIENTED_EDGE ( 'NONE', *, *, #7420, .F. ) ;
#11957 = DIRECTION ( 'NONE',  ( 0.000000000000000000, 0.000000000000000000, 1.000000000000000000 ) ) ;
#11958 = CARTESIAN_POINT ( 'NONE',  ( 115.0540265531850395, 2.143131898507847836E-16, -40.93171244307202983 ) ) ;
#11959 = FACE_OUTER_BOUND ( 'NONE', #4796, .T. ) ;
#11960 = ORIENTED_EDGE ( 'NONE', *, *, #25215, .F. ) ;
#11961 = ORIENTED_EDGE ( 'NONE', *, *, #39339, .T. ) ;
#11962 = CARTESIAN_POINT ( 'NONE',  ( 214.9999999999999432, 164.9999999999999716, 372.0000000000000000 ) ) ;
#11963 = CARTESIAN_POINT ( 'NONE',  ( -206.6959734468149463, 1.750000000000009992, 160.8182875569279702 ) ) ;
#11964 = DIRECTION ( 'NONE',  ( 0.000000000000000000, 0.000000000000000000, 1.000000000000000000 ) ) ;
#11965 = VERTEX_POINT ( 'NONE', #46924 ) ;
#11966 = ORIENTED_EDGE ( 'NONE', *, *, #15701, .T. ) ;
#11967 = CARTESIAN_POINT ( 'NONE',  ( 15.44803555374680393, 6.237487519713364570, -3.546734833711462365 ) ) ;
#11968 = DIRECTION ( 'NONE',  ( -1.000000000000000000, 0.000000000000000000, 0.000000000000000000 ) ) ;
#11969 = ORIENTED_EDGE ( 'NONE', *, *, #9883, .T. ) ;
#11970 = VECTOR ( 'NONE', #3852, 1000.000000000000000 ) ;
#11971 = DIRECTION ( 'NONE',  ( -0.000000000000000000, -0.000000000000000000, -1.000000000000000000 ) ) ;
#11972 = DIRECTION ( 'NONE',  ( -1.000000000000000000, 0.000000000000000000, 0.000000000000000000 ) ) ;
#11973 = CARTESIAN_POINT ( 'NONE',  ( -64.99999999999783995, 17.00000000000000000, 115.0000000000000142 ) ) ;
#11974 = CARTESIAN_POINT ( 'NONE',  ( 35.05402655318504657, 2.143131898507880377E-16, 165.0000000000000000 ) ) ;
#11975 = AXIS2_PLACEMENT_3D ( 'NONE', #26024, #17308, #21920 ) ;
#11976 = EDGE_LOOP ( 'NONE', ( #8832, #50636, #31082, #21291 ) ) ;
#11977 = FACE_OUTER_BOUND ( 'NONE', #35206, .T. ) ;
#11978 = CARTESIAN_POINT ( 'NONE',  ( 349.9999999999999432, -168.9999999999999432, 357.9999999999997726 ) ) ;
#11979 = ADVANCED_FACE ( 'NONE', ( #7983 ), #43358, .F. ) ;
#11980 = CARTESIAN_POINT ( 'NONE',  ( -4.999999999999997335, 204.9999999999999716, -230.2499999999999716 ) ) ;
#11981 = VECTOR ( 'NONE', #41470, 1000.000000000000000 ) ;
#11982 = AXIS2_PLACEMENT_3D ( 'NONE', #19512, #8500, #32095 ) ;
#11983 = CARTESIAN_POINT ( 'NONE',  ( 0.000000000000000000, 165.0000000000000000, 355.9999999999997726 ) ) ;
#11984 = CARTESIAN_POINT ( 'NONE',  ( -16.76006782980216059, 2.050259795448645228, 9.178419661560148768 ) ) ;
#11985 = DIRECTION ( 'NONE',  ( 0.1671032855531390526, -0.5142910309547716885, -0.8411784753765542133 ) ) ;
#11986 = AXIS2_PLACEMENT_3D ( 'NONE', #537, #46420, #23610 ) ;
#11987 = EDGE_LOOP ( 'NONE', ( #23294, #24631, #43234, #31912 ) ) ;
#11988 = LINE ( 'NONE', #31753, #42045 ) ;
#11989 = CARTESIAN_POINT ( 'NONE',  ( -69.99999999999847944, 17.00000000000000000, 35.00000000000000000 ) ) ;
#11990 = ORIENTED_EDGE ( 'NONE', *, *, #41822, .F. ) ;
#11991 = CARTESIAN_POINT ( 'NONE',  ( 155.0540265531850537, 2.143131898507880377E-16, -40.93171244307202983 ) ) ;
#11992 = CARTESIAN_POINT ( 'NONE',  ( 0.000000000000000000, 0.000000000000000000, 0.000000000000000000 ) ) ;
#11993 = CARTESIAN_POINT ( 'NONE',  ( -84.94597344681494633, 2.143131898507880377E-16, 82.56828755692798438 ) ) ;
#11994 = ORIENTED_EDGE ( 'NONE', *, *, #17078, .T. ) ;
#11995 = DIRECTION ( 'NONE',  ( -0.000000000000000000, -0.000000000000000000, -1.000000000000000000 ) ) ;
#11996 = VERTEX_POINT ( 'NONE', #43119 ) ;
#11997 = VERTEX_POINT ( 'NONE', #20019 ) ;
#11998 = CARTESIAN_POINT ( 'NONE',  ( 15.00099850811936264, 7.462898891544210933, 9.403735324607438884 ) ) ;
#11999 = FACE_OUTER_BOUND ( 'NONE', #44225, .T. ) ;
#12000 = VECTOR ( 'NONE', #34742, 1000.000000000000000 ) ;
#12001 = CIRCLE ( 'NONE', #47988, 1.750000000000015543 ) ;
#12002 = ORIENTED_EDGE ( 'NONE', *, *, #33824, .T. ) ;
#12003 = LINE ( 'NONE', #31007, #32802 ) ;
#12004 = CARTESIAN_POINT ( 'NONE',  ( -48.44597344681495343, 0.000000000000000000, -40.93171244307205825 ) ) ;
#12005 = AXIS2_PLACEMENT_3D ( 'NONE', #25454, #6211, #5438 ) ;
#12006 = ADVANCED_FACE ( 'NONE', ( #3865 ), #42597, .F. ) ;
#12007 = CARTESIAN_POINT ( 'NONE',  ( -19.99999999999971223, 16.00000000000000000, -60.00000000000000000 ) ) ;
#12008 = ORIENTED_EDGE ( 'NONE', *, *, #17207, .F. ) ;
#12009 = CARTESIAN_POINT ( 'NONE',  ( 185.0000000000000000, -5.999999999999950262, -340.0000000000001137 ) ) ;
#12010 = DIRECTION ( 'NONE',  ( -1.000000000000000000, -0.000000000000000000, -0.000000000000000000 ) ) ;
#12011 = CARTESIAN_POINT ( 'NONE',  ( 169.0000000000000000, -174.9999999999999716, -113.0000000000001563 ) ) ;
#12012 = AXIS2_PLACEMENT_3D ( 'NONE', #12319, #50513, #784 ) ;
#12013 = ORIENTED_EDGE ( 'NONE', *, *, #14300, .F. ) ;
#12014 = DIRECTION ( 'NONE',  ( -0.000000000000000000, -0.000000000000000000, -1.000000000000000000 ) ) ;
#12015 = DIRECTION ( 'NONE',  ( -1.586032880504786307E-16, 1.654361225106055350E-24, -1.000000000000000000 ) ) ;
#12016 = ORIENTED_EDGE ( 'NONE', *, *, #42133, .T. ) ;
#12017 = VECTOR ( 'NONE', #47379, 1000.000000000000000 ) ;
#12018 = ORIENTED_EDGE ( 'NONE', *, *, #49620, .F. ) ;
#12019 = ORIENTED_EDGE ( 'NONE', *, *, #26616, .F. ) ;
#12020 = CARTESIAN_POINT ( 'NONE',  ( 75.05402655318509630, 2.143131898507880377E-16, -37.43171244307200141 ) ) ;
#12021 = ADVANCED_FACE ( 'NONE', ( #34943 ), #42851, .F. ) ;
#12022 = ADVANCED_FACE ( 'NONE', ( #27975 ), #12317, .F. ) ;
#12023 = DIRECTION ( 'NONE',  ( 1.000000000000000000, 0.000000000000000000, 0.000000000000000000 ) ) ;
#12024 = ORIENTED_EDGE ( 'NONE', *, *, #48200, .F. ) ;
#12025 = AXIS2_PLACEMENT_3D ( 'NONE', #18799, #34483, #50061 ) ;
#12026 = CARTESIAN_POINT ( 'NONE',  ( -1.066995270233474624, 50.00000000000000711, -3.760136334089591248 ) ) ;
#12027 = PLANE ( 'NONE',  #3302 ) ;
#12028 = EDGE_CURVE ( 'NONE', #8778, #39465, #31122, .T. ) ;
#12029 = CARTESIAN_POINT ( 'NONE',  ( -29.18392875402943432, -17.44843138996582965, 7.906207997025717304 ) ) ;
#12030 = CARTESIAN_POINT ( 'NONE',  ( 31.55402655318503236, -1.025126265847089657, -80.93171244307201562 ) ) ;
#12031 = CARTESIAN_POINT ( 'NONE',  ( -86.69597344681494633, -1.750000000000009992, 160.8182875569279702 ) ) ;
#12032 = CARTESIAN_POINT ( 'NONE',  ( 7.576114424932982594, -33.14742743729794938, 7.906207997025717304 ) ) ;
#12033 = DIRECTION ( 'NONE',  ( -0.000000000000000000, 1.000000000000000000, 0.000000000000000000 ) ) ;
#12034 = FACE_OUTER_BOUND ( 'NONE', #25325, .T. ) ;
#12035 = CARTESIAN_POINT ( 'NONE',  ( 192.2789002873380184, 1.750000000000009548, -38.15658617722494483 ) ) ;
#12036 = DIRECTION ( 'NONE',  ( -1.000000000000000000, 0.000000000000000000, 0.000000000000000000 ) ) ;
#12037 = EDGE_CURVE ( 'NONE', #339, #2423, #27887, .T. ) ;
#12038 = CARTESIAN_POINT ( 'NONE',  ( -46.69597344681494633, -1.750000000000009992, 160.8182875569279702 ) ) ;
#12039 = ADVANCED_FACE ( 'NONE', ( #46427 ), #38779, .T. ) ;
#12040 = CARTESIAN_POINT ( 'NONE',  ( -205.6708471809678827, -1.750000000000009548, -118.1565861772249519 ) ) ;
#12041 = CARTESIAN_POINT ( 'NONE',  ( 181.0000000000000000, -184.9999999999999716, -350.0000000000001705 ) ) ;
#12042 = EDGE_CURVE ( 'NONE', #4637, #38939, #11573, .T. ) ;
#12043 = EDGE_CURVE ( 'NONE', #29675, #32627, #4634, .T. ) ;
#12044 = SPHERICAL_SURFACE ( 'NONE', #16696, 0.5000000000000000000 ) ;
#12045 = ORIENTED_EDGE ( 'NONE', *, *, #35975, .T. ) ;
#12046 = FACE_OUTER_BOUND ( 'NONE', #2204, .T. ) ;
#12047 = EDGE_CURVE ( 'NONE', #25327, #16502, #36196, .T. ) ;
#12048 = CARTESIAN_POINT ( 'NONE',  ( -44.99506233596265048, -23.32283626942287569, 7.455576670931136185 ) ) ;
#12049 = DIRECTION ( 'NONE',  ( 1.000000000000000000, 0.000000000000000000, -0.000000000000000000 ) ) ;
#12050 = CARTESIAN_POINT ( 'NONE',  ( 33.30402655318503946, 1.750000000000010658, -79.18171244307201562 ) ) ;
#12051 = VERTEX_POINT ( 'NONE', #24889 ) ;
#12052 = CYLINDRICAL_SURFACE ( 'NONE', #15789, 1.750000000000001554 ) ;
#12053 = ORIENTED_EDGE ( 'NONE', *, *, #19288, .F. ) ;
#12054 = CARTESIAN_POINT ( 'NONE',  ( -194.9999999999999432, 0.000000000000000000, 0.000000000000000000 ) ) ;
#12055 = ORIENTED_EDGE ( 'NONE', *, *, #43931, .F. ) ;
#12056 = LINE ( 'NONE', #8, #2498 ) ;
#12057 = CARTESIAN_POINT ( 'NONE',  ( 210.0000000000000568, 0.000000000000000000, 0.8182875569279768335 ) ) ;
#12058 = ORIENTED_EDGE ( 'NONE', *, *, #4186, .F. ) ;
#12059 = EDGE_CURVE ( 'NONE', #2268, #36390, #31525, .T. ) ;
#12060 = ORIENTED_EDGE ( 'NONE', *, *, #15503, .T. ) ;
#12061 = VECTOR ( 'NONE', #31135, 1000.000000000000000 ) ;
#12062 = EDGE_CURVE ( 'NONE', #12549, #38939, #38015, .T. ) ;
#12063 = EDGE_CURVE ( 'NONE', #24745, #15166, #20773, .T. ) ;
#12064 = EDGE_LOOP ( 'NONE', ( #38247, #45848, #34785, #1752 ) ) ;
#12065 = CARTESIAN_POINT ( 'NONE',  ( 164.9999999999999716, -174.9999999999999716, -356.0000000000001705 ) ) ;
#12066 = CARTESIAN_POINT ( 'NONE',  ( -204.9459734468149463, 2.143131898507880377E-16, 39.06828755692798438 ) ) ;
#12067 = ORIENTED_EDGE ( 'NONE', *, *, #41213, .T. ) ;
#12068 = DIRECTION ( 'NONE',  ( 0.000000000000000000, 0.000000000000000000, -1.000000000000000000 ) ) ;
#12069 = CARTESIAN_POINT ( 'NONE',  ( 38.83486119589591112, -15.16159403945135153, -9.387872844313825738 ) ) ;
#12070 = EDGE_CURVE ( 'NONE', #1878, #20271, #28237, .T. ) ;
#12071 = CARTESIAN_POINT ( 'NONE',  ( 0.000000000000000000, 0.000000000000000000, 0.000000000000000000 ) ) ;
#12072 = PLANE ( 'NONE',  #11986 ) ;
#12073 = EDGE_CURVE ( 'NONE', #17197, #13383, #43239, .T. ) ;
#12074 = CARTESIAN_POINT ( 'NONE',  ( 7.216980890441427654, -6.922079660550236824, 0.000000000000000000 ) ) ;
#12075 = ORIENTED_EDGE ( 'NONE', *, *, #1922, .F. ) ;
#12076 = VECTOR ( 'NONE', #19965, 1000.000000000000000 ) ;
#12077 = LINE ( 'NONE', #27722, #50439 ) ;
#12078 = DIRECTION ( 'NONE',  ( 1.000000000000000000, 0.000000000000000000, 0.000000000000000000 ) ) ;
#12079 = VERTEX_POINT ( 'NONE', #44855 ) ;
#12080 = CYLINDRICAL_SURFACE ( 'NONE', #1641, 1.750000000000008438 ) ;
#12081 = CARTESIAN_POINT ( 'NONE',  ( 26.76431201374280278, -26.27596734087696362, 8.506357886886739550 ) ) ;
#12082 = ORIENTED_EDGE ( 'NONE', *, *, #48867, .F. ) ;
#12083 = PLANE ( 'NONE',  #22647 ) ;
#12084 = DIRECTION ( 'NONE',  ( -0.000000000000000000, -0.000000000000000000, -1.000000000000000000 ) ) ;
#12085 = CARTESIAN_POINT ( 'NONE',  ( 151.5540265531850537, 0.000000000000000000, -157.4317124430720582 ) ) ;
#12086 =( BOUNDED_CURVE ( )  B_SPLINE_CURVE ( 3, ( #39571, #39076, #30862, #46453 ),
 .UNSPECIFIED., .F., .F. ) 
 B_SPLINE_CURVE_WITH_KNOTS ( ( 4, 4 ),
 ( 4.712388980384689674, 6.283185307179586232 ),
 .UNSPECIFIED. ) 
 CURVE ( )  GEOMETRIC_REPRESENTATION_ITEM ( )  RATIONAL_B_SPLINE_CURVE ( ( 1.000000000000000000, 0.8047378541243649375, 0.8047378541243649375, 1.000000000000000000 ) ) 
 REPRESENTATION_ITEM ( '' )  );
#12087 = CARTESIAN_POINT ( 'NONE',  ( 193.3040265531851105, 1.750000000000010214, 40.81828755692798438 ) ) ;
#12088 = ORIENTED_EDGE ( 'NONE', *, *, #29294, .T. ) ;
#12089 = ADVANCED_FACE ( 'NONE', ( #32086 ), #5378, .T. ) ;
#12090 = CYLINDRICAL_SURFACE ( 'NONE', #36820, 1.750000000000015543 ) ;
#12091 = PLANE ( 'NONE',  #12779 ) ;
#12092 =( BOUNDED_CURVE ( )  B_SPLINE_CURVE ( 3, ( #4148, #54, #47456, #20297 ),
 .UNSPECIFIED., .F., .F. ) 
 B_SPLINE_CURVE_WITH_KNOTS ( ( 4, 4 ),
 ( 1.570796326794896558, 3.141592653589793116 ),
 .UNSPECIFIED. ) 
 CURVE ( )  GEOMETRIC_REPRESENTATION_ITEM ( )  RATIONAL_B_SPLINE_CURVE ( ( 1.000000000000000000, 0.8047378541243649375, 0.8047378541243649375, 1.000000000000000000 ) ) 
 REPRESENTATION_ITEM ( '' )  );
#12094 = B_SPLINE_CURVE_WITH_KNOTS ( 'NONE', 3,
 ( #23133, #20302, #15693, #39567 ),
 .UNSPECIFIED., .F., .F.,
 ( 4, 4 ),
 ( 0.9688112071879413367, 0.9724175925769218409 ),
 .UNSPECIFIED. ) ;
#12093 = CARTESIAN_POINT ( 'NONE',  ( 15.00000000000000000, 0.000000000000000000, 0.000000000000000000 ) ) ;
#12095 = ORIENTED_EDGE ( 'NONE', *, *, #30895, .T. ) ;
#12096 = ORIENTED_EDGE ( 'NONE', *, *, #44586, .T. ) ;
#12097 = DIRECTION ( 'NONE',  ( 1.000000000000000000, -1.060262988517032700E-14, -1.744802545150791203E-14 ) ) ;
#12098 = LINE ( 'NONE', #44376, #14662 ) ;
#12099 = CARTESIAN_POINT ( 'NONE',  ( 183.0000000000000568, 175.0000000000000284, 343.9999999999998863 ) ) ;
#12100 = EDGE_CURVE ( 'NONE', #24711, #17183, #29241, .T. ) ;
#12101 = EDGE_CURVE ( 'NONE', #2507, #36127, #44361, .T. ) ;
#12102 = CARTESIAN_POINT ( 'NONE',  ( -30.25247992116029394, 39.82368563463828792, -3.760136334089591248 ) ) ;
#12103 = DIRECTION ( 'NONE',  ( 0.000000000000000000, 2.537652627714642000E-15, 1.000000000000000000 ) ) ;
#12104 = ORIENTED_EDGE ( 'NONE', *, *, #6484, .T. ) ;
#12105 = EDGE_CURVE ( 'NONE', #28712, #35844, #43869, .T. ) ;
#12106 = DIRECTION ( 'NONE',  ( -1.000000000000000000, -0.000000000000000000, -0.000000000000000000 ) ) ;
#12107 = EDGE_CURVE ( 'NONE', #48410, #34818, #6535, .T. ) ;
#12108 =( BOUNDED_CURVE ( )  B_SPLINE_CURVE ( 3, ( #7225, #45930, #2846, #14412 ),
 .UNSPECIFIED., .F., .F. ) 
 B_SPLINE_CURVE_WITH_KNOTS ( ( 4, 4 ),
 ( 1.570796326794896558, 3.141592653589793116 ),
 .UNSPECIFIED. ) 
 CURVE ( )  GEOMETRIC_REPRESENTATION_ITEM ( )  RATIONAL_B_SPLINE_CURVE ( ( 1.000000000000000000, 0.8047378541243649375, 0.8047378541243649375, 1.000000000000000000 ) ) 
 REPRESENTATION_ITEM ( '' )  );
#12109 = CARTESIAN_POINT ( 'NONE',  ( -46.69597344681494633, -1.750000000000010214, 40.81828755692798438 ) ) ;
#12110 = CYLINDRICAL_SURFACE ( 'NONE', #42167, 1.750000000000010214 ) ;
#12111 = DIRECTION ( 'NONE',  ( -1.000000000000000000, 0.000000000000000000, 0.000000000000000000 ) ) ;
#12112 = EDGE_CURVE ( 'NONE', #19110, #11639, #5626, .T. ) ;
#12113 = ORIENTED_EDGE ( 'NONE', *, *, #29275, .T. ) ;
#12114 = DIRECTION ( 'NONE',  ( -1.654361225106055350E-24, -1.654361225106055350E-24, 1.000000000000000000 ) ) ;
#12115 = ORIENTED_EDGE ( 'NONE', *, *, #36525, .T. ) ;
#12116 = LINE ( 'NONE', #46705, #30266 ) ;
#12117 = ORIENTED_EDGE ( 'NONE', *, *, #38802, .F. ) ;
#12118 = CARTESIAN_POINT ( 'NONE',  ( -0.3370904143228963812, 0.2449105217885287067, 10.00000000000000000 ) ) ;
#12119 = CARTESIAN_POINT ( 'NONE',  ( -208.4459734468149463, 0.000000000000000000, 159.0682875569279702 ) ) ;
#12120 = CARTESIAN_POINT ( 'NONE',  ( -210.0000000000000568, 0.000000000000000000, -39.18171244307202983 ) ) ;
#12121 = LINE ( 'NONE', #47474, #32078 ) ;
#12122 = ORIENTED_EDGE ( 'NONE', *, *, #11580, .T. ) ;
#12123 = CARTESIAN_POINT ( 'NONE',  ( -165.6708471809677974, -1.750000000000010436, -80.20683870891910772 ) ) ;
#12124 = ADVANCED_FACE ( 'NONE', ( #32855 ), #9728, .T. ) ;
#12125 = CARTESIAN_POINT ( 'NONE',  ( 151.5540265531850537, 1.025126265847089435, -77.43171244307200141 ) ) ;
#12126 = ORIENTED_EDGE ( 'NONE', *, *, #39396, .T. ) ;
#12127 = DIRECTION ( 'NONE',  ( 0.000000000000000000, 0.2791762785758810650, -0.9602398687205827565 ) ) ;
#12128 = CARTESIAN_POINT ( 'NONE',  ( -2.210477865340801706, -37.43479381012853224, -9.422646554964178023 ) ) ;
#12129 = LINE ( 'NONE', #27774, #44250 ) ;
#12130 = DIRECTION ( 'NONE',  ( -1.000000000000000000, 0.000000000000000000, -0.000000000000000000 ) ) ;
#12131 = AXIS2_PLACEMENT_3D ( 'NONE', #37855, #34502, #41168 ) ;
#12132 = EDGE_LOOP ( 'NONE', ( #40590, #12113, #26433, #28424, #43043, #33286 ) ) ;
#12133 = ORIENTED_EDGE ( 'NONE', *, *, #3326, .T. ) ;
#12134 = LINE ( 'NONE', #8287, #17732 ) ;
#12135 = ORIENTED_EDGE ( 'NONE', *, *, #40276, .F. ) ;
#12136 = CARTESIAN_POINT ( 'NONE',  ( 192.2789002873380184, 1.750000000000009548, -78.15658617722490931 ) ) ;
#12137 = CARTESIAN_POINT ( 'NONE',  ( 135.0000000000019043, 17.00000000000000000, 90.00000000000000000 ) ) ;
#12138 = CARTESIAN_POINT ( 'NONE',  ( 210.0000000000000568, 0.000000000000000000, -159.1817124430720298 ) ) ;
#12139 = ORIENTED_EDGE ( 'NONE', *, *, #22804, .T. ) ;
#12140 = CARTESIAN_POINT ( 'NONE',  ( 181.0000000000000000, -272.5000000000000000, -98.99999999999990052 ) ) ;
#12141 = EDGE_LOOP ( 'NONE', ( #25897, #12580, #27329, #7209 ) ) ;
#12142 = ADVANCED_FACE ( 'NONE', ( #13324 ), #40043, .F. ) ;
#12143 = ORIENTED_EDGE ( 'NONE', *, *, #16124, .F. ) ;
#12144 = CARTESIAN_POINT ( 'NONE',  ( -8.176860274785726190, 5.756644512789648616, 9.282506307616472441 ) ) ;
#12145 = CARTESIAN_POINT ( 'NONE',  ( 183.0000000000000000, -164.9999999999999432, 343.9999999999998863 ) ) ;
#12146 = EDGE_LOOP ( 'NONE', ( #47141, #8661, #39195, #9095, #31528 ) ) ;
#12147 = CIRCLE ( 'NONE', #20341, 1.750000000000001554 ) ;
#12148 = ORIENTED_EDGE ( 'NONE', *, *, #6126, .F. ) ;
#12149 = EDGE_LOOP ( 'NONE', ( #47091, #30563, #25457, #30883 ) ) ;
#12150 = DIRECTION ( 'NONE',  ( 0.000000000000000000, 0.2981428420003837121, 0.9545212652235329776 ) ) ;
#12151 = DIRECTION ( 'NONE',  ( 0.000000000000000000, 5.664403186863042467E-17, 1.000000000000000000 ) ) ;
#12152 = ORIENTED_EDGE ( 'NONE', *, *, #20330, .T. ) ;
#12153 = CARTESIAN_POINT ( 'NONE',  ( 356.0000000000000000, 167.0000000000001990, -342.0000000000002842 ) ) ;
#12154 = ORIENTED_EDGE ( 'NONE', *, *, #49194, .F. ) ;
#12155 = ORIENTED_EDGE ( 'NONE', *, *, #24881, .T. ) ;
#12156 = DIRECTION ( 'NONE',  ( -1.586032892321651989E-16, 3.736034562988530447E-32, -1.000000000000000000 ) ) ;
#12157 = CARTESIAN_POINT ( 'NONE',  ( 0.000000000000000000, 181.0000000000000284, 343.9999999999997726 ) ) ;
#12158 = EDGE_CURVE ( 'NONE', #45326, #15741, #44109, .T. ) ;
#12159 = EDGE_CURVE ( 'NONE', #18070, #23819, #17437, .T. ) ;
#12160 = PLANE ( 'NONE',  #4536 ) ;
#12161 = CARTESIAN_POINT ( 'NONE',  ( 33.30402655318503946, 0.000000000000000000, 165.0000000000000000 ) ) ;
#12162 = LINE ( 'NONE', #624, #7595 ) ;
#12163 = ORIENTED_EDGE ( 'NONE', *, *, #45596, .T. ) ;
#12164 = VERTEX_POINT ( 'NONE', #10246 ) ;
#12165 = CARTESIAN_POINT ( 'NONE',  ( -204.9459734468149463, 2.143131898507880377E-16, 159.0682875569279702 ) ) ;
#12166 = EDGE_CURVE ( 'NONE', #39344, #19058, #13818, .T. ) ;
#12167 = B_SPLINE_SURFACE_WITH_KNOTS ( 'NONE', 3, 3, ( 
 ( #8461, #16396, #756, #20748 ),
 ( #40017, #21010, #48407, #40513 ),
 ( #40258, #5596, #36945, #36692 ),
 ( #32062, #12543, #1762, #4838 ) ),
 .UNSPECIFIED., .F., .F., .F.,
 ( 4, 4 ),
 ( 4, 4 ),
 ( 0.000000000000000000, 1.000000000000000000 ),
 ( 0.000000000000000000, 1.000000000000000000 ),
 .UNSPECIFIED. ) ;
#12168 = LINE ( 'NONE', #16525, #49800 ) ;
#12169 = FACE_OUTER_BOUND ( 'NONE', #30701, .T. ) ;
#12170 = EDGE_CURVE ( 'NONE', #29662, #26951, #22035, .T. ) ;
#12171 = EDGE_CURVE ( 'NONE', #9851, #32219, #31974, .T. ) ;
#12172 = CARTESIAN_POINT ( 'NONE',  ( -568.8466156985925863, 57.49999999999996447, -173.6910835022032700 ) ) ;
#12173 = DIRECTION ( 'NONE',  ( 0.000000000000000000, 0.000000000000000000, 1.000000000000000000 ) ) ;
#12174 = EDGE_LOOP ( 'NONE', ( #1540, #15895, #18865, #33980, #35113, #27016, #11122, #35300 ) ) ;
#12175 = CARTESIAN_POINT ( 'NONE',  ( 228.9999999999999716, -169.9999999999999716, 4.999999999999616307 ) ) ;
#12176 = EDGE_CURVE ( 'NONE', #29610, #49500, #36685, .T. ) ;
#12177 = CARTESIAN_POINT ( 'NONE',  ( 165.0000000000000000, -174.9999999999999716, -111.0000000000001563 ) ) ;
#12178 = ORIENTED_EDGE ( 'NONE', *, *, #8691, .F. ) ;
#12179 = AXIS2_PLACEMENT_3D ( 'NONE', #32431, #4722, #9325 ) ;
#12180 = CARTESIAN_POINT ( 'NONE',  ( 1.066995270233474624, -33.23888904628638841, -3.760136334089591248 ) ) ;
#12181 = LINE ( 'NONE', #46525, #4884 ) ;
#12182 = CARTESIAN_POINT ( 'NONE',  ( 0.000000000000000000, 184.8000000000000114, -359.8000000000002387 ) ) ;
#12183 = ORIENTED_EDGE ( 'NONE', *, *, #21794, .F. ) ;
#12184 = ORIENTED_EDGE ( 'NONE', *, *, #2827, .F. ) ;
#12185 = DIRECTION ( 'NONE',  ( -1.000000000000000000, -0.000000000000000000, -0.000000000000000000 ) ) ;
#12186 = CARTESIAN_POINT ( 'NONE',  ( 0.3370904143228981575, -0.2449105217885261532, 10.00000000000000000 ) ) ;
#12187 = EDGE_LOOP ( 'NONE', ( #10786, #35264, #42014, #13322 ) ) ;
#12188 = EDGE_LOOP ( 'NONE', ( #27948, #32644, #47740, #31346, #12018, #29269 ) ) ;
#12189 = DIRECTION ( 'NONE',  ( -0.000000000000000000, -0.000000000000000000, -1.000000000000000000 ) ) ;
#12190 = LINE ( 'NONE', #20384, #41171 ) ;
#12191 = CARTESIAN_POINT ( 'NONE',  ( 1.011271242968677653, 0.7347315653656002477, 10.00000000000000000 ) ) ;
#12192 = CARTESIAN_POINT ( 'NONE',  ( 15.00099850811936264, 7.462898891544210933, 9.403735324607438884 ) ) ;
#12193 = CARTESIAN_POINT ( 'NONE',  ( 72.27890028733797578, 1.750000000000010436, 119.7931612910808781 ) ) ;
#12194 = ORIENTED_EDGE ( 'NONE', *, *, #16161, .F. ) ;
#12195 = VERTEX_POINT ( 'NONE', #5883 ) ;
#12196 = ORIENTED_EDGE ( 'NONE', *, *, #40589, .F. ) ;
#12197 = ADVANCED_FACE ( 'NONE', ( #9988 ), #45616, .F. ) ;
#12198 = DIRECTION ( 'NONE',  ( 1.000000000000000000, 0.000000000000000000, 7.793956916774525800E-48 ) ) ;
#12199 = ORIENTED_EDGE ( 'NONE', *, *, #12648, .F. ) ;
#12200 = CARTESIAN_POINT ( 'NONE',  ( -1.315487699542658984, 0.8933127557393807372, 9.933337059263839919 ) ) ;
#12201 = ORIENTED_EDGE ( 'NONE', *, *, #30487, .T. ) ;
#12202 = EDGE_LOOP ( 'NONE', ( #41677, #13801, #35310, #39306 ) ) ;
#12203 = CARTESIAN_POINT ( 'NONE',  ( 191.5540265531850537, 1.025126265847089435, -117.4317124430720156 ) ) ;
#12204 = VERTEX_POINT ( 'NONE', #26139 ) ;
#12205 = EDGE_LOOP ( 'NONE', ( #4062, #30291, #30381 ) ) ;
#12206 = CARTESIAN_POINT ( 'NONE',  ( 16.99749102614301677, -1.320765928724307425, 8.953103998512858652 ) ) ;
#12207 = CARTESIAN_POINT ( 'NONE',  ( -166.6959734468149463, 1.750000000000010658, -79.18171244307201562 ) ) ;
#12209 = EDGE_LOOP ( 'NONE', ( #26785, #40468, #18932, #764, #49791, #32387, #42654, #29094, #1131, #23445, #35828, #38764 ) ) ;
#12208 = VECTOR ( 'NONE', #29378, 1000.000000000000000 ) ;
#12210 = FACE_OUTER_BOUND ( 'NONE', #45584, .T. ) ;
#12211 = CARTESIAN_POINT ( 'NONE',  ( -46.69597344681494633, 1.750000000000010658, 120.8182875569279702 ) ) ;
#12212 = CARTESIAN_POINT ( 'NONE',  ( -2.538055338523173443, -50.00000000000000000, -9.367992836599951190 ) ) ;
#12213 = AXIS2_PLACEMENT_3D ( 'NONE', #37055, #1881, #17525 ) ;
#12214 = EDGE_CURVE ( 'NONE', #32429, #43783, #18180, .T. ) ;
#12215 = FACE_OUTER_BOUND ( 'NONE', #33019, .T. ) ;
#12216 = CIRCLE ( 'NONE', #29427, 3.500000000000003109 ) ;
#12217 = VERTEX_POINT ( 'NONE', #33602 ) ;
#12218 = VECTOR ( 'NONE', #20453, 1000.000000000000000 ) ;
#12219 = LINE ( 'NONE', #3235, #35746 ) ;
#12220 = CARTESIAN_POINT ( 'NONE',  ( -206.6959734468149463, 0.000000000000000000, 165.0000000000000000 ) ) ;
#12221 = VECTOR ( 'NONE', #21292, 1000.000000000000000 ) ;
#12222 = EDGE_CURVE ( 'NONE', #9233, #36841, #49447, .T. ) ;
#12223 = DIRECTION ( 'NONE',  ( 1.586032892321651989E-16, -8.666415220619855873E-32, 1.000000000000000000 ) ) ;
#12224 = EDGE_CURVE ( 'NONE', #22094, #12195, #3872, .T. ) ;
#12225 = EDGE_CURVE ( 'NONE', #17811, #31254, #41285, .T. ) ;
#12226 = FACE_OUTER_BOUND ( 'NONE', #35569, .T. ) ;
#12227 = DIRECTION ( 'NONE',  ( 0.7233555441435719491, -0.6904757466825007794, 0.000000000000000000 ) ) ;
#12228 = LINE ( 'NONE', #27891, #44314 ) ;
#12229 = VERTEX_POINT ( 'NONE', #30249 ) ;
#12230 = CARTESIAN_POINT ( 'NONE',  ( -7.822422304254325276, -2.816136035261162185, 226.0000000000000000 ) ) ;
#12231 = DIRECTION ( 'NONE',  ( 0.000000000000000000, -0.000000000000000000, 1.000000000000000000 ) ) ;
#12232 = EDGE_LOOP ( 'NONE', ( #21216, #4045, #23734, #22737 ) ) ;
#12233 = PLANE ( 'NONE',  #3413 ) ;
#12234 = PLANE ( 'NONE',  #30755 ) ;
#12235 =( BOUNDED_CURVE ( )  B_SPLINE_CURVE ( 3, ( #43609, #20769, #17917, #33349 ),
 .UNSPECIFIED., .F., .F. ) 
 B_SPLINE_CURVE_WITH_KNOTS ( ( 4, 4 ),
 ( 4.712388980384689674, 6.283185307179586232 ),
 .UNSPECIFIED. ) 
 CURVE ( )  GEOMETRIC_REPRESENTATION_ITEM ( )  RATIONAL_B_SPLINE_CURVE ( ( 1.000000000000000000, 0.8047378541243649375, 0.8047378541243649375, 1.000000000000000000 ) ) 
 REPRESENTATION_ITEM ( '' )  );
#12236 = ORIENTED_EDGE ( 'NONE', *, *, #34023, .F. ) ;
#12237 = DIRECTION ( 'NONE',  ( 7.793956916774525800E-48, 0.000000000000000000, 1.000000000000000000 ) ) ;
#12238 = ORIENTED_EDGE ( 'NONE', *, *, #27587, .F. ) ;
#12239 = ORIENTED_EDGE ( 'NONE', *, *, #39309, .F. ) ;
#12240 = CARTESIAN_POINT ( 'NONE',  ( -556.7900739183570522, 53.53801056904005407, -65.53102910462104091 ) ) ;
#12241 = CARTESIAN_POINT ( 'NONE',  ( -4.945973446814903696, 2.143131898507912917E-16, 165.0000000000000000 ) ) ;
#12242 = VECTOR ( 'NONE', #4530, 1000.000000000000000 ) ;
#12243 = VECTOR ( 'NONE', #41887, 1000.000000000000000 ) ;
#12244 = VERTEX_POINT ( 'NONE', #37222 ) ;
#12245 = CARTESIAN_POINT ( 'NONE',  ( -164.9999999999978400, 17.00000000000000000, 95.00000000000000000 ) ) ;
#12246 = CARTESIAN_POINT ( 'NONE',  ( 168.9999999999999716, -252.4999999999999432, -339.9999999999998863 ) ) ;
#12247 = ORIENTED_EDGE ( 'NONE', *, *, #7775, .F. ) ;
#12248=STYLED_ITEM('',(#50747),#4281);
#12249 = AXIS2_PLACEMENT_3D ( 'NONE', #29207, #45577, #37427 ) ;
#12250 = DIRECTION ( 'NONE',  ( -1.000000000000000000, 0.000000000000000000, 0.000000000000000000 ) ) ;
#12251 = ORIENTED_EDGE ( 'NONE', *, *, #27728, .T. ) ;
#12252 = EDGE_CURVE ( 'NONE', #23225, #27522, #10736, .T. ) ;
#12253 = DIRECTION ( 'NONE',  ( 0.000000000000000000, 0.000000000000000000, 1.000000000000000000 ) ) ;
#12254 = CARTESIAN_POINT ( 'NONE',  ( -84.94597344681493212, -1.025126265847089657, -120.9317124430720440 ) ) ;
#12255 = CARTESIAN_POINT ( 'NONE',  ( 115.0540265531850395, 2.143131898507847836E-16, 159.0682875569279702 ) ) ;
#12256 = CIRCLE ( 'NONE', #9003, 3.750000000000000000 ) ;
#12257 = ORIENTED_EDGE ( 'NONE', *, *, #33825, .F. ) ;
#12258 = B_SPLINE_CURVE_WITH_KNOTS ( 'NONE', 3,
 ( #45962, #7000, #18534, #38323 ),
 .UNSPECIFIED., .F., .F.,
 ( 4, 4 ),
 ( 5.641302087661087512E-05, 0.0003272669002613764534 ),
 .UNSPECIFIED. ) ;
#12259 = CARTESIAN_POINT ( 'NONE',  ( -5.951572692819863342, 0.3107723024025113023, -2.642742795433417058E-16 ) ) ;
#12260 = CARTESIAN_POINT ( 'NONE',  ( 1.437255894074055185, -3.713052624461447682, -1.301042606982605321E-15 ) ) ;
#12261 = ORIENTED_EDGE ( 'NONE', *, *, #4808, .T. ) ;
#12262 = EDGE_LOOP ( 'NONE', ( #16607, #7848, #21845, #27651, #42861, #43104 ) ) ;
#12263 = ORIENTED_EDGE ( 'NONE', *, *, #25852, .F. ) ;
#12264 = CARTESIAN_POINT ( 'NONE',  ( -8.445973446814962315, -1.025126265847096985, 159.0682875569279418 ) ) ;
#12265 = CARTESIAN_POINT ( 'NONE',  ( 169.0000000000000000, -272.5000000000000000, -96.99999999999988631 ) ) ;
#12266 = EDGE_LOOP ( 'NONE', ( #5500, #29529, #14429, #20643, #8668 ) ) ;
#12267 = LINE ( 'NONE', #50461, #35673 ) ;
#12268 = DIRECTION ( 'NONE',  ( 0.000000000000000000, 0.000000000000000000, -1.000000000000000000 ) ) ;
#12269 = LINE ( 'NONE', #231, #32178 ) ;
#12270 = CARTESIAN_POINT ( 'NONE',  ( -46.69597344681494633, 1.750000000000010214, 40.81828755692798438 ) ) ;
#12271 = FACE_OUTER_BOUND ( 'NONE', #25143, .T. ) ;
#12272 = PLANE ( 'NONE',  #7852 ) ;
#12273 = CARTESIAN_POINT ( 'NONE',  ( -1.011271242968688533, 0.7347315653655859258, 10.00000000000000000 ) ) ;
#12274 = CARTESIAN_POINT ( 'NONE',  ( 1.286508520038679659, 0.4866366830693329426, 9.972175347158279024 ) ) ;
#12275 = CARTESIAN_POINT ( 'NONE',  ( -582.5000000000000000, -72.50000000000001421, -58.60000000000003695 ) ) ;
#12276 = CYLINDRICAL_SURFACE ( 'NONE', #7233, 4.000000000000003553 ) ;
#12277 = AXIS2_PLACEMENT_3D ( 'NONE', #28780, #44156, #37267 ) ;
#12278 = FACE_OUTER_BOUND ( 'NONE', #38970, .T. ) ;
#12279 = AXIS2_PLACEMENT_3D ( 'NONE', #37871, #2689, #18834 ) ;
#12280 = CARTESIAN_POINT ( 'NONE',  ( -0.6721397084974984892, -9.977385840602783773, 0.000000000000000000 ) ) ;
#12281 = CARTESIAN_POINT ( 'NONE',  ( 71.55402655318505367, 0.000000000000000000, 165.0000000000000000 ) ) ;
#12282 = ORIENTED_EDGE ( 'NONE', *, *, #34345, .T. ) ;
#12283 = EDGE_CURVE ( 'NONE', #10058, #2811, #30498, .T. ) ;
#12284 = VECTOR ( 'NONE', #3036, 1000.000000000000000 ) ;
#12285 = CARTESIAN_POINT ( 'NONE',  ( 339.9999999999999432, 169.0000000000000000, -344.0000000000001137 ) ) ;
#12286 = CARTESIAN_POINT ( 'NONE',  ( 35.00000000000028422, 16.00000000000000000, -60.00000000000000000 ) ) ;
#12287 = CARTESIAN_POINT ( 'NONE',  ( -88.44597344681494633, 1.025126265847088991, 2.568287556927986159 ) ) ;
#12288 = DIRECTION ( 'NONE',  ( -1.000000000000000000, -0.000000000000000000, -0.000000000000000000 ) ) ;
#12289 = AXIS2_PLACEMENT_3D ( 'NONE', #589, #9033, #48481 ) ;
#12290 = ORIENTED_EDGE ( 'NONE', *, *, #15348, .T. ) ;
#12291 = CARTESIAN_POINT ( 'NONE',  ( -6.695973446814940111, 1.750000000000024203, 120.8182875569279702 ) ) ;
#12292 = CARTESIAN_POINT ( 'NONE',  ( -128.4459734468149179, 0.000000000000000000, 39.06828755692801280 ) ) ;
#12293 = ORIENTED_EDGE ( 'NONE', *, *, #44640, .F. ) ;
#12294 = DIRECTION ( 'NONE',  ( -1.000000000000000000, -0.000000000000000000, -0.000000000000000000 ) ) ;
#12295 = LINE ( 'NONE', #19997, #15822 ) ;
#12296 = PLANE ( 'NONE',  #20275 ) ;
#12297 = ORIENTED_EDGE ( 'NONE', *, *, #4698, .F. ) ;
#12298 = DIRECTION ( 'NONE',  ( 0.000000000000000000, 0.000000000000000000, -1.000000000000000000 ) ) ;
#12299 = ORIENTED_EDGE ( 'NONE', *, *, #42129, .F. ) ;
#12300 = EDGE_CURVE ( 'NONE', #45326, #47156, #17922, .T. ) ;
#12301 = VERTEX_POINT ( 'NONE', #17689 ) ;
#12302 = LINE ( 'NONE', #39270, #9818 ) ;
#12303 = CARTESIAN_POINT ( 'NONE',  ( 183.0000000000000000, -164.9999999999999432, 355.9999999999998863 ) ) ;
#12304 = ORIENTED_EDGE ( 'NONE', *, *, #15856, .T. ) ;
#12305 = CARTESIAN_POINT ( 'NONE',  ( -165.3973046169136012, 70.03596893647589638, -94.69675437945477370 ) ) ;
#12306 = CARTESIAN_POINT ( 'NONE',  ( 115.0540265531850395, 1.025126265847082108, -77.43171244307201562 ) ) ;
#12307 = DIRECTION ( 'NONE',  ( 0.000000000000000000, 0.000000000000000000, -1.000000000000000000 ) ) ;
#12308 = EDGE_CURVE ( 'NONE', #37848, #23455, #32812, .T. ) ;
#12309 = DIRECTION ( 'NONE',  ( -1.000000000000000000, 0.000000000000000000, 0.000000000000000000 ) ) ;
#12310 = ORIENTED_EDGE ( 'NONE', *, *, #49933, .F. ) ;
#12311 = DIRECTION ( 'NONE',  ( 0.000000000000000000, 1.000000000000000000, 0.000000000000000000 ) ) ;
#12312 = VECTOR ( 'NONE', #26756, 1000.000000000000114 ) ;
#12313 = VECTOR ( 'NONE', #6482, 1000.000000000000000 ) ;
#12314 = ORIENTED_EDGE ( 'NONE', *, *, #13704, .F. ) ;
#12315 = CARTESIAN_POINT ( 'NONE',  ( -128.4459734468149463, -1.025126265847081886, -80.93171244307201562 ) ) ;
#12316 = ORIENTED_EDGE ( 'NONE', *, *, #50105, .F. ) ;
#12317 = PLANE ( 'NONE',  #25403 ) ;
#12318 = VECTOR ( 'NONE', #43246, 1000.000000000000000 ) ;
#12319 = CARTESIAN_POINT ( 'NONE',  ( -166.6959734468149463, 0.000000000000000000, 165.0000000000000000 ) ) ;
#12320 = VECTOR ( 'NONE', #8203, 1000.000000000000000 ) ;
#12321 = VERTEX_POINT ( 'NONE', #14080 ) ;
#12322 = CARTESIAN_POINT ( 'NONE',  ( -44.94597344681493922, 2.143131898507880377E-16, 79.06828755692797017 ) ) ;
#12323 = CARTESIAN_POINT ( 'NONE',  ( 341.9999999999999432, -168.9999999999999147, 343.9999999999998295 ) ) ;
#12324 = CARTESIAN_POINT ( 'NONE',  ( -50.64730461691362962, -42.31198943095992604, 742.8425600500171413 ) ) ;
#12325 = CARTESIAN_POINT ( 'NONE',  ( 350.0000000000000000, 185.0000000000000284, -344.0000000000001705 ) ) ;
#12326 = VERTEX_POINT ( 'NONE', #49941 ) ;
#12327 = FACE_OUTER_BOUND ( 'NONE', #19410, .T. ) ;
#12328 = CARTESIAN_POINT ( 'NONE',  ( 0.000000000000000000, 0.000000000000000000, -10.00000000000000000 ) ) ;
#12329 = CARTESIAN_POINT ( 'NONE',  ( 73.30402655318508209, 1.750000000000010658, 80.81828755692798438 ) ) ;
#12330 = ORIENTED_EDGE ( 'NONE', *, *, #14183, .T. ) ;
#12331 = ORIENTED_EDGE ( 'NONE', *, *, #5582, .F. ) ;
#12332 = APPLICATION_PROTOCOL_DEFINITION ( 'draft international standard', 'automotive_design', 1998, #48559 ) ;
#12333 = DIRECTION ( 'NONE',  ( 1.000000000000000000, 0.000000000000000000, 0.000000000000000000 ) ) ;
#12334 = DIRECTION ( 'NONE',  ( 0.000000000000000000, -1.000000000000000000, 0.000000000000000000 ) ) ;
#12335 = EDGE_CURVE ( 'NONE', #42650, #1069, #42042, .T. ) ;
#12336 = DIRECTION ( 'NONE',  ( 0.000000000000000000, -2.969158215481698263E-48, 1.000000000000000000 ) ) ;
#12337 = CARTESIAN_POINT ( 'NONE',  ( 1.104345476778523016, 0.6507740520594131883, 9.967237415621767127 ) ) ;
#12338 = ORIENTED_EDGE ( 'NONE', *, *, #5109, .T. ) ;
#12339 = LINE ( 'NONE', #12851, #30480 ) ;
#12340 = EDGE_CURVE ( 'NONE', #25272, #5007, #22542, .T. ) ;
#12341 = LINE ( 'NONE', #23900, #26968 ) ;
#12342 = CARTESIAN_POINT ( 'NONE',  ( 115.0540265531850395, 1.025126265847081886, -40.93171244307202272 ) ) ;
#12343 = EDGE_CURVE ( 'NONE', #11870, #15720, #29741, .T. ) ;
#12344 = CARTESIAN_POINT ( 'NONE',  ( 339.9999999999998863, -166.9999999999999432, 343.9999999999997726 ) ) ;
#12345 = AXIS2_PLACEMENT_3D ( 'NONE', #46084, #7136, #19167 ) ;
#12346 = EDGE_CURVE ( 'NONE', #10429, #9357, #34608, .T. ) ;
#12347 = ORIENTED_EDGE ( 'NONE', *, *, #24268, .F. ) ;
#12348 = VECTOR ( 'NONE', #9703, 1000.000000000000000 ) ;
#12349 = ORIENTED_EDGE ( 'NONE', *, *, #9216, .T. ) ;
#12350 = CARTESIAN_POINT ( 'NONE',  ( 31.55402655318503236, 0.000000000000000000, -80.93171244307204404 ) ) ;
#12351 = ORIENTED_EDGE ( 'NONE', *, *, #16338, .T. ) ;
#12352 = CARTESIAN_POINT ( 'NONE',  ( -22.69295089195507487, -45.31600496604688999, 7.455576670931136185 ) ) ;
#12353 = LINE ( 'NONE', #4671, #40514 ) ;
#12354 = MECHANICAL_DESIGN_GEOMETRIC_PRESENTATION_REPRESENTATION (  '', ( #22971 ), #27086 ) ;
#12355 = CARTESIAN_POINT ( 'NONE',  ( -84.94597344681494633, 2.143131898507880377E-16, 39.06828755692798438 ) ) ;
#12356 = CARTESIAN_POINT ( 'NONE',  ( -124.9459734468149463, 2.143131898507847836E-16, -77.43171244307204404 ) ) ;
#12357 = ORIENTED_EDGE ( 'NONE', *, *, #31517, .T. ) ;
#12358 = CARTESIAN_POINT ( 'NONE',  ( -124.9459734468149463, 2.143131898507847836E-16, -0.9317124430719969652 ) ) ;
#12359 = CARTESIAN_POINT ( 'NONE',  ( -164.9999999999997442, 17.00000000000000000, -84.99999999999998579 ) ) ;
#12360 = ORIENTED_EDGE ( 'NONE', *, *, #1470, .T. ) ;
#12361 = CARTESIAN_POINT ( 'NONE',  ( 130.0000000000002842, 17.00000000000000000, -84.99999999999998579 ) ) ;
#12362 = CARTESIAN_POINT ( 'NONE',  ( 0.000000000000000000, 17.00000000000000000, 0.000000000000000000 ) ) ;
#12363 = CARTESIAN_POINT ( 'NONE',  ( 17.23491422248386584, -0.5912720620000816441, 8.727788335465566760 ) ) ;
#12364 = DIRECTION ( 'NONE',  ( -0.3090169943749515591, 0.9510565162951523099, 0.000000000000000000 ) ) ;
#12365 = VERTEX_POINT ( 'NONE', #12020 ) ;
#12366 = B_SPLINE_CURVE_WITH_KNOTS ( 'NONE', 3,
 ( #30259, #22803, #25460, #41108 ),
 .UNSPECIFIED., .F., .F.,
 ( 4, 4 ),
 ( 0.7998230999345288250, 0.9869080488566183140 ),
 .UNSPECIFIED. ) ;
#12368 = EDGE_LOOP ( 'NONE', ( #22173, #12497, #28307, #9749 ) ) ;
#12367 = EDGE_CURVE ( 'NONE', #12051, #16336, #10589, .T. ) ;
#12369 = DIRECTION ( 'NONE',  ( -0.000000000000000000, -1.000000000000000000, -0.000000000000000000 ) ) ;
#12370 = EDGE_CURVE ( 'NONE', #46883, #17305, #15863, .T. ) ;
#12371 = ADVANCED_BREP_SHAPE_REPRESENTATION ( '', ( #38799, #38969, #38632, #45486 ), #9445 ) ;
#12372 =( BOUNDED_CURVE ( )  B_SPLINE_CURVE ( 3, ( #20124, #39142, #7574, #39398 ),
 .UNSPECIFIED., .F., .F. ) 
 B_SPLINE_CURVE_WITH_KNOTS ( ( 4, 4 ),
 ( 4.712388980384689674, 6.283185307179586232 ),
 .UNSPECIFIED. ) 
 CURVE ( )  GEOMETRIC_REPRESENTATION_ITEM ( )  RATIONAL_B_SPLINE_CURVE ( ( 1.000000000000000000, 0.8047378541243649375, 0.8047378541243649375, 1.000000000000000000 ) ) 
 REPRESENTATION_ITEM ( '' )  );
#12373 = EDGE_CURVE ( 'NONE', #10907, #31922, #14315, .T. ) ;
#12374 = ADVANCED_FACE ( 'NONE', ( #42539 ), #15102, .T. ) ;
#12375 = ORIENTED_EDGE ( 'NONE', *, *, #18636, .T. ) ;
#12376 = CYLINDRICAL_SURFACE ( 'NONE', #1222, 1.750000000000008438 ) ;
#12377 = FACE_OUTER_BOUND ( 'NONE', #30112, .T. ) ;
#12378 = CARTESIAN_POINT ( 'NONE',  ( -10.49999999999999467, -46.01315789473684248, 5.916985404131813731 ) ) ;
#12379 = VERTEX_POINT ( 'NONE', #23042 ) ;
#12380 = LINE ( 'NONE', #20082, #40739 ) ;
#12381 = EDGE_CURVE ( 'NONE', #31274, #33538, #27414, .T. ) ;
#12382 =( BOUNDED_CURVE ( )  B_SPLINE_CURVE ( 3, ( #44942, #49026, #9823, #6242 ),
 .UNSPECIFIED., .F., .F. ) 
 B_SPLINE_CURVE_WITH_KNOTS ( ( 4, 4 ),
 ( 3.141592653589793116, 4.712388980384689674 ),
 .UNSPECIFIED. ) 
 CURVE ( )  GEOMETRIC_REPRESENTATION_ITEM ( )  RATIONAL_B_SPLINE_CURVE ( ( 1.000000000000000000, 0.8047378541243649375, 0.8047378541243649375, 1.000000000000000000 ) ) 
 REPRESENTATION_ITEM ( '' )  );
#12383 = EDGE_CURVE ( 'NONE', #3452, #48040, #46372, .T. ) ;
#12384 = DIRECTION ( 'NONE',  ( 4.758098676964954489E-16, 1.000000000000000000, 1.751623080406021339E-46 ) ) ;
#12385 = VECTOR ( 'NONE', #47508, 1000.000000000000000 ) ;
#12386 = DIRECTION ( 'NONE',  ( 1.000000000000000000, 0.000000000000000000, 0.000000000000000000 ) ) ;
#12387 = ORIENTED_EDGE ( 'NONE', *, *, #23670, .F. ) ;
#12388 = EDGE_LOOP ( 'NONE', ( #6409, #6274, #42966 ) ) ;
#12389 = ORIENTED_EDGE ( 'NONE', *, *, #16780, .T. ) ;
#12390 = VECTOR ( 'NONE', #36354, 1000.000000000000000 ) ;
#12391 = CARTESIAN_POINT ( 'NONE',  ( 5.551115123125782702E-14, -182.9999999999999716, 343.9999999999997726 ) ) ;
#12392 =( BOUNDED_CURVE ( )  B_SPLINE_CURVE ( 3, ( #35404, #7682, #3557, #4339 ),
 .UNSPECIFIED., .F., .F. ) 
 B_SPLINE_CURVE_WITH_KNOTS ( ( 4, 4 ),
 ( 1.570796326794896558, 3.141592653589793116 ),
 .UNSPECIFIED. ) 
 CURVE ( )  GEOMETRIC_REPRESENTATION_ITEM ( )  RATIONAL_B_SPLINE_CURVE ( ( 1.000000000000000000, 0.8047378541243649375, 0.8047378541243649375, 1.000000000000000000 ) ) 
 REPRESENTATION_ITEM ( '' )  );
#12393 = PRODUCT_DEFINITION_CONTEXT ( 'detailed design', #13525, 'design' ) ;
#12394 = ORIENTED_EDGE ( 'NONE', *, *, #2602, .T. ) ;
#12395 = CARTESIAN_POINT ( 'NONE',  ( -64.99999999999909051, 16.00000000000000000, 0.000000000000000000 ) ) ;
#12396 = AXIS2_PLACEMENT_3D ( 'NONE', #45579, #2746, #18898 ) ;
#12397 = ORIENTED_EDGE ( 'NONE', *, *, #1240, .F. ) ;
#12398 = ADVANCED_FACE ( 'NONE', ( #16120 ), #31782, .F. ) ;
#12399 = CARTESIAN_POINT ( 'NONE',  ( 9.174209336589868258, 3.979181203266223488, 9.646707543097347681 ) ) ;
#12400 = VERTEX_POINT ( 'NONE', #19188 ) ;
#12401 = CARTESIAN_POINT ( 'NONE',  ( -128.4459734468149179, 0.000000000000000000, 39.06828755692801280 ) ) ;
#12402 = CARTESIAN_POINT ( 'NONE',  ( -84.94597344681494633, 2.143131898507880377E-16, 119.0682875569279702 ) ) ;
#12403 = DIRECTION ( 'NONE',  ( 0.8411784753765542133, 0.000000000000000000, -0.5407575913134976542 ) ) ;
#12404 = EDGE_CURVE ( 'NONE', #3395, #38611, #34876, .T. ) ;
#12405 = EDGE_CURVE ( 'NONE', #39651, #11178, #43302, .T. ) ;
#12406 = CARTESIAN_POINT ( 'NONE',  ( 370.7621192902014968, 53.53801056904005407, -93.79675437945476801 ) ) ;
#12407 = FACE_BOUND ( 'NONE', #28364, .T. ) ;
#12408 = CARTESIAN_POINT ( 'NONE',  ( 12.97493236725083676, -11.05939663306990717, 8.953103998512858652 ) ) ;
#12409 = ORIENTED_EDGE ( 'NONE', *, *, #11217, .F. ) ;
#12410 = ORIENTED_EDGE ( 'NONE', *, *, #25559, .F. ) ;
#12411 = DIRECTION ( 'NONE',  ( -0.000000000000000000, -0.000000000000000000, -1.000000000000000000 ) ) ;
#12412 = DIRECTION ( 'NONE',  ( 0.000000000000000000, 0.000000000000000000, -1.000000000000000000 ) ) ;
#12413 = DIRECTION ( 'NONE',  ( -0.9908916497796512735, 0.000000000000000000, -0.1346615698592613652 ) ) ;
#12414 = CARTESIAN_POINT ( 'NONE',  ( 181.0000000000000000, 175.0000000000000284, -358.0000000000001705 ) ) ;
#12415 = EDGE_LOOP ( 'NONE', ( #11613, #14700, #33107, #9920 ) ) ;
#12416 = EDGE_CURVE ( 'NONE', #29858, #24991, #43045, .T. ) ;
#12417 = DIRECTION ( 'NONE',  ( 0.000000000000000000, 0.000000000000000000, -1.000000000000000000 ) ) ;
#12418 = CARTESIAN_POINT ( 'NONE',  ( 195.0540265531851105, -1.025126265847089213, -160.9317124430720014 ) ) ;
#12419 = ORIENTED_EDGE ( 'NONE', *, *, #39681, .F. ) ;
#12420 = AXIS2_PLACEMENT_3D ( 'NONE', #10339, #33196, #18259 ) ;
#12421 = DIRECTION ( 'NONE',  ( 0.000000000000000000, -1.000000000000000000, 0.000000000000000000 ) ) ;
#12422 = EDGE_CURVE ( 'NONE', #19097, #36058, #8174, .T. ) ;
#12423 = DIRECTION ( 'NONE',  ( 0.000000000000000000, -1.000000000000000000, 1.604368532695312981E-16 ) ) ;
#12424 = DIRECTION ( 'NONE',  ( -1.000000000000000000, -0.000000000000000000, -0.000000000000000000 ) ) ;
#12425 = ORIENTED_EDGE ( 'NONE', *, *, #44165, .T. ) ;
#12426 = VECTOR ( 'NONE', #40326, 1000.000000000000000 ) ;
#12427 = EDGE_LOOP ( 'NONE', ( #846, #19104, #16504, #43224, #26453, #1469, #39989, #22761 ) ) ;
#12428 = CARTESIAN_POINT ( 'NONE',  ( 1.104609456715839766, 0.6504863887005235545, 9.948547179989622791 ) ) ;
#12429 = CARTESIAN_POINT ( 'NONE',  ( -47.72109971266203132, 1.750000000000009326, -158.1565861772249377 ) ) ;
#12430 = EDGE_CURVE ( 'NONE', #19251, #23733, #35280, .T. ) ;
#12431 = EDGE_CURVE ( 'NONE', #4734, #30864, #4321, .T. ) ;
#12432 = ORIENTED_EDGE ( 'NONE', *, *, #21750, .F. ) ;
#12433 = EDGE_LOOP ( 'NONE', ( #23272, #31365, #35067, #44053 ) ) ;
#12434 = CARTESIAN_POINT ( 'NONE',  ( -9.760995290733800900, 2.173239732351794462, 9.646707543097347681 ) ) ;
#12435 = DIRECTION ( 'NONE',  ( -0.000000000000000000, -0.000000000000000000, -1.000000000000000000 ) ) ;
#12436 = CARTESIAN_POINT ( 'NONE',  ( -206.6959734468149463, -1.750000000000010214, 40.81828755692798438 ) ) ;
#12437 = CARTESIAN_POINT ( 'NONE',  ( 71.55402655318505367, 1.025126265847089657, 119.0682875569279560 ) ) ;
#12438 = VERTEX_POINT ( 'NONE', #7929 ) ;
#12439 = ORIENTED_EDGE ( 'NONE', *, *, #10574, .T. ) ;
#12440 = VERTEX_POINT ( 'NONE', #22795 ) ;
#12441 = ADVANCED_FACE ( 'NONE', ( #23566 ), #28469, .T. ) ;
#12442 = EDGE_CURVE ( 'NONE', #49361, #40327, #31112, .T. ) ;
#12443 = CYLINDRICAL_SURFACE ( 'NONE', #8681, 1.880036658038868103 ) ;
#12444 = ADVANCED_FACE ( 'NONE', ( #717 ), #16882, .F. ) ;
#12445 = ORIENTED_EDGE ( 'NONE', *, *, #24038, .T. ) ;
#12446 = DIRECTION ( 'NONE',  ( 0.1671032855531318084, 0.5142910309547740200, -0.8411784753765541023 ) ) ;
#12447 = ORIENTED_EDGE ( 'NONE', *, *, #21750, .T. ) ;
#12448 = VERTEX_POINT ( 'NONE', #1732 ) ;
#12449 = PLANE ( 'NONE',  #4960 ) ;
#12450 = CARTESIAN_POINT ( 'NONE',  ( -21.61731705588949737, -25.43568671410585935, -9.367992836599954742 ) ) ;
#12451 = VECTOR ( 'NONE', #18746, 1000.000000000000000 ) ;
#12452 = EDGE_CURVE ( 'NONE', #40254, #18731, #48376, .T. ) ;
#12453 = CARTESIAN_POINT ( 'NONE',  ( 14.29087950072012170, 9.652079258044652832, 8.727788335465566760 ) ) ;
#12454 = EDGE_LOOP ( 'NONE', ( #17852, #42109, #8344, #22731, #8116, #20496, #46844, #34906, #23353, #20313, #43168, #46319, #48181, #1556, #24225, #17226, #23759, #41035, #20881, #16617, #13935, #6497, #12702, #34280, #37590, #15750, #46140, #31955, #12299, #48739, #42613, #6651, #28917, #22318, #44828, #38839, #22701, #10276, #14521, #31019, #4451, #11090, #43779, #49192, #31180, #40832, #29123, #36862, #12503, #5567, #16105, #7706, #22, #3138, #26671, #821, #5044, #31666, #39116, #16987, #38437, #23083, #32235, #12148, #34602, #5096, #1535, #41394, #24261, #36271, #6130, #4098, #26274, #50703, #32838, #39845, #32013, #50280, #25222, #12757, #34326, #25269, #41020, #11969, #1067, #22562, #24205, #43283, #28722, #15172, #15760, #46144, #35887, #37881, #49491, #10020, #18849, #14403, #42324, #43488 ) ) ;
#12455 = VERTEX_POINT ( 'NONE', #5319 ) ;
#12456 = PLANE ( 'NONE',  #2057 ) ;
#12457 = DIRECTION ( 'NONE',  ( -1.000000000000000000, -0.000000000000000000, -0.000000000000000000 ) ) ;
#12458 = ORIENTED_EDGE ( 'NONE', *, *, #20221, .T. ) ;
#12459 = CARTESIAN_POINT ( 'NONE',  ( 0.000000000000000000, 17.00000000000000000, 0.000000000000000000 ) ) ;
#12460 = CARTESIAN_POINT ( 'NONE',  ( -2.595273106918313033, -2.906811120256372671, 9.741991644047246268 ) ) ;
#12461 = CYLINDRICAL_SURFACE ( 'NONE', #32809, 2.000000000000001776 ) ;
#12462 = AXIS2_PLACEMENT_3D ( 'NONE', #6025, #22193, #6789 ) ;
#12463 = CARTESIAN_POINT ( 'NONE',  ( 13.59579750444771307, -10.60877755095900632, 8.727788335465566760 ) ) ;
#12464 = ORIENTED_EDGE ( 'NONE', *, *, #16810, .T. ) ;
#12465 = DIRECTION ( 'NONE',  ( 0.000000000000000000, 0.000000000000000000, -1.000000000000000000 ) ) ;
#12466 = FACE_OUTER_BOUND ( 'NONE', #11306, .T. ) ;
#12467 = CARTESIAN_POINT ( 'NONE',  ( 155.0540265531850537, 2.143131898507880377E-16, 122.5682875569279702 ) ) ;
#12468 = DIRECTION ( 'NONE',  ( -1.000000000000000000, -0.000000000000000000, 9.251858538543084240E-16 ) ) ;
#12469 = CARTESIAN_POINT ( 'NONE',  ( 210.0000000000000568, 0.000000000000000000, -159.1817124430720298 ) ) ;
#12470 = AXIS2_PLACEMENT_3D ( 'NONE', #2405, #18049, #6758 ) ;
#12471 = CARTESIAN_POINT ( 'NONE',  ( -164.9459734468149463, 1.025126265847088991, 162.5682875569279133 ) ) ;
#12472 = DIRECTION ( 'NONE',  ( -0.000000000000000000, -1.000000000000000000, -0.000000000000000000 ) ) ;
#12473 = EDGE_LOOP ( 'NONE', ( #17167, #20280, #39150, #34773, #26833, #3058 ) ) ;
#12474 = CARTESIAN_POINT ( 'NONE',  ( 183.0000000000000000, -184.9999999999999716, -356.0000000000001705 ) ) ;
#12475 = CARTESIAN_POINT ( 'NONE',  ( 193.3040265531851105, -1.750000000000009992, 160.8182875569279702 ) ) ;
#12476 = MECHANICAL_DESIGN_GEOMETRIC_PRESENTATION_REPRESENTATION (  '', ( #29698 ), #31333 ) ;
#12477 = ORIENTED_EDGE ( 'NONE', *, *, #28567, .T. ) ;
#12478 = LINE ( 'NONE', #19928, #17166 ) ;
#12479 = CARTESIAN_POINT ( 'NONE',  ( 24.47767542868285062, -23.18653802921781448, 8.807470649214879543 ) ) ;
#12480 = FACE_OUTER_BOUND ( 'NONE', #11059, .T. ) ;
#12481 = AXIS2_PLACEMENT_3D ( 'NONE', #15429, #31086, #14922 ) ;
#12482 = ORIENTED_EDGE ( 'NONE', *, *, #6786, .F. ) ;
#12483 = FACE_OUTER_BOUND ( 'NONE', #28221, .T. ) ;
#12484 = ORIENTED_EDGE ( 'NONE', *, *, #31861, .T. ) ;
#12485 = ORIENTED_EDGE ( 'NONE', *, *, #14011, .T. ) ;
#12486 = CARTESIAN_POINT ( 'NONE',  ( 135.0000000000015632, 17.00000000000000000, 35.00000000000000000 ) ) ;
#12487 = CARTESIAN_POINT ( 'NONE',  ( 6.204997580903516941, 7.611558401714507482, 230.0000000000000000 ) ) ;
#12488 = EDGE_CURVE ( 'NONE', #3794, #20580, #38322, .T. ) ;
#12489 = EDGE_CURVE ( 'NONE', #39670, #31422, #981, .T. ) ;
#12490 = ORIENTED_EDGE ( 'NONE', *, *, #42891, .F. ) ;
#12491 = VECTOR ( 'NONE', #45216, 1000.000000000000000 ) ;
#12492 = CYLINDRICAL_SURFACE ( 'NONE', #31154, 2.000000000000001776 ) ;
#12493 = DIRECTION ( 'NONE',  ( -1.000000000000000000, 0.000000000000000000, 0.000000000000000000 ) ) ;
#12494 = ORIENTED_EDGE ( 'NONE', *, *, #3523, .F. ) ;
#12495 = ADVANCED_FACE ( 'NONE', ( #24830 ), #47878, .T. ) ;
#12496 = CARTESIAN_POINT ( 'NONE',  ( 0.6369768774142625656, -1.285364331396288806, 9.950105812514305370 ) ) ;
#12497 = ORIENTED_EDGE ( 'NONE', *, *, #48342, .F. ) ;
#12499 = EDGE_CURVE ( 'NONE', #31445, #4257, #44054, .T. ) ;
#12498 = CARTESIAN_POINT ( 'NONE',  ( 21.23829395927641883, 7.611558401714507482, 229.0000000000000000 ) ) ;
#12500 = DIRECTION ( 'NONE',  ( -1.000000000000000000, 0.000000000000000000, -2.958228394578794270E-31 ) ) ;
#12501 = EDGE_CURVE ( 'NONE', #13237, #7540, #49118, .T. ) ;
#12502 = CARTESIAN_POINT ( 'NONE',  ( 0.4402948852767718524, -2.015117899693914527, 9.894754715216725671 ) ) ;
#12503 = ORIENTED_EDGE ( 'NONE', *, *, #7771, .F. ) ;
#12504 = CARTESIAN_POINT ( 'NONE',  ( 164.9999999999999716, 17.00000000000000000, 29.99999999999999289 ) ) ;
#12505 = CARTESIAN_POINT ( 'NONE',  ( 168.9999999999999716, -272.4999999999999432, -355.9999999999999432 ) ) ;
#12506 = ORIENTED_EDGE ( 'NONE', *, *, #33479, .T. ) ;
#12507 = ORIENTED_EDGE ( 'NONE', *, *, #47578, .F. ) ;
#12508 = ORIENTED_EDGE ( 'NONE', *, *, #38535, .F. ) ;
#12509 = CARTESIAN_POINT ( 'NONE',  ( -69.99999999999972999, 17.00000000000000000, -84.99999999999998579 ) ) ;
#12510 = EDGE_CURVE ( 'NONE', #46117, #30636, #3301, .T. ) ;
#12511 = VECTOR ( 'NONE', #41093, 1000.000000000000000 ) ;
#12512 = FACE_OUTER_BOUND ( 'NONE', #6000, .T. ) ;
#12513 = VERTEX_POINT ( 'NONE', #32543 ) ;
#12514 = CARTESIAN_POINT ( 'NONE',  ( -48.33712804702535237, -13.03701565032741705, -9.367992836599951190 ) ) ;
#12515 = LINE ( 'NONE', #39992, #33815 ) ;
#12516 = CARTESIAN_POINT ( 'NONE',  ( -29.61572577327014955, -16.11461842845715253, 8.807470649214879543 ) ) ;
#12517 = FACE_OUTER_BOUND ( 'NONE', #48961, .T. ) ;
#12518 = LINE ( 'NONE', #47886, #22239 ) ;
#12519 = PRESENTATION_LAYER_ASSIGNMENT (  '', '', ( #28896 ) ) ;
#12520 = DIRECTION ( 'NONE',  ( 0.000000000000000000, 0.000000000000000000, 1.000000000000000000 ) ) ;
#12521 = CARTESIAN_POINT ( 'NONE',  ( 49.46074318306830975, -9.578883844006831794, 8.807470649214879543 ) ) ;
#12522 = LINE ( 'NONE', #17386, #29125 ) ;
#12524 = B_SPLINE_CURVE_WITH_KNOTS ( 'NONE', 3,
 ( #8805, #4190, #32400, #19828 ),
 .UNSPECIFIED., .F., .F.,
 ( 4, 4 ),
 ( 0.9890644561682322422, 1.000000000000000000 ),
 .UNSPECIFIED. ) ;
#12523 = CARTESIAN_POINT ( 'NONE',  ( 35.87018513526846419, 11.05844981164239194, -6.568693074176337632 ) ) ;
#12525 = CARTESIAN_POINT ( 'NONE',  ( 0.000000000000000000, 17.00000000000000000, 0.000000000000000000 ) ) ;
#12526 = COLOUR_RGB ( '',0.7921568627450980005, 0.8196078431372548767, 0.9333333333333333481 ) ;
#12527 = DIRECTION ( 'NONE',  ( 0.000000000000000000, 0.000000000000000000, 1.000000000000000000 ) ) ;
#12528 = VECTOR ( 'NONE', #5712, 1000.000000000000000 ) ;
#12529 = DIRECTION ( 'NONE',  ( 0.000000000000000000, -1.000000000000000000, 0.000000000000000000 ) ) ;
#12530 = LINE ( 'NONE', #19469, #27307 ) ;
#12531 = ORIENTED_EDGE ( 'NONE', *, *, #32860, .F. ) ;
#12532 = LINE ( 'NONE', #28455, #4049 ) ;
#12533 = EDGE_CURVE ( 'NONE', #44854, #39344, #20218, .T. ) ;
#12534 =( BOUNDED_CURVE ( )  B_SPLINE_CURVE ( 3, ( #27815, #8071, #117, #31419 ),
 .UNSPECIFIED., .F., .F. ) 
 B_SPLINE_CURVE_WITH_KNOTS ( ( 4, 4 ),
 ( 1.570796326794897002, 3.141592653589793560 ),
 .UNSPECIFIED. ) 
 CURVE ( )  GEOMETRIC_REPRESENTATION_ITEM ( )  RATIONAL_B_SPLINE_CURVE ( ( 1.000000000000000000, 0.8047378541243649375, 0.8047378541243649375, 1.000000000000000000 ) ) 
 REPRESENTATION_ITEM ( '' )  );
#12535 = DIRECTION ( 'NONE',  ( 0.000000000000000000, 0.000000000000000000, -1.000000000000000000 ) ) ;
#12536 = CARTESIAN_POINT ( 'NONE',  ( -2.707743684961791075, -37.43817128298309882, -5.338708898921614043 ) ) ;
#12537 = LINE ( 'NONE', #34905, #12320 ) ;
#12538 = EDGE_CURVE ( 'NONE', #40406, #37272, #45155, .T. ) ;
#12539 = ORIENTED_EDGE ( 'NONE', *, *, #20259, .F. ) ;
#12540 = DIRECTION ( 'NONE',  ( 0.000000000000000000, 0.000000000000000000, -1.000000000000000000 ) ) ;
#12541 = DIRECTION ( 'NONE',  ( 1.000000000000000000, 0.000000000000000000, 0.000000000000000000 ) ) ;
#12542 = ORIENTED_EDGE ( 'NONE', *, *, #49464, .F. ) ;
#12543 = CARTESIAN_POINT ( 'NONE',  ( -23.31729631074215092, -24.19776167542410406, -8.016098858316205167 ) ) ;
#12544 = CARTESIAN_POINT ( 'NONE',  ( -126.6959734468149321, 1.749999999999997113, 40.81828755692798438 ) ) ;
#12545 = FACE_OUTER_BOUND ( 'NONE', #14702, .T. ) ;
#12546 = ORIENTED_EDGE ( 'NONE', *, *, #31423, .T. ) ;
#12547 = DIRECTION ( 'NONE',  ( -1.000000000000000000, 0.000000000000000000, 0.000000000000000000 ) ) ;
#12548 = ORIENTED_EDGE ( 'NONE', *, *, #4222, .T. ) ;
#12549 = VERTEX_POINT ( 'NONE', #43559 ) ;
#12550 = VERTEX_POINT ( 'NONE', #20719 ) ;
#12551 = DIRECTION ( 'NONE',  ( -0.000000000000000000, -1.000000000000000000, -0.000000000000000000 ) ) ;
#12552 = CARTESIAN_POINT ( 'NONE',  ( 181.0000000000000000, -184.9999999999999716, -340.0000000000001137 ) ) ;
#12553 = VERTEX_POINT ( 'NONE', #8428 ) ;
#12554 = CARTESIAN_POINT ( 'NONE',  ( 80.00000000000153477, 17.00000000000000000, 35.00000000000000000 ) ) ;
#12555 = DIRECTION ( 'NONE',  ( 1.000000000000000000, 0.000000000000000000, 7.793956916774525800E-48 ) ) ;
#12556 = AXIS2_PLACEMENT_3D ( 'NONE', #7560, #19084, #34775 ) ;
#12557 = DIRECTION ( 'NONE',  ( -1.000000000000000000, -0.000000000000000000, -0.000000000000000000 ) ) ;
#12558 = CARTESIAN_POINT ( 'NONE',  ( -7.398363427652413726, 15.19415887381139285, -9.008049429158102583 ) ) ;
#12559 = ORIENTED_EDGE ( 'NONE', *, *, #22229, .F. ) ;
#12560=STYLED_ITEM('',(#50747),#39637);
#12561 = CARTESIAN_POINT ( 'NONE',  ( 164.9999999999999716, 17.00000000000000000, -30.00000000000001421 ) ) ;
#12562 = EDGE_LOOP ( 'NONE', ( #10430, #8768, #40903, #13453 ) ) ;
#12563 = CARTESIAN_POINT ( 'NONE',  ( 2.569099690548740877, -33.19126772784019153, 3.199614146704519602 ) ) ;
#12564 = CARTESIAN_POINT ( 'NONE',  ( -128.4459734468149179, 0.000000000000000000, -80.93171244307201562 ) ) ;
#12565 = ORIENTED_EDGE ( 'NONE', *, *, #2492, .T. ) ;
#12566 = DIRECTION ( 'NONE',  ( -1.000000000000000000, 0.000000000000000000, 0.000000000000000000 ) ) ;
#12567 = EDGE_CURVE ( 'NONE', #5307, #38906, #48124, .T. ) ;
#12568 = CARTESIAN_POINT ( 'NONE',  ( 169.0000000000000284, 175.0000000000000284, 357.9999999999998863 ) ) ;
#12569 = B_SPLINE_SURFACE_WITH_KNOTS ( 'NONE', 3, 3, ( 
 ( #10090, #41393, #29344, #37569 ),
 ( #5731, #2389, #37325, #17033 ),
 ( #40647, #33214, #18033, #5482 ),
 ( #48288, #17540, #21133, #44463 ) ),
 .UNSPECIFIED., .F., .F., .F.,
 ( 4, 4 ),
 ( 4, 4 ),
 ( 0.000000000000000000, 1.000000000000000000 ),
 ( 0.000000000000000000, 1.000000000000000000 ),
 .UNSPECIFIED. ) ;
#12570 = EDGE_LOOP ( 'NONE', ( #40357, #29917, #2076, #5249 ) ) ;
#12571 = LINE ( 'NONE', #8492, #31691 ) ;
#12572 = CARTESIAN_POINT ( 'NONE',  ( -35.51846793572368455, 35.99772139009146343, 7.906207997025717304 ) ) ;
#12573 = DIRECTION ( 'NONE',  ( 0.000000000000000000, 0.000000000000000000, -1.000000000000000000 ) ) ;
#12574 = CARTESIAN_POINT ( 'NONE',  ( 210.0000000000000568, 0.000000000000000000, 80.81828755692798438 ) ) ;
#12575 = VECTOR ( 'NONE', #35081, 1000.000000000000000 ) ;
#12576 = VERTEX_POINT ( 'NONE', #16366 ) ;
#12577 = CARTESIAN_POINT ( 'NONE',  ( 210.0000000000000568, 0.000000000000000000, 80.81828755692798438 ) ) ;
#12578 = CARTESIAN_POINT ( 'NONE',  ( 0.1287570809895660084, -0.3962735484563127408, 10.00000000000000000 ) ) ;
#12579 = CARTESIAN_POINT ( 'NONE',  ( -12.35406723005387875, 11.51001571518090039, 9.178419661560148768 ) ) ;
#12580 = ORIENTED_EDGE ( 'NONE', *, *, #9414, .T. ) ;
#12581 = EDGE_LOOP ( 'NONE', ( #28517, #4103, #28912, #19218, #37639, #15913, #40112, #9769 ) ) ;
#12582 = PRODUCT_CONTEXT ( 'NONE', #1417, 'mechanical' ) ;
#12583 = DIRECTION ( 'NONE',  ( 3.172065745548403743E-16, 1.000000000000000000, 0.000000000000000000 ) ) ;
#12584 = CARTESIAN_POINT ( 'NONE',  ( 0.000000000000000000, 0.000000000000000000, 10.00000000000000000 ) ) ;
#12585 = CARTESIAN_POINT ( 'NONE',  ( -126.6959734468149321, 0.000000000000000000, 165.0000000000000000 ) ) ;
#12586 = AXIS2_PLACEMENT_3D ( 'NONE', #43914, #32129, #39335 ) ;
#12587 = CARTESIAN_POINT ( 'NONE',  ( 191.5540265531851105, 0.000000000000000000, 42.56828755692798438 ) ) ;
#12588 = DIRECTION ( 'NONE',  ( 0.000000000000000000, 1.000000000000000000, 6.123233995736766036E-17 ) ) ;
#12589 = ORIENTED_EDGE ( 'NONE', *, *, #15157, .F. ) ;
#12590 = DIRECTION ( 'NONE',  ( -0.000000000000000000, -0.000000000000000000, -1.000000000000000000 ) ) ;
#12591 = AXIS2_PLACEMENT_3D ( 'NONE', #40006, #47139, #47895 ) ;
#12592 = CARTESIAN_POINT ( 'NONE',  ( 15.00000000000000000, 12.87566193687862715, -19.86060803177194956 ) ) ;
#12593 = DIRECTION ( 'NONE',  ( 0.000000000000000000, 0.000000000000000000, 1.000000000000000000 ) ) ;
#12594 = VECTOR ( 'NONE', #10220, 1000.000000000000000 ) ;
#12595 = LINE ( 'NONE', #59, #5966 ) ;
#12596 = EDGE_CURVE ( 'NONE', #11052, #39773, #28696, .T. ) ;
#12597 = AXIS2_PLACEMENT_3D ( 'NONE', #30783, #47137, #11535 ) ;
#12598 = ORIENTED_EDGE ( 'NONE', *, *, #41392, .T. ) ;
#12599 = CARTESIAN_POINT ( 'NONE',  ( 153.3040265531850537, 1.750000000000010214, -39.18171244307202983 ) ) ;
#12600 = ORIENTED_EDGE ( 'NONE', *, *, #5388, .T. ) ;
#12601 = CARTESIAN_POINT ( 'NONE',  ( -194.9999999999999432, 173.0000000000000000, 132.0000000000000000 ) ) ;
#12602 = ORIENTED_EDGE ( 'NONE', *, *, #11424, .F. ) ;
#12603 = LINE ( 'NONE', #9019, #40193 ) ;
#12604 = CARTESIAN_POINT ( 'NONE',  ( 5.888214538810389698, 16.20866436362417673, 8.727788335465566760 ) ) ;
#12605 = CARTESIAN_POINT ( 'NONE',  ( -7.241383964640739634, -3.469446951953614189E-15, 5.000000000000000000 ) ) ;
#12606 = FACE_OUTER_BOUND ( 'NONE', #42519, .T. ) ;
#12607 = ORIENTED_EDGE ( 'NONE', *, *, #7627, .F. ) ;
#12608 = VECTOR ( 'NONE', #11710, 1000.000000000000000 ) ;
#12609 = DIRECTION ( 'NONE',  ( 0.000000000000000000, 0.000000000000000000, 1.000000000000000000 ) ) ;
#12610 = DIRECTION ( 'NONE',  ( 1.860490536778032451E-50, 0.000000000000000000, -1.000000000000000000 ) ) ;
#12611 = ORIENTED_EDGE ( 'NONE', *, *, #8634, .F. ) ;
#12612 = CARTESIAN_POINT ( 'NONE',  ( 135.0000000000006253, 17.00000000000000000, -30.00000000000000000 ) ) ;
#12613 = CARTESIAN_POINT ( 'NONE',  ( -4.945973446814917018, 1.025126265847096985, -160.9317124430720014 ) ) ;
#12614 =( BOUNDED_CURVE ( )  B_SPLINE_CURVE ( 3, ( #37202, #1527, #28721, #44580 ),
 .UNSPECIFIED., .F., .F. ) 
 B_SPLINE_CURVE_WITH_KNOTS ( ( 4, 4 ),
 ( 4.712388980384689674, 6.283185307179586232 ),
 .UNSPECIFIED. ) 
 CURVE ( )  GEOMETRIC_REPRESENTATION_ITEM ( )  RATIONAL_B_SPLINE_CURVE ( ( 1.000000000000000000, 0.8047378541243649375, 0.8047378541243649375, 1.000000000000000000 ) ) 
 REPRESENTATION_ITEM ( '' )  );
#12615 = CARTESIAN_POINT ( 'NONE',  ( 1.565927753002672285, -1.491090762200744102, 9.882710035074770971 ) ) ;
#12616 = CARTESIAN_POINT ( 'NONE',  ( -8.760073316077734873, 222.4999999999999716, -228.6347188485896140 ) ) ;
#12617 = VERTEX_POINT ( 'NONE', #39986 ) ;
#12618 = VERTEX_POINT ( 'NONE', #24339 ) ;
#12619 = CARTESIAN_POINT ( 'NONE',  ( 153.2026953830863647, 103.0380105690400683, -17.46817021067766973 ) ) ;
#12620 = EDGE_LOOP ( 'NONE', ( #12991, #38558, #30169, #36581, #36706, #41099, #152, #47658 ) ) ;
#12621 = DIRECTION ( 'NONE',  ( -1.000000000000000000, 0.000000000000000000, 0.000000000000000000 ) ) ;
#12622 = CARTESIAN_POINT ( 'NONE',  ( -87.72109971266203843, -1.750000000000009548, 41.84341382277508359 ) ) ;
#12623 = AXIS2_PLACEMENT_3D ( 'NONE', #1342, #37019, #29287 ) ;
#12624 = VECTOR ( 'NONE', #8667, 1000.000000000000114 ) ;
#12625 = DIRECTION ( 'NONE',  ( 0.000000000000000000, 0.000000000000000000, -1.000000000000000000 ) ) ;
#12626 = ORIENTED_EDGE ( 'NONE', *, *, #30625, .F. ) ;
#12627 = CARTESIAN_POINT ( 'NONE',  ( -5.000000000000000000, 165.2000000000000171, -359.8000000000002387 ) ) ;
#12628 = ADVANCED_FACE ( 'NONE', ( #26341 ), #9923, .T. ) ;
#12629 = CARTESIAN_POINT ( 'NONE',  ( -84.94597344681494633, 2.143131898507880377E-16, 159.0682875569279702 ) ) ;
#12630 = VECTOR ( 'NONE', #8238, 1000.000000000000000 ) ;
#12631 = EDGE_CURVE ( 'NONE', #48700, #34291, #25836, .T. ) ;
#12632 = PLANE ( 'NONE',  #29185 ) ;
#12633 = EDGE_CURVE ( 'NONE', #45598, #15451, #6583, .T. ) ;
#12634 = CARTESIAN_POINT ( 'NONE',  ( -1.066995270233474624, 33.23888904628638841, -3.760136334089591248 ) ) ;
#12635 = EDGE_LOOP ( 'NONE', ( #14524, #27363, #36284, #34942, #141, #21201, #25703, #27988 ) ) ;
#12636 = ORIENTED_EDGE ( 'NONE', *, *, #24457, .T. ) ;
#12637 = ORIENTED_EDGE ( 'NONE', *, *, #16431, .F. ) ;
#12638 = CARTESIAN_POINT ( 'NONE',  ( 177.5000000000000284, -112.5000000000000000, -10.00000000000000000 ) ) ;
#12639 =( NAMED_UNIT ( * ) SI_UNIT ( $, .STERADIAN. ) SOLID_ANGLE_UNIT ( ) );
#12640 = ADVANCED_FACE ( 'NONE', ( #38158 ), #18123, .F. ) ;
#12641 = DIRECTION ( 'NONE',  ( -0.000000000000000000, -0.9749645535258953943, 0.2223603367690637489 ) ) ;
#12642 = EDGE_CURVE ( 'NONE', #38442, #37949, #1594, .T. ) ;
#12643 = ORIENTED_EDGE ( 'NONE', *, *, #29778, .T. ) ;
#12644 = DIRECTION ( 'NONE',  ( -1.000000000000000000, -0.000000000000000000, -0.000000000000000000 ) ) ;
#12645 = ORIENTED_EDGE ( 'NONE', *, *, #23388, .F. ) ;
#12646 = CARTESIAN_POINT ( 'NONE',  ( 0.3862712429686894766, -1.188820645368940276, 10.00000000000000000 ) ) ;
#12647 = ORIENTED_EDGE ( 'NONE', *, *, #49194, .T. ) ;
#12648 = EDGE_CURVE ( 'NONE', #35861, #25110, #50386, .T. ) ;
#12649 = CARTESIAN_POINT ( 'NONE',  ( 1.249999999999999778, 0.000000000000000000, 9.972675548442463622 ) ) ;
#12650 = CARTESIAN_POINT ( 'NONE',  ( -210.0000000000000568, 0.000000000000000000, -159.1817124430720298 ) ) ;
#12651 = DIRECTION ( 'NONE',  ( 0.000000000000000000, 1.000000000000000000, 0.000000000000000000 ) ) ;
#12652 = PLANE ( 'NONE',  #34799 ) ;
#12653 = AXIS2_PLACEMENT_3D ( 'NONE', #8577, #7823, #43211 ) ;
#12654 = CARTESIAN_POINT ( 'NONE',  ( -2.052581215100349521, 0.2042358160481012597, 9.886433018048073507 ) ) ;
#12655 = ORIENTED_EDGE ( 'NONE', *, *, #20197, .T. ) ;
#12656 = DIRECTION ( 'NONE',  ( -3.172065784643302499E-16, -1.000000000000000000, 0.000000000000000000 ) ) ;
#12657 = CARTESIAN_POINT ( 'NONE',  ( 195.0540265531851105, 2.143131898507880377E-16, 122.5682875569279702 ) ) ;
#12658 = CARTESIAN_POINT ( 'NONE',  ( -6.604186672497962540, 1.848482776016375340, 9.753789706659947711 ) ) ;
#12659 = EDGE_CURVE ( 'NONE', #34063, #33842, #22857, .T. ) ;
#12660 = EDGE_CURVE ( 'NONE', #32832, #9482, #10181, .T. ) ;
#12661 = EDGE_CURVE ( 'NONE', #23671, #21333, #6335, .T. ) ;
#12662 = ADVANCED_FACE ( 'NONE', ( #5826 ), #49384, .T. ) ;
#12663 = VERTEX_POINT ( 'NONE', #33539 ) ;
#12664 = VECTOR ( 'NONE', #21781, 1000.000000000000000 ) ;
#12665 = DIRECTION ( 'NONE',  ( 1.000000000000000000, 0.000000000000000000, 0.000000000000000000 ) ) ;
#12666 = EDGE_CURVE ( 'NONE', #25919, #7318, #37909, .T. ) ;
#12667 = ORIENTED_EDGE ( 'NONE', *, *, #45529, .T. ) ;
#12668 = LINE ( 'NONE', #1142, #29498 ) ;
#12669 = EDGE_CURVE ( 'NONE', #3854, #8266, #14016, .T. ) ;
#12670 = LINE ( 'NONE', #36561, #140 ) ;
#12671 = AXIS2_PLACEMENT_3D ( 'NONE', #16315, #28117, #24279 ) ;
#12672 = ORIENTED_EDGE ( 'NONE', *, *, #10808, .T. ) ;
#12673 =( BOUNDED_CURVE ( )  B_SPLINE_CURVE ( 3, ( #34843, #15332, #190, #32245 ),
 .UNSPECIFIED., .F., .F. ) 
 B_SPLINE_CURVE_WITH_KNOTS ( ( 4, 4 ),
 ( 4.712388980384689674, 6.283185307179586232 ),
 .UNSPECIFIED. ) 
 CURVE ( )  GEOMETRIC_REPRESENTATION_ITEM ( )  RATIONAL_B_SPLINE_CURVE ( ( 1.000000000000000000, 0.8047378541243649375, 0.8047378541243649375, 1.000000000000000000 ) ) 
 REPRESENTATION_ITEM ( '' )  );
#12674 = DIRECTION ( 'NONE',  ( 0.000000000000000000, -1.000000000000000000, -3.186989995019654210E-49 ) ) ;
#12675 = DIRECTION ( 'NONE',  ( 0.000000000000000000, 0.000000000000000000, -1.000000000000000000 ) ) ;
#12676 = CARTESIAN_POINT ( 'NONE',  ( -15.00099850811941948, -7.462898891544107016, 9.403735324607438884 ) ) ;
#12677 = CARTESIAN_POINT ( 'NONE',  ( 181.0000000000000000, -164.9999999999999432, -340.0000000000001705 ) ) ;
#12678 =( BOUNDED_CURVE ( )  B_SPLINE_CURVE ( 3, ( #12849, #8251, #23392, #3885 ),
 .UNSPECIFIED., .F., .F. ) 
 B_SPLINE_CURVE_WITH_KNOTS ( ( 4, 4 ),
 ( 4.712388980384689674, 6.283185307179586232 ),
 .UNSPECIFIED. ) 
 CURVE ( )  GEOMETRIC_REPRESENTATION_ITEM ( )  RATIONAL_B_SPLINE_CURVE ( ( 1.000000000000000000, 0.8047378541243649375, 0.8047378541243649375, 1.000000000000000000 ) ) 
 REPRESENTATION_ITEM ( '' )  );
#12679 = ORIENTED_EDGE ( 'NONE', *, *, #18678, .T. ) ;
#12680 = ORIENTED_EDGE ( 'NONE', *, *, #32509, .T. ) ;
#12681 = EDGE_CURVE ( 'NONE', #8852, #49105, #9862, .T. ) ;
#12682 = DIRECTION ( 'NONE',  ( -1.000000000000000000, -0.000000000000000000, -0.000000000000000000 ) ) ;
#12683 = CARTESIAN_POINT ( 'NONE',  ( 48.34672127938079456, -13.00749071703866555, 3.199614146704519602 ) ) ;
#12684 = AXIS2_PLACEMENT_3D ( 'NONE', #17409, #33576, #14307 ) ;
#12685 = ADVANCED_FACE ( 'NONE', ( #49134 ), #34050, .F. ) ;
#12686 = EDGE_LOOP ( 'NONE', ( #4023, #47082, #29661, #22757 ) ) ;
#12687 = EDGE_CURVE ( 'NONE', #14142, #50479, #45297, .T. ) ;
#12688 = ORIENTED_EDGE ( 'NONE', *, *, #6036, .T. ) ;
#12689 = CARTESIAN_POINT ( 'NONE',  ( 28.96803024440893992, 18.11533787072037072, 7.455576670931136185 ) ) ;
#12690 = CARTESIAN_POINT ( 'NONE',  ( 166.9999999999999716, -272.4999999999999432, -343.9999999999987494 ) ) ;
#12691 = CARTESIAN_POINT ( 'NONE',  ( -9.999999999999998224, 8.486842105263161073, 18.34680996553531784 ) ) ;
#12692 = CARTESIAN_POINT ( 'NONE',  ( 360.0000000000001137, 183.3431457505076594, 358.3431457505074604 ) ) ;
#12693 = VERTEX_POINT ( 'NONE', #6837 ) ;
#12694 = AXIS2_PLACEMENT_3D ( 'NONE', #46196, #22885, #3123 ) ;
#12695 = ORIENTED_EDGE ( 'NONE', *, *, #38597, .T. ) ;
#12696 = ADVANCED_FACE ( 'NONE', ( #33038 ), #17624, .T. ) ;
#12697 = ORIENTED_EDGE ( 'NONE', *, *, #48838, .F. ) ;
#12698 = B_SPLINE_CURVE_WITH_KNOTS ( 'NONE', 3,
 ( #4056, #23035, #27153, #15853 ),
 .UNSPECIFIED., .F., .F.,
 ( 4, 4 ),
 ( 0.000000000000000000, 0.002217981418793440844 ),
 .UNSPECIFIED. ) ;
#12699 = ADVANCED_FACE ( 'NONE', ( #38655 ), #50647, .T. ) ;
#12700 = CARTESIAN_POINT ( 'NONE',  ( -3.087186397306470820, -2.514307945609864259, -2.642742795433417058E-16 ) ) ;
#12701 = VECTOR ( 'NONE', #29089, 1000.000000000000000 ) ;
#12702 = ORIENTED_EDGE ( 'NONE', *, *, #49676, .T. ) ;
#12703 = ORIENTED_EDGE ( 'NONE', *, *, #40307, .T. ) ;
#12704 = CARTESIAN_POINT ( 'NONE',  ( -1.035950918207909632, -50.00000000000000711, -2.408242355805840784 ) ) ;
#12705 = CARTESIAN_POINT ( 'NONE',  ( 111.5540265531850537, 1.025126265847081886, -40.93171244307202272 ) ) ;
#12706 =( GEOMETRIC_REPRESENTATION_CONTEXT ( 3 ) GLOBAL_UNCERTAINTY_ASSIGNED_CONTEXT ( ( #46464 ) ) GLOBAL_UNIT_ASSIGNED_CONTEXT ( ( #48263, #45433, #26471 ) ) REPRESENTATION_CONTEXT ( 'NONE', 'WORKASPACE' ) );
#12707 = ORIENTED_EDGE ( 'NONE', *, *, #43107, .F. ) ;
#12708 = ORIENTED_EDGE ( 'NONE', *, *, #25844, .F. ) ;
#12709 = AXIS2_PLACEMENT_3D ( 'NONE', #42931, #3942, #111 ) ;
#12710 = EDGE_CURVE ( 'NONE', #49781, #8266, #42236, .T. ) ;
#12711 = DIRECTION ( 'NONE',  ( 0.000000000000000000, 0.000000000000000000, -1.000000000000000000 ) ) ;
#12712 = VERTEX_POINT ( 'NONE', #15551 ) ;
#12713 = CARTESIAN_POINT ( 'NONE',  ( -166.6959734468149463, 0.000000000000000000, 165.0000000000000000 ) ) ;
#12714 = CARTESIAN_POINT ( 'NONE',  ( -206.6959734468149463, 1.750000000000010658, 120.8182875569279702 ) ) ;
#12715 = CARTESIAN_POINT ( 'NONE',  ( 168.9999999999999716, -93.49999999999998579, -350.0000000000001705 ) ) ;
#12716 = EDGE_CURVE ( 'NONE', #835, #44977, #31462, .T. ) ;
#12717 = FACE_OUTER_BOUND ( 'NONE', #43851, .T. ) ;
#12718 = ORIENTED_EDGE ( 'NONE', *, *, #6252, .F. ) ;
#12719 = PLANE ( 'NONE',  #14395 ) ;
#12720 = CARTESIAN_POINT ( 'NONE',  ( 34.32915281903212446, -1.750000000000009548, -118.1565861772249519 ) ) ;
#12721 = CARTESIAN_POINT ( 'NONE',  ( -7.398363427652414614, 15.19415887381139108, -9.008049429158100807 ) ) ;
#12722 = CARTESIAN_POINT ( 'NONE',  ( 0.4183568061215536815, -10.00547810715653618, 6.429802539306306741 ) ) ;
#12723 = EDGE_CURVE ( 'NONE', #46038, #11473, #33067, .T. ) ;
#12724 = AXIS2_PLACEMENT_3D ( 'NONE', #337, #47733, #47486 ) ;
#12725 = EDGE_CURVE ( 'NONE', #5511, #31646, #7867, .T. ) ;
#12726 = VECTOR ( 'NONE', #32276, 1000.000000000000227 ) ;
#12727 = EDGE_CURVE ( 'NONE', #33842, #40358, #41893, .T. ) ;
#12728 = DIRECTION ( 'NONE',  ( -1.000000000000000000, 0.000000000000000000, 0.000000000000000000 ) ) ;
#12729 = EDGE_CURVE ( 'NONE', #1016, #46409, #46803, .T. ) ;
#12730 = CIRCLE ( 'NONE', #43047, 4.000000000000003553 ) ;
#12731 = CARTESIAN_POINT ( 'NONE',  ( -164.4973046169135955, -98.56198943095992604, 23.74256005001722158 ) ) ;
#12732 = CARTESIAN_POINT ( 'NONE',  ( 1.540571744149447309, -1.371626741452957488, 9.889206917020304743 ) ) ;
#12733 = ADVANCED_FACE ( 'NONE', ( #38407 ), #42723, .F. ) ;
#12734 = ORIENTED_EDGE ( 'NONE', *, *, #44738, .T. ) ;
#12735 = CARTESIAN_POINT ( 'NONE',  ( -7.749480817862350435, -14.85497772329513211, 9.403735324607438884 ) ) ;
#12736 = AXIS2_PLACEMENT_3D ( 'NONE', #2987, #18632, #22991 ) ;
#12737 = CARTESIAN_POINT ( 'NONE',  ( 154.3291528190321458, 1.750000000000009548, 41.84341382277508359 ) ) ;
#12738 = AXIS2_PLACEMENT_3D ( 'NONE', #41734, #41986, #41483 ) ;
#12739 = EDGE_LOOP ( 'NONE', ( #38201, #21263, #26940, #38391 ) ) ;
#12740 = CARTESIAN_POINT ( 'NONE',  ( -86.69597344681496054, 0.000000000000000000, 165.0000000000000000 ) ) ;
#12741 = CARTESIAN_POINT ( 'NONE',  ( 75.05402655318509630, 2.143131898507880377E-16, 2.568287556928006143 ) ) ;
#12742 = DIRECTION ( 'NONE',  ( 0.000000000000000000, 0.000000000000000000, -1.000000000000000000 ) ) ;
#12743 = ORIENTED_EDGE ( 'NONE', *, *, #24046, .F. ) ;
#12744 = CARTESIAN_POINT ( 'NONE',  ( 195.0540265531851105, 2.143131898507880377E-16, -117.4317124430720725 ) ) ;
#12745 = ORIENTED_EDGE ( 'NONE', *, *, #30361, .T. ) ;
#12746 = VERTEX_POINT ( 'NONE', #11962 ) ;
#12747 = VECTOR ( 'NONE', #11218, 1000.000000000000000 ) ;
#12748 = CARTESIAN_POINT ( 'NONE',  ( -4.207128120815918256E-14, 3.058192377181588826E-14, 10.00000000000000000 ) ) ;
#12749 = FACE_OUTER_BOUND ( 'NONE', #10978, .T. ) ;
#12750 = EDGE_LOOP ( 'NONE', ( #26872, #36251, #33828, #22671 ) ) ;
#12751 = ADVANCED_FACE ( 'NONE', ( #3744 ), #39425, .T. ) ;
#12752 = DIRECTION ( 'NONE',  ( -1.000000000000000000, 0.000000000000000000, 2.312964634635864737E-16 ) ) ;
#12753 = CYLINDRICAL_SURFACE ( 'NONE', #18365, 2.000000000000001776 ) ;
#12754 = EDGE_LOOP ( 'NONE', ( #34695, #6486, #49550 ) ) ;
#12755 = VERTEX_POINT ( 'NONE', #11204 ) ;
#12756 = CARTESIAN_POINT ( 'NONE',  ( -4.945973446814903696, 2.143131898507912917E-16, -80.93171244307204404 ) ) ;
#12757 = ORIENTED_EDGE ( 'NONE', *, *, #47146, .T. ) ;
#12758 = CARTESIAN_POINT ( 'NONE',  ( 339.9999999999999432, 175.0000000000000284, -106.0000000000001990 ) ) ;
#12759 = CARTESIAN_POINT ( 'NONE',  ( -86.69597344681494633, -1.750000000000010658, -119.1817124430720440 ) ) ;
#12760 = CARTESIAN_POINT ( 'NONE',  ( 80.00000000000028422, 17.00000000000000000, -84.99999999999998579 ) ) ;
#12761 = AXIS2_PLACEMENT_3D ( 'NONE', #30166, #25133, #1024 ) ;
#12762 = ORIENTED_EDGE ( 'NONE', *, *, #20315, .T. ) ;
#12763 = DIRECTION ( 'NONE',  ( 1.000000000000000000, 0.000000000000000000, -0.000000000000000000 ) ) ;
#12764 = CARTESIAN_POINT ( 'NONE',  ( -88.44597344681497475, 0.000000000000000000, -77.43171244307198720 ) ) ;
#12765 = VERTEX_POINT ( 'NONE', #19394 ) ;
#12766 = VECTOR ( 'NONE', #26582, 1000.000000000000000 ) ;
#12767 = ORIENTED_EDGE ( 'NONE', *, *, #13290, .F. ) ;
#12768 = VERTEX_POINT ( 'NONE', #22980 ) ;
#12769 = CARTESIAN_POINT ( 'NONE',  ( 210.0000000000000568, 0.000000000000000000, -79.18171244307201562 ) ) ;
#12770 = EDGE_CURVE ( 'NONE', #48741, #10841, #30347, .T. ) ;
#12771 = CARTESIAN_POINT ( 'NONE',  ( 22.69295089195473025, 45.31600496604705341, 7.455576670931136185 ) ) ;
#12772 = ORIENTED_EDGE ( 'NONE', *, *, #1865, .T. ) ;
#12773 = CARTESIAN_POINT ( 'NONE',  ( -27.33593271309441519, 41.94268121623345991, -9.367992836599954742 ) ) ;
#12774 = DIRECTION ( 'NONE',  ( -1.000000000000000000, 0.000000000000000000, 0.000000000000000000 ) ) ;
#12775 = DIRECTION ( 'NONE',  ( -0.000000000000000000, -0.000000000000000000, -1.000000000000000000 ) ) ;
#12776 = VECTOR ( 'NONE', #49440, 1000.000000000000000 ) ;
#12777 = CARTESIAN_POINT ( 'NONE',  ( 113.3040265531850537, -1.749999999999996891, -159.1817124430720298 ) ) ;
#12778 = DIRECTION ( 'NONE',  ( 0.000000000000000000, -2.537652627714643577E-15, -1.000000000000000000 ) ) ;
#12779 = AXIS2_PLACEMENT_3D ( 'NONE', #797, #44122, #35458 ) ;
#12780 = CARTESIAN_POINT ( 'NONE',  ( -86.69597344681494633, -1.750000000000010658, 80.81828755692798438 ) ) ;
#12781 = DIRECTION ( 'NONE',  ( 0.000000000000000000, 0.000000000000000000, 1.000000000000000000 ) ) ;
#12782 = CARTESIAN_POINT ( 'NONE',  ( 33.30402655318503946, 1.750000000000010658, 120.8182875569279702 ) ) ;
#12783 = LINE ( 'NONE', #5071, #30982 ) ;
#12784 = VECTOR ( 'NONE', #33716, 1000.000000000000000 ) ;
#12785 = CARTESIAN_POINT ( 'NONE',  ( -177.4999999999999716, 57.49999999999996447, -9.999999999999973355 ) ) ;
#12786 = UNCERTAINTY_MEASURE_WITH_UNIT (LENGTH_MEASURE( 1.000000000000000082E-05 ), #47510, 'distance_accuracy_value', 'NONE');
#12787 = ADVANCED_FACE ( 'NONE', ( #49870 ), #11697, .F. ) ;
#12788 = EDGE_CURVE ( 'NONE', #36968, #47621, #30439, .T. ) ;
#12789 = FACE_OUTER_BOUND ( 'NONE', #5217, .T. ) ;
#12790 = ORIENTED_EDGE ( 'NONE', *, *, #39821, .F. ) ;
#12791 = CARTESIAN_POINT ( 'NONE',  ( 5.551115123125782702E-14, -180.9999999999999716, 343.9999999999997726 ) ) ;
#12792 = EDGE_CURVE ( 'NONE', #49743, #11508, #162, .T. ) ;
#12793 = CARTESIAN_POINT ( 'NONE',  ( 0.9341213539222221751, 1.950087977540064577, 9.885585981620945262 ) ) ;
#12794 = CARTESIAN_POINT ( 'NONE',  ( 49.46074318306830975, -9.578883844006831794, 8.807470649214879543 ) ) ;
#12795 = CARTESIAN_POINT ( 'NONE',  ( 55.00000000000002132, 52.49999999999999289, 5.000000000000000000 ) ) ;
#12796 = EDGE_CURVE ( 'NONE', #38055, #48807, #10932, .T. ) ;
#12797 = EDGE_CURVE ( 'NONE', #48563, #34745, #34549, .T. ) ;
#12798 = VERTEX_POINT ( 'NONE', #4754 ) ;
#12799 = VECTOR ( 'NONE', #43484, 1000.000000000000000 ) ;
#12800 = DIRECTION ( 'NONE',  ( -1.000000000000000000, 0.000000000000000000, 0.000000000000000000 ) ) ;
#12801 = AXIS2_PLACEMENT_3D ( 'NONE', #38776, #7210, #15414 ) ;
#12802 = LINE ( 'NONE', #5086, #23752 ) ;
#12803 = ORIENTED_EDGE ( 'NONE', *, *, #27754, .F. ) ;
#12804 = CARTESIAN_POINT ( 'NONE',  ( 50.11058929355270664, -7.578863168071591438, 7.455576670931136185 ) ) ;
#12805 = CARTESIAN_POINT ( 'NONE',  ( 74.32915281903215998, -1.750000000000010436, -120.2068387089191219 ) ) ;
#12806 = CARTESIAN_POINT ( 'NONE',  ( 111.5540265531850679, 0.000000000000000000, -157.4317124430720582 ) ) ;
#12807 = ADVANCED_FACE ( 'NONE', ( #35577 ), #20396, .F. ) ;
#12808 = ORIENTED_EDGE ( 'NONE', *, *, #7538, .T. ) ;
#12809 = CARTESIAN_POINT ( 'NONE',  ( 185.0000000000000284, -174.9999999999999716, -111.0000000000001563 ) ) ;
#12810 = ORIENTED_EDGE ( 'NONE', *, *, #14396, .T. ) ;
#12811 = ORIENTED_EDGE ( 'NONE', *, *, #38113, .T. ) ;
#12812 = VECTOR ( 'NONE', #16873, 1000.000000000000000 ) ;
#12813 = ORIENTED_EDGE ( 'NONE', *, *, #10169, .T. ) ;
#12814 = FACE_OUTER_BOUND ( 'NONE', #40158, .T. ) ;
#12815 = CARTESIAN_POINT ( 'NONE',  ( -14.48769039275601145, -30.44468701195584970, 8.807470649214879543 ) ) ;
#12816 = COLOUR_RGB ( '',0.7921568627450980005, 0.8196078431372548767, 0.9333333333333333481 ) ;
#12817 = ORIENTED_EDGE ( 'NONE', *, *, #16180, .F. ) ;
#12818 = CYLINDRICAL_SURFACE ( 'NONE', #13129, 1.750000000000015543 ) ;
#12819 = FACE_OUTER_BOUND ( 'NONE', #27957, .T. ) ;
#12820 = CARTESIAN_POINT ( 'NONE',  ( -164.9999999999981526, 17.00000000000000000, 65.00000000000000000 ) ) ;
#12821 = CARTESIAN_POINT ( 'NONE',  ( -25.63461350838931452, 43.17876197216397571, -8.016098858316205167 ) ) ;
#12822 = EDGE_LOOP ( 'NONE', ( #42067, #21206 ) ) ;
#12823 = AXIS2_PLACEMENT_3D ( 'NONE', #3915, #31389, #46980 ) ;
#12824 = DIRECTION ( 'NONE',  ( 0.000000000000000000, -0.000000000000000000, -1.000000000000000000 ) ) ;
#12825 =( BOUNDED_CURVE ( )  B_SPLINE_CURVE ( 3, ( #14024, #32796, #33553, #29685 ),
 .UNSPECIFIED., .F., .F. ) 
 B_SPLINE_CURVE_WITH_KNOTS ( ( 4, 4 ),
 ( 4.712388980384689674, 6.283185307179586232 ),
 .UNSPECIFIED. ) 
 CURVE ( )  GEOMETRIC_REPRESENTATION_ITEM ( )  RATIONAL_B_SPLINE_CURVE ( ( 1.000000000000000000, 0.8047378541243649375, 0.8047378541243649375, 1.000000000000000000 ) ) 
 REPRESENTATION_ITEM ( '' )  );
#12826 = ORIENTED_EDGE ( 'NONE', *, *, #23878, .T. ) ;
#12827 = CARTESIAN_POINT ( 'NONE',  ( 154.3291528190321458, -1.750000000000009548, -38.15658617722494483 ) ) ;
#12828 = ORIENTED_EDGE ( 'NONE', *, *, #19528, .T. ) ;
#12829 = DIRECTION ( 'NONE',  ( 0.000000000000000000, 0.000000000000000000, 1.000000000000000000 ) ) ;
#12830 = CARTESIAN_POINT ( 'NONE',  ( 50.24128791297869867, 41.04536285977714982, -5.000000000000000000 ) ) ;
#12831 = ORIENTED_EDGE ( 'NONE', *, *, #5906, .F. ) ;
#12832 = EDGE_CURVE ( 'NONE', #11124, #8521, #6830, .T. ) ;
#12833 = CARTESIAN_POINT ( 'NONE',  ( 46.76852358249013264, -17.86468378716708827, -9.367992836599951190 ) ) ;
#12834 = CARTESIAN_POINT ( 'NONE',  ( -165.0000000000000284, 16.00000000000000000, 115.0000000000000142 ) ) ;
#12835 = CARTESIAN_POINT ( 'NONE',  ( -44.94597344681493922, 2.143131898507880377E-16, -80.93171244307204404 ) ) ;
#12836 = CARTESIAN_POINT ( 'NONE',  ( 195.0540265531851105, 1.025126265847089435, 159.0682875569279418 ) ) ;
#12837 = VECTOR ( 'NONE', #16614, 1000.000000000000000 ) ;
#12838 = ORIENTED_EDGE ( 'NONE', *, *, #44460, .T. ) ;
#12839 = CARTESIAN_POINT ( 'NONE',  ( -2.052570692346794790, 0.2041439924650417514, 9.889206917020306520 ) ) ;
#12840 =( BOUNDED_CURVE ( )  B_SPLINE_CURVE ( 3, ( #17557, #44973, #9850, #5998 ),
 .UNSPECIFIED., .F., .F. ) 
 B_SPLINE_CURVE_WITH_KNOTS ( ( 4, 4 ),
 ( 0.000000000000000000, 1.570796326794896558 ),
 .UNSPECIFIED. ) 
 CURVE ( )  GEOMETRIC_REPRESENTATION_ITEM ( )  RATIONAL_B_SPLINE_CURVE ( ( 1.000000000000000000, 0.8047378541243649375, 0.8047378541243649375, 1.000000000000000000 ) ) 
 REPRESENTATION_ITEM ( '' )  );
#12841 = CARTESIAN_POINT ( 'NONE',  ( -5.000000000000000000, 165.2000000000000171, 340.1999999999997044 ) ) ;
#12842 = VERTEX_POINT ( 'NONE', #413 ) ;
#12843 = VERTEX_POINT ( 'NONE', #8615 ) ;
#12844 = SHAPE_DEFINITION_REPRESENTATION ( #18341, #41838 ) ;
#12845 = CARTESIAN_POINT ( 'NONE',  ( -165.2900739183569954, 54.43801056904003133, -18.55102910462098365 ) ) ;
#12846 = CYLINDRICAL_SURFACE ( 'NONE', #18474, 0.5000000000000004441 ) ;
#12847 = DIRECTION ( 'NONE',  ( 1.000000000000000000, 0.000000000000000000, 0.000000000000000000 ) ) ;
#12848 = DIRECTION ( 'NONE',  ( -0.000000000000000000, -0.000000000000000000, -1.000000000000000000 ) ) ;
#12849 = CARTESIAN_POINT ( 'NONE',  ( 153.3040265531850537, -1.750000000000010658, -119.1817124430720440 ) ) ;
#12850 = VERTEX_POINT ( 'NONE', #16061 ) ;
#12851 = CARTESIAN_POINT ( 'NONE',  ( -4.999999999999997335, 214.9999999999999716, -234.7500000000000000 ) ) ;
#12852 = CARTESIAN_POINT ( 'NONE',  ( 350.0000000000000000, -182.9999999999999716, -344.0000000000001705 ) ) ;
#12853 = CARTESIAN_POINT ( 'NONE',  ( -0.5386300094813477601, 1.098626330213929636, 9.993783931180534097 ) ) ;
#12854 = CARTESIAN_POINT ( 'NONE',  ( -48.44597344681496054, 1.025126265847089657, 79.06828755692797017 ) ) ;
#12855 = VECTOR ( 'NONE', #47612, 1000.000000000000000 ) ;
#12856 = EDGE_CURVE ( 'NONE', #11949, #14610, #660, .T. ) ;
#12857 = ADVANCED_FACE ( 'NONE', ( #20150 ), #12449, .T. ) ;
#12858 = ORIENTED_EDGE ( 'NONE', *, *, #29293, .T. ) ;
#12859 = CARTESIAN_POINT ( 'NONE',  ( -44.94597344681493922, 2.143131898507880377E-16, -0.9317124430720247208 ) ) ;
#12860 = EDGE_LOOP ( 'NONE', ( #35370, #8864, #40956, #45795, #19166 ) ) ;
#12861 = CARTESIAN_POINT ( 'NONE',  ( 115.0540265531850395, 2.143131898507847836E-16, -40.93171244307202983 ) ) ;
#12862 = VERTEX_POINT ( 'NONE', #16562 ) ;
#12863 = EDGE_CURVE ( 'NONE', #4897, #5706, #4258, .T. ) ;
#12864 = FACE_OUTER_BOUND ( 'NONE', #18188, .T. ) ;
#12865 = LINE ( 'NONE', #28772, #38883 ) ;
#12866 = CARTESIAN_POINT ( 'NONE',  ( 344.0000000000000000, -165.0000000000001137, 340.0000000000000568 ) ) ;
#12867 = LINE ( 'NONE', #43648, #3374 ) ;
#12868 = ORIENTED_EDGE ( 'NONE', *, *, #13491, .T. ) ;
#12869 = DIRECTION ( 'NONE',  ( -1.000000000000000000, -0.000000000000000000, -0.000000000000000000 ) ) ;
#12870 = VECTOR ( 'NONE', #47632, 1000.000000000000000 ) ;
#12871 = ORIENTED_EDGE ( 'NONE', *, *, #45666, .T. ) ;
#12872 = DIRECTION ( 'NONE',  ( 0.000000000000000000, 0.000000000000000000, 1.000000000000000000 ) ) ;
#12873 = CARTESIAN_POINT ( 'NONE',  ( -126.6959734468149321, -1.749999999999996891, 0.8182875569279768335 ) ) ;
#12874 = CARTESIAN_POINT ( 'NONE',  ( 0.1287570809895575430, 0.3962735484563150168, 10.00000000000000000 ) ) ;
#12875 = CARTESIAN_POINT ( 'NONE',  ( -1.540617191852276413, 1.371546265746164783, 9.891980816076525684 ) ) ;
#12876 = ORIENTED_EDGE ( 'NONE', *, *, #36167, .F. ) ;
#12877 = VERTEX_POINT ( 'NONE', #19894 ) ;
#12878 = DIRECTION ( 'NONE',  ( 0.000000000000000000, -1.000000000000000000, -1.544785076050074834E-48 ) ) ;
#12879 = ORIENTED_EDGE ( 'NONE', *, *, #6114, .F. ) ;
#12880 = CARTESIAN_POINT ( 'NONE',  ( 164.9999999999999716, 16.00000000000000000, 115.0000000000000142 ) ) ;
#12881 = ORIENTED_EDGE ( 'NONE', *, *, #14596, .T. ) ;
#12882 = FACE_OUTER_BOUND ( 'NONE', #49322, .T. ) ;
#12883 = CARTESIAN_POINT ( 'NONE',  ( 183.0000000000000000, -174.9999999999999716, -344.0000000000001137 ) ) ;
#12884 = B_SPLINE_SURFACE_WITH_KNOTS ( 'NONE', 3, 3, ( 
 ( #6932, #22573, #41823, #2565 ),
 ( #49976, #29270, #41072, #18209 ),
 ( #5913, #37255, #6667, #33390 ),
 ( #17956, #48962, #13850, #25680 ) ),
 .UNSPECIFIED., .F., .F., .F.,
 ( 4, 4 ),
 ( 4, 4 ),
 ( 0.000000000000000000, 1.000000000000000000 ),
 ( 0.000000000000000000, 1.000000000000000000 ),
 .UNSPECIFIED. ) ;
#12885 = LINE ( 'NONE', #32399, #16951 ) ;
#12886 = EDGE_CURVE ( 'NONE', #31206, #41298, #27686, .T. ) ;
#12887 = FACE_OUTER_BOUND ( 'NONE', #26069, .T. ) ;
#12888 = FACE_OUTER_BOUND ( 'NONE', #4674, .T. ) ;
#12889 = PLANE ( 'NONE',  #15753 ) ;
#12890 = ORIENTED_EDGE ( 'NONE', *, *, #21435, .F. ) ;
#12891 = VERTEX_POINT ( 'NONE', #47313 ) ;
#12892 = ORIENTED_EDGE ( 'NONE', *, *, #8028, .T. ) ;
#12893 = LINE ( 'NONE', #5200, #45133 ) ;
#12894 = DIRECTION ( 'NONE',  ( -0.000000000000000000, -1.000000000000000000, -0.000000000000000000 ) ) ;
#12895 = CARTESIAN_POINT ( 'NONE',  ( -1.387778780781445676E-14, -6.938893903907228378E-14, 978.4685478195414134 ) ) ;
#12896 = CARTESIAN_POINT ( 'NONE',  ( -208.1473046169136580, 2.688010569040066411, 472.8425600500171981 ) ) ;
#12897 = EDGE_LOOP ( 'NONE', ( #13725, #17754, #21507, #18547, #30438 ) ) ;
#12898 = CARTESIAN_POINT ( 'NONE',  ( -168.4459734468149747, 1.025126265847089435, -40.93171244307204404 ) ) ;
#12899 = ORIENTED_EDGE ( 'NONE', *, *, #5507, .F. ) ;
#12900 = CARTESIAN_POINT ( 'NONE',  ( 80.00000000000028422, 16.00000000000000000, -84.99999999999998579 ) ) ;
#12901 = LINE ( 'NONE', #36541, #31793 ) ;
#12902 = CARTESIAN_POINT ( 'NONE',  ( -44.94597344681493922, 2.143131898507880377E-16, -117.4317124430720156 ) ) ;
#12903 = AXIS2_PLACEMENT_3D ( 'NONE', #16070, #35846, #24785 ) ;
#12904 = CARTESIAN_POINT ( 'NONE',  ( 344.0000000000000568, 167.0000000000000000, 341.9999999999998295 ) ) ;
#12905 = CARTESIAN_POINT ( 'NONE',  ( 7.499999999999948486, -194.9999999999999716, -224.9999999999999716 ) ) ;
#12906 = CARTESIAN_POINT ( 'NONE',  ( 36.08557433729230723, -35.58569447144768105, 7.455576670931136185 ) ) ;
#12907 = ORIENTED_EDGE ( 'NONE', *, *, #46643, .F. ) ;
#12908 = LINE ( 'NONE', #44199, #29640 ) ;
#12909 = PLANE ( 'NONE',  #3964 ) ;
#12910 = DIRECTION ( 'NONE',  ( 0.000000000000000000, 0.000000000000000000, -1.000000000000000000 ) ) ;
#12911 = ORIENTED_EDGE ( 'NONE', *, *, #35342, .T. ) ;
#12912 =( BOUNDED_CURVE ( )  B_SPLINE_CURVE ( 3, ( #20187, #42510, #7386, #5800 ),
 .UNSPECIFIED., .F., .F. ) 
 B_SPLINE_CURVE_WITH_KNOTS ( ( 4, 4 ),
 ( 4.712388980384689674, 6.283185307179586232 ),
 .UNSPECIFIED. ) 
 CURVE ( )  GEOMETRIC_REPRESENTATION_ITEM ( )  RATIONAL_B_SPLINE_CURVE ( ( 1.000000000000000000, 0.8047378541243649375, 0.8047378541243649375, 1.000000000000000000 ) ) 
 REPRESENTATION_ITEM ( '' )  );
#12913 = CARTESIAN_POINT ( 'NONE',  ( 73.30402655318508209, 1.750000000000010658, -79.18171244307201562 ) ) ;
#12914 = ORIENTED_EDGE ( 'NONE', *, *, #37121, .F. ) ;
#12915 = EDGE_CURVE ( 'NONE', #31020, #16052, #18084, .T. ) ;
#12916 = DIRECTION ( 'NONE',  ( -1.156482317317871478E-16, 1.000000000000000000, -0.000000000000000000 ) ) ;
#12917 = CARTESIAN_POINT ( 'NONE',  ( 210.0000000000000568, 0.000000000000000000, -157.4317124430720298 ) ) ;
#12918 = VERTEX_POINT ( 'NONE', #14102 ) ;
#12919 = ORIENTED_EDGE ( 'NONE', *, *, #22425, .F. ) ;
#12920 = CARTESIAN_POINT ( 'NONE',  ( -2.538055338523177440, -50.00000000000000711, -9.367992836599954742 ) ) ;
#12921 = CARTESIAN_POINT ( 'NONE',  ( -175.0000000000000000, 15.00000000000000000, -122.5000000000000000 ) ) ;
#12922 = PLANE ( 'NONE',  #16360 ) ;
#12923 = CARTESIAN_POINT ( 'NONE',  ( 210.0000000000000568, 0.000000000000000000, -119.1817124430720440 ) ) ;
#12924 = EDGE_CURVE ( 'NONE', #5904, #20782, #9954, .T. ) ;
#12925 = ORIENTED_EDGE ( 'NONE', *, *, #38753, .F. ) ;
#12926 = EDGE_LOOP ( 'NONE', ( #4407, #6903, #20738, #43199 ) ) ;
#12927 = CARTESIAN_POINT ( 'NONE',  ( -0.4166666666666669072, 0.000000000000000000, -10.00000000000000000 ) ) ;
#12928 = EDGE_CURVE ( 'NONE', #1045, #28535, #36996, .T. ) ;
#12929 = PLANE ( 'NONE',  #33718 ) ;
#12930 = AXIS2_PLACEMENT_3D ( 'NONE', #17267, #21358, #1625 ) ;
#12931 = ORIENTED_EDGE ( 'NONE', *, *, #23360, .T. ) ;
#12932 = ORIENTED_EDGE ( 'NONE', *, *, #11809, .F. ) ;
#12933 = DIRECTION ( 'NONE',  ( 0.000000000000000000, -0.000000000000000000, -1.000000000000000000 ) ) ;
#12934 = CARTESIAN_POINT ( 'NONE',  ( 33.30402655318503946, 1.750000000000010214, 40.81828755692798438 ) ) ;
#12935 = LINE ( 'NONE', #28595, #19355 ) ;
#12936 = CARTESIAN_POINT ( 'NONE',  ( -14.99999999999970868, 17.00000000000000000, -60.00000000000000000 ) ) ;
#12937 = ORIENTED_EDGE ( 'NONE', *, *, #48034, .F. ) ;
#12938 = VERTEX_POINT ( 'NONE', #33379 ) ;
#12939 = ORIENTED_EDGE ( 'NONE', *, *, #37161, .F. ) ;
#12940 = EDGE_CURVE ( 'NONE', #40195, #34478, #20527, .T. ) ;
#12941 = ADVANCED_FACE ( 'NONE', ( #1817 ), #20676, .T. ) ;
#12942 = CARTESIAN_POINT ( 'NONE',  ( 0.000000000000000000, -168.9999999999999432, -344.0000000000001705 ) ) ;
#12943 = ADVANCED_FACE ( 'NONE', ( #2307 ), #10013, .T. ) ;
#12944 = LINE ( 'NONE', #32477, #20528 ) ;
#12945 = ORIENTED_EDGE ( 'NONE', *, *, #39947, .F. ) ;
#12946 = EDGE_LOOP ( 'NONE', ( #17899, #20592, #29465, #14791, #1576, #31421 ) ) ;
#12947 = CARTESIAN_POINT ( 'NONE',  ( -4.641001526964560142, -50.00000000000000711, -8.016098858316199838 ) ) ;
#12948 = ORIENTED_EDGE ( 'NONE', *, *, #37199, .F. ) ;
#12949 = ORIENTED_EDGE ( 'NONE', *, *, #17043, .F. ) ;
#12950 = DIRECTION ( 'NONE',  ( -1.000000000000000000, -0.000000000000000000, -0.000000000000000000 ) ) ;
#12951 = PRESENTATION_STYLE_ASSIGNMENT (( #48067 ) ) ;
#12952 = EDGE_LOOP ( 'NONE', ( #32666, #35296, #31706, #24305 ) ) ;
#12953 = DIRECTION ( 'NONE',  ( -0.000000000000000000, -0.000000000000000000, -1.000000000000000000 ) ) ;
#12954 = LINE ( 'NONE', #36607, #17014 ) ;
#12955 = DIRECTION ( 'NONE',  ( -1.586032892321652236E-16, -1.000000000000000000, -6.853681917100419162E-49 ) ) ;
#12956 = DIRECTION ( 'NONE',  ( -0.000000000000000000, -0.000000000000000000, -1.000000000000000000 ) ) ;
#12957 = ORIENTED_EDGE ( 'NONE', *, *, #20181, .T. ) ;
#12958 = DIRECTION ( 'NONE',  ( 0.000000000000000000, 0.9545212652235329776, -0.2981428420003837121 ) ) ;
#12959 = DIRECTION ( 'NONE',  ( -1.000000000000000000, 0.000000000000000000, 0.000000000000000000 ) ) ;
#12960 = DIRECTION ( 'NONE',  ( 0.000000000000000000, 0.000000000000000000, 1.000000000000000000 ) ) ;
#12961 = EDGE_CURVE ( 'NONE', #5769, #4874, #20922, .T. ) ;
#12962 =( BOUNDED_CURVE ( )  B_SPLINE_CURVE ( 3, ( #22145, #6738, #37814, #37566 ),
 .UNSPECIFIED., .F., .F. ) 
 B_SPLINE_CURVE_WITH_KNOTS ( ( 4, 4 ),
 ( 1.570796326794896558, 3.141592653589793116 ),
 .UNSPECIFIED. ) 
 CURVE ( )  GEOMETRIC_REPRESENTATION_ITEM ( )  RATIONAL_B_SPLINE_CURVE ( ( 1.000000000000000000, 0.8047378541243649375, 0.8047378541243649375, 1.000000000000000000 ) ) 
 REPRESENTATION_ITEM ( '' )  );
#12963 = ADVANCED_FACE ( 'NONE', ( #48710 ), #29513, .T. ) ;
#12964 = AXIS2_PLACEMENT_3D ( 'NONE', #41686, #2683, #21941 ) ;
#12965 = ADVANCED_FACE ( 'NONE', ( #37988 ), #25415, .T. ) ;
#12966 = CARTESIAN_POINT ( 'NONE',  ( 32.27890028733795447, 1.750000000000010436, 119.7931612910808781 ) ) ;
#12967 = ADVANCED_FACE ( 'NONE', ( #37736 ), #29262, .T. ) ;
#12968 = CARTESIAN_POINT ( 'NONE',  ( -126.6959734468149321, 1.749999999999997335, 80.81828755692798438 ) ) ;
#12969 =( BOUNDED_CURVE ( )  B_SPLINE_CURVE ( 3, ( #47717, #44394, #37008, #40076 ),
 .UNSPECIFIED., .F., .F. ) 
 B_SPLINE_CURVE_WITH_KNOTS ( ( 4, 4 ),
 ( 1.570796326794896558, 3.141592653589793116 ),
 .UNSPECIFIED. ) 
 CURVE ( )  GEOMETRIC_REPRESENTATION_ITEM ( )  RATIONAL_B_SPLINE_CURVE ( ( 1.000000000000000000, 0.8047378541243649375, 0.8047378541243649375, 1.000000000000000000 ) ) 
 REPRESENTATION_ITEM ( '' )  );
#12970 = DIRECTION ( 'NONE',  ( -1.000000000000000000, -0.000000000000000000, -0.000000000000000000 ) ) ;
#12971 = AXIS2_PLACEMENT_3D ( 'NONE', #5951, #29310, #49514 ) ;
#12972 = LINE ( 'NONE', #44264, #11565 ) ;
#12973 = ADVANCED_FACE ( 'NONE', ( #37494 ), #14613, .T. ) ;
#12974 = VERTEX_POINT ( 'NONE', #37247 ) ;
#12975 = CARTESIAN_POINT ( 'NONE',  ( -0.9989200098981521059, -1.123829893718962802, 9.927319414211225990 ) ) ;
#12976 = CARTESIAN_POINT ( 'NONE',  ( -88.44597344681494633, 1.025126265847089213, 159.0682875569279418 ) ) ;
#12977 = VERTEX_POINT ( 'NONE', #2067 ) ;
#12978 = CARTESIAN_POINT ( 'NONE',  ( -126.6959734468149321, 1.749999999999996891, 0.8182875569279768335 ) ) ;
#12979 = FACE_OUTER_BOUND ( 'NONE', #30678, .T. ) ;
#12980 = CARTESIAN_POINT ( 'NONE',  ( -85.67084718096784002, -1.750000000000009548, 81.84341382277507648 ) ) ;
#12981 = ORIENTED_EDGE ( 'NONE', *, *, #29289, .F. ) ;
#12982 = CARTESIAN_POINT ( 'NONE',  ( 14.49999999999999822, 12.98684210526315930, -19.37312575500900280 ) ) ;
#12983 = B_SPLINE_SURFACE_WITH_KNOTS ( 'NONE', 3, 3, ( 
 ( #32584, #12815, #20757, #21267 ),
 ( #36439, #5868, #41263, #8968 ),
 ( #40523, #48168, #9212, #13558 ),
 ( #36955, #1774, #17419, #33087 ) ),
 .UNSPECIFIED., .F., .F., .F.,
 ( 4, 4 ),
 ( 4, 4 ),
 ( 0.000000000000000000, 1.000000000000000000 ),
 ( 0.000000000000000000, 1.000000000000000000 ),
 .UNSPECIFIED. ) ;
#12984 = VERTEX_POINT ( 'NONE', #17715 ) ;
#12985 = CARTESIAN_POINT ( 'NONE',  ( -16.52264463346130796, 2.779753662172870232, 9.403735324607438884 ) ) ;
#12986 = CARTESIAN_POINT ( 'NONE',  ( 181.0000000000000000, 175.0000000000000284, -342.0000000000001137 ) ) ;
#12987 = ORIENTED_EDGE ( 'NONE', *, *, #50285, .F. ) ;
#12988 = DIRECTION ( 'NONE',  ( -0.000000000000000000, -0.000000000000000000, -1.000000000000000000 ) ) ;
#12989 = CARTESIAN_POINT ( 'NONE',  ( -168.4459734468149463, 0.000000000000000000, -0.9317124430720247208 ) ) ;
#12990 = ORIENTED_EDGE ( 'NONE', *, *, #25437, .T. ) ;
#12991 = ORIENTED_EDGE ( 'NONE', *, *, #26219, .F. ) ;
#12992 = DIRECTION ( 'NONE',  ( -1.000000000000000000, 0.000000000000000000, 1.860490536778032451E-50 ) ) ;
#12993 = EDGE_CURVE ( 'NONE', #12217, #43021, #50213, .T. ) ;
#12994 = ADVANCED_FACE ( 'NONE', ( #11540 ), #39248, .T. ) ;
#12995 = ORIENTED_EDGE ( 'NONE', *, *, #20801, .F. ) ;
#12996 = DIRECTION ( 'NONE',  ( -1.000000000000000000, 0.000000000000000000, 0.000000000000000000 ) ) ;
#12997 = CARTESIAN_POINT ( 'NONE',  ( 10.49999999999996447, 8.875661936878630698, 18.94832733001756253 ) ) ;
#12998 = VECTOR ( 'NONE', #26602, 1000.000000000000000 ) ;
#12999 = CARTESIAN_POINT ( 'NONE',  ( 1.011271242968688311, -0.7347315653655855927, 3.333333333333333481 ) ) ;
#13000 = ADVANCED_FACE ( 'NONE', ( #46395 ), #43077, .T. ) ;
#13001 = VERTEX_POINT ( 'NONE', #11283 ) ;
#13002 = ADVANCED_FACE ( 'NONE', ( #23327, #7948 ), #38998, .T. ) ;
#13003 = VECTOR ( 'NONE', #35671, 1000.000000000000000 ) ;
#13004 = CYLINDRICAL_SURFACE ( 'NONE', #29247, 0.5000000000000004441 ) ;
#13005 = CARTESIAN_POINT ( 'NONE',  ( -204.9459734468149463, 2.143131898507880377E-16, 165.0000000000000000 ) ) ;
#13006 = ORIENTED_EDGE ( 'NONE', *, *, #35978, .T. ) ;
#13007 = ORIENTED_EDGE ( 'NONE', *, *, #35263, .F. ) ;
#13008 = VERTEX_POINT ( 'NONE', #46125 ) ;
#13009 = CARTESIAN_POINT ( 'NONE',  ( 7.499999999999944045, -224.9999999999999716, -240.0000000000000000 ) ) ;
#13010 = AXIS2_PLACEMENT_3D ( 'NONE', #41538, #22537, #49937 ) ;
#13011 = ADVANCED_FACE ( 'NONE', ( #26922 ), #22564, .T. ) ;
#13012 = EDGE_CURVE ( 'NONE', #31089, #3248, #15124, .T. ) ;
#13013 = CYLINDRICAL_SURFACE ( 'NONE', #7854, 4.000000000000003553 ) ;
#13014 = EDGE_LOOP ( 'NONE', ( #7157, #19689, #27022, #7440 ) ) ;
#13015 = DIRECTION ( 'NONE',  ( -1.000000000000000000, -0.000000000000000000, -0.000000000000000000 ) ) ;
#13016 = CARTESIAN_POINT ( 'NONE',  ( 7.499999999999948486, -194.9999999999999716, -240.0000000000000000 ) ) ;
#13017 = FACE_OUTER_BOUND ( 'NONE', #24126, .T. ) ;
#13018 = VECTOR ( 'NONE', #26188, 1000.000000000000000 ) ;
#13019 = CARTESIAN_POINT ( 'NONE',  ( 111.5540265531850537, 1.025126265847081664, -37.43171244307203693 ) ) ;
#13020 = LINE ( 'NONE', #1988, #6663 ) ;
#13021 = LINE ( 'NONE', #21732, #33942 ) ;
#13022 = CARTESIAN_POINT ( 'NONE',  ( -46.69597344681494633, -1.750000000000009992, 0.8182875569279768335 ) ) ;
#13023 = DIRECTION ( 'NONE',  ( -1.000000000000000000, -0.000000000000000000, -0.000000000000000000 ) ) ;
#13024 = DIRECTION ( 'NONE',  ( -1.000000000000000000, -0.000000000000000000, -0.000000000000000000 ) ) ;
#13025 = CARTESIAN_POINT ( 'NONE',  ( -3.975459390375366997, -0.2195152216756601216, -2.642742795433417058E-16 ) ) ;
#13026 = EDGE_CURVE ( 'NONE', #11765, #28419, #4089, .T. ) ;
#13027 = CARTESIAN_POINT ( 'NONE',  ( 0.000000000000000000, 0.000000000000000000, 0.000000000000000000 ) ) ;
#13028 = EDGE_CURVE ( 'NONE', #3789, #45615, #11021, .T. ) ;
#13029 = EDGE_CURVE ( 'NONE', #27105, #39341, #15512, .T. ) ;
#13030 = DIRECTION ( 'NONE',  ( -1.000000000000000000, 0.000000000000000000, 0.000000000000000000 ) ) ;
#13031 = ORIENTED_EDGE ( 'NONE', *, *, #40882, .T. ) ;
#13032 = DIRECTION ( 'NONE',  ( -1.000000000000000000, -0.000000000000000000, -0.000000000000000000 ) ) ;
#13033 = DIRECTION ( 'NONE',  ( 0.000000000000000000, -0.000000000000000000, -1.000000000000000000 ) ) ;
#13034 = CARTESIAN_POINT ( 'NONE',  ( 154.1026953830863420, -97.66198943095992036, -17.65743994998277699 ) ) ;
#13035 = PRODUCT_DEFINITION ( 'UNKNOWN', '', #37356, #39611 ) ;
#13036 = CYLINDRICAL_SURFACE ( 'NONE', #30389, 1.750000000000001554 ) ;
#13037 = AXIS2_PLACEMENT_3D ( 'NONE', #10519, #21562, #41574 ) ;
#13038 = EDGE_LOOP ( 'NONE', ( #40981, #22516, #12890, #13198 ) ) ;
#13039 = CARTESIAN_POINT ( 'NONE',  ( -124.9459734468149463, 2.143131898507847836E-16, -80.93171244307201562 ) ) ;
#13040 = AXIS2_PLACEMENT_3D ( 'NONE', #24737, #4724, #43961 ) ;
#13041 = CARTESIAN_POINT ( 'NONE',  ( 350.0000000000001137, 169.0000000000000000, 357.9999999999997726 ) ) ;
#13042 = EDGE_LOOP ( 'NONE', ( #2643, #17963, #15624, #41173, #24862, #41071 ) ) ;
#13043 = VECTOR ( 'NONE', #34872, 1000.000000000000000 ) ;
#13044 = LINE ( 'NONE', #1516, #22999 ) ;
#13046 = EDGE_CURVE ( 'NONE', #38061, #47848, #33373, .T. ) ;
#13045 = CARTESIAN_POINT ( 'NONE',  ( 177.5000000000000284, -112.5000000000000000, 0.000000000000000000 ) ) ;
#13047 = VECTOR ( 'NONE', #29700, 1000.000000000000000 ) ;
#13048 = FACE_OUTER_BOUND ( 'NONE', #9403, .T. ) ;
#13049 = B_SPLINE_CURVE_WITH_KNOTS ( 'NONE', 3,
 ( #9398, #16852, #1953, #5799 ),
 .UNSPECIFIED., .F., .F.,
 ( 4, 4 ),
 ( 0.000000000000000000, 0.002466147708923230580 ),
 .UNSPECIFIED. ) ;
#13050 = ORIENTED_EDGE ( 'NONE', *, *, #17834, .T. ) ;
#13051 = DIRECTION ( 'NONE',  ( 0.000000000000000000, -2.265761274745217480E-16, 1.000000000000000000 ) ) ;
#13052 = VERTEX_POINT ( 'NONE', #35156 ) ;
#13053 = ORIENTED_EDGE ( 'NONE', *, *, #11772, .T. ) ;
#13054 = AXIS2_PLACEMENT_3D ( 'NONE', #17544, #32451, #4732 ) ;
#13055 = ORIENTED_EDGE ( 'NONE', *, *, #13944, .T. ) ;
#13056 = LINE ( 'NONE', #44839, #8189 ) ;
#13057 = EDGE_CURVE ( 'NONE', #48360, #10360, #27041, .T. ) ;
#13058 = ORIENTED_EDGE ( 'NONE', *, *, #43776, .F. ) ;
#13059 = DIRECTION ( 'NONE',  ( 0.000000000000000000, 0.000000000000000000, -1.000000000000000000 ) ) ;
#13060 = DIRECTION ( 'NONE',  ( 0.000000000000000000, 0.000000000000000000, 1.000000000000000000 ) ) ;
#13061 = CARTESIAN_POINT ( 'NONE',  ( 210.0000000000000568, 0.000000000000000000, -39.18171244307202983 ) ) ;
#13062 = FACE_OUTER_BOUND ( 'NONE', #49543, .T. ) ;
#13063 = ORIENTED_EDGE ( 'NONE', *, *, #48490, .F. ) ;
#13064 = LINE ( 'NONE', #20766, #31345 ) ;
#13065 = ADVANCED_FACE ( 'NONE', ( #12046 ), #38249, .F. ) ;
#13066 = ORIENTED_EDGE ( 'NONE', *, *, #27810, .F. ) ;
#13067 = ADVANCED_FACE ( 'NONE', ( #34385 ), #26678, .T. ) ;
#13068 = DIRECTION ( 'NONE',  ( 0.000000000000000000, 0.000000000000000000, 1.000000000000000000 ) ) ;
#13069 = CARTESIAN_POINT ( 'NONE',  ( 356.0000000000000000, -167.0000000000001137, -342.0000000000002842 ) ) ;
#13070 = VERTEX_POINT ( 'NONE', #42320 ) ;
#13071 = ORIENTED_EDGE ( 'NONE', *, *, #7454, .F. ) ;
#13072 = VERTEX_POINT ( 'NONE', #7178 ) ;
#13073 = CARTESIAN_POINT ( 'NONE',  ( -4.945973446814903696, 2.143131898507912917E-16, 79.06828755692795596 ) ) ;
#13074 = EDGE_CURVE ( 'NONE', #7169, #12438, #8161, .T. ) ;
#13075 = CARTESIAN_POINT ( 'NONE',  ( 0.000000000000000000, 167.0000000000000000, 355.9999999999997726 ) ) ;
#13076 = ORIENTED_EDGE ( 'NONE', *, *, #39357, .F. ) ;
#13077 = AXIS2_PLACEMENT_3D ( 'NONE', #29724, #7139, #41524 ) ;
#13078 = EDGE_CURVE ( 'NONE', #24013, #18422, #22060, .T. ) ;
#13079 = AXIS2_PLACEMENT_3D ( 'NONE', #25938, #26422, #26179 ) ;
#13080 = DIRECTION ( 'NONE',  ( -1.000000000000000000, 0.000000000000000000, 0.000000000000000000 ) ) ;
#13081 = DIRECTION ( 'NONE',  ( 1.000000000000000000, -0.000000000000000000, 0.000000000000000000 ) ) ;
#13082 = EDGE_CURVE ( 'NONE', #30057, #46103, #40008, .T. ) ;
#13083 = CARTESIAN_POINT ( 'NONE',  ( -206.6959734468149463, -1.750000000000009992, -159.1817124430720298 ) ) ;
#13084 = VECTOR ( 'NONE', #12916, 1000.000000000000000 ) ;
#13085 = VERTEX_POINT ( 'NONE', #32307 ) ;
#13086 = CARTESIAN_POINT ( 'NONE',  ( -6.695973446814940111, 1.750000000000023759, -39.18171244307202983 ) ) ;
#13087 = DIRECTION ( 'NONE',  ( -1.000000000000000000, 0.000000000000000000, 0.000000000000000000 ) ) ;
#13088 = VECTOR ( 'NONE', #9782, 1000.000000000000114 ) ;
#13089 = EDGE_CURVE ( 'NONE', #8176, #31607, #5341, .T. ) ;
#13090 = ORIENTED_EDGE ( 'NONE', *, *, #7987, .F. ) ;
#13091 = ORIENTED_EDGE ( 'NONE', *, *, #35251, .T. ) ;
#13092 = ITEM_DEFINED_TRANSFORMATION ( 'NONE', 'NONE', #47092,  #30773 ) ;
#13094 = CARTESIAN_POINT ( 'NONE',  ( -8.445973446814964092, 1.025126265847096985, -37.43171244307200851 ) ) ;
#13093 = VECTOR ( 'NONE', #5423, 1000.000000000000000 ) ;
#13095 = DIRECTION ( 'NONE',  ( -1.000000000000000000, 0.000000000000000000, -2.958228394578794270E-31 ) ) ;
#13096 = LINE ( 'NONE', #7294, #18295 ) ;
#13097 = CARTESIAN_POINT ( 'NONE',  ( -31.28977333267361871, 11.25592690310926969, -2.408242355805840784 ) ) ;
#13098 = EDGE_LOOP ( 'NONE', ( #7952, #25814, #50368, #9303, #6205, #21528, #12745, #39807 ) ) ;
#13099 = CARTESIAN_POINT ( 'NONE',  ( -0.3862712429686729343, -1.188820645368946050, 10.00000000000000000 ) ) ;
#13100 = PLANE ( 'NONE',  #31081 ) ;
#13101 = CARTESIAN_POINT ( 'NONE',  ( -0.6909887759940060992, 1.008432015058918552, 9.987567862361069970 ) ) ;
#13102 = CARTESIAN_POINT ( 'NONE',  ( -9.999999999999994671, -46.01315789473684248, 5.916985404131813731 ) ) ;
#13103 = EDGE_LOOP ( 'NONE', ( #16694, #30931, #15536, #6396, #48931, #7033 ) ) ;
#13104 = CARTESIAN_POINT ( 'NONE',  ( 71.55402655318505367, 0.000000000000000000, 39.06828755692795596 ) ) ;
#13105 = VERTEX_POINT ( 'NONE', #44319 ) ;
#13106 = CARTESIAN_POINT ( 'NONE',  ( -206.6959734468149463, -1.750000000000010214, -39.18171244307202983 ) ) ;
#13107 = EDGE_LOOP ( 'NONE', ( #19490, #3596, #652, #29520, #45733, #20899 ) ) ;
#13108 = CARTESIAN_POINT ( 'NONE',  ( -204.9459734468148895, 1.025126265847089213, 159.0682875569279418 ) ) ;
#13109 = CARTESIAN_POINT ( 'NONE',  ( -208.4459734468148611, -1.025126265847089213, -160.9317124430720014 ) ) ;
#13110 = CARTESIAN_POINT ( 'NONE',  ( -85.67084718096784002, 1.750000000000009548, 39.79316129108089228 ) ) ;
#13111 = AXIS2_PLACEMENT_3D ( 'NONE', #33025, #12988, #17105 ) ;
#13112 = ORIENTED_EDGE ( 'NONE', *, *, #48424, .T. ) ;
#13113 = EDGE_CURVE ( 'NONE', #45829, #39370, #20487, .T. ) ;
#13114 = VECTOR ( 'NONE', #50300, 1000.000000000000000 ) ;
#13115 =( BOUNDED_CURVE ( )  B_SPLINE_CURVE ( 3, ( #36891, #17103, #5299, #25066 ),
 .UNSPECIFIED., .F., .F. ) 
 B_SPLINE_CURVE_WITH_KNOTS ( ( 4, 4 ),
 ( 0.000000000000000000, 1.570796326794896558 ),
 .UNSPECIFIED. ) 
 CURVE ( )  GEOMETRIC_REPRESENTATION_ITEM ( )  RATIONAL_B_SPLINE_CURVE ( ( 1.000000000000000000, 0.8047378541243649375, 0.8047378541243649375, 1.000000000000000000 ) ) 
 REPRESENTATION_ITEM ( '' )  );
#13116 = LINE ( 'NONE', #28777, #13018 ) ;
#13117 = ORIENTED_EDGE ( 'NONE', *, *, #26154, .F. ) ;
#13118 = DIRECTION ( 'NONE',  ( 1.860490536778032451E-50, 0.000000000000000000, -1.000000000000000000 ) ) ;
#13119 = PLANE ( 'NONE',  #13393 ) ;
#13120 = CARTESIAN_POINT ( 'NONE',  ( 1.222012661920449439, -0.2471648704738783342, 9.981352469109934233 ) ) ;
#13121 = DIRECTION ( 'NONE',  ( 0.9770330068457271366, -0.000000000000000000, 0.2130880182788259247 ) ) ;
#13122 = AXIS2_PLACEMENT_3D ( 'NONE', #6073, #29677, #37652 ) ;
#13123 =( BOUNDED_CURVE ( )  B_SPLINE_CURVE ( 3, ( #20868, #8325, #27819, #36548 ),
 .UNSPECIFIED., .F., .F. ) 
 B_SPLINE_CURVE_WITH_KNOTS ( ( 4, 4 ),
 ( 1.570796326794896558, 3.141592653589793116 ),
 .UNSPECIFIED. ) 
 CURVE ( )  GEOMETRIC_REPRESENTATION_ITEM ( )  RATIONAL_B_SPLINE_CURVE ( ( 1.000000000000000000, 0.8047378541243649375, 0.8047378541243649375, 1.000000000000000000 ) ) 
 REPRESENTATION_ITEM ( '' )  );
#13124 = DIRECTION ( 'NONE',  ( -1.000000000000000000, 0.000000000000000000, 0.000000000000000000 ) ) ;
#13125 = AXIS2_PLACEMENT_3D ( 'NONE', #725, #32039, #16371 ) ;
#13126 = VERTEX_POINT ( 'NONE', #506 ) ;
#13127 = ORIENTED_EDGE ( 'NONE', *, *, #24035, .T. ) ;
#13128 = FACE_BOUND ( 'NONE', #32439, .T. ) ;
#13129 = AXIS2_PLACEMENT_3D ( 'NONE', #43347, #28723, #4368 ) ;
#13130 = EDGE_CURVE ( 'NONE', #24963, #41575, #38499, .T. ) ;
#13131 = EDGE_LOOP ( 'NONE', ( #18873, #20759 ) ) ;
#13132 = EDGE_CURVE ( 'NONE', #49775, #4462, #12532, .T. ) ;
#13133 = DIRECTION ( 'NONE',  ( 0.000000000000000000, -2.265761274745217480E-16, 1.000000000000000000 ) ) ;
#13134 = CARTESIAN_POINT ( 'NONE',  ( 164.9999999999999716, -184.9999999999999716, -344.0000000000001137 ) ) ;
#13135 = DIRECTION ( 'NONE',  ( -0.000000000000000000, -0.000000000000000000, 1.000000000000000000 ) ) ;
#13136 = ORIENTED_EDGE ( 'NONE', *, *, #30906, .T. ) ;
#13137 = DIRECTION ( 'NONE',  ( -0.000000000000000000, -0.000000000000000000, -1.000000000000000000 ) ) ;
#13138 =( BOUNDED_CURVE ( )  B_SPLINE_CURVE ( 3, ( #38930, #3756, #23773, #28124 ),
 .UNSPECIFIED., .F., .F. ) 
 B_SPLINE_CURVE_WITH_KNOTS ( ( 4, 4 ),
 ( 1.570796326794896558, 3.141592653589793116 ),
 .UNSPECIFIED. ) 
 CURVE ( )  GEOMETRIC_REPRESENTATION_ITEM ( )  RATIONAL_B_SPLINE_CURVE ( ( 1.000000000000000000, 0.8047378541243649375, 0.8047378541243649375, 1.000000000000000000 ) ) 
 REPRESENTATION_ITEM ( '' )  );
#13139 = FACE_OUTER_BOUND ( 'NONE', #1418, .T. ) ;
#13140 = CARTESIAN_POINT ( 'NONE',  ( 356.0000000000000000, -167.0000000000001137, -342.0000000000002842 ) ) ;
#13141 = FACE_OUTER_BOUND ( 'NONE', #37540, .T. ) ;
#13142 = EDGE_CURVE ( 'NONE', #46411, #41927, #36893, .T. ) ;
#13143 = CARTESIAN_POINT ( 'NONE',  ( 33.30402655318503946, -1.750000000000009992, 160.8182875569279702 ) ) ;
#13144 = EDGE_CURVE ( 'NONE', #31478, #16715, #48247, .T. ) ;
#13145 = CARTESIAN_POINT ( 'NONE',  ( 15.00000000000000000, 13.48684210526315930, -20.00000000000000000 ) ) ;
#13146 = VERTEX_POINT ( 'NONE', #9189 ) ;
#13147 = VERTEX_POINT ( 'NONE', #27944 ) ;
#13148 = VERTEX_POINT ( 'NONE', #24850 ) ;
#13149 = CARTESIAN_POINT ( 'NONE',  ( -168.4459734468149463, 0.000000000000000000, -117.4317124430720725 ) ) ;
#13150 = EDGE_CURVE ( 'NONE', #20047, #21591, #40504, .T. ) ;
#13151 = CARTESIAN_POINT ( 'NONE',  ( -50.00000000000000000, -50.00000000000000000, 800.0000000000000000 ) ) ;
#13152 = DIRECTION ( 'NONE',  ( 0.000000000000000000, 0.000000000000000000, -1.000000000000000000 ) ) ;
#13153 = CARTESIAN_POINT ( 'NONE',  ( 72.27890028733797578, -1.750000000000009548, 1.843413822775065825 ) ) ;
#13154 = VERTEX_POINT ( 'NONE', #12285 ) ;
#13155 = LINE ( 'NONE', #28308, #26670 ) ;
#13157 = ORIENTED_EDGE ( 'NONE', *, *, #36523, .F. ) ;
#13156 = AXIS2_PLACEMENT_3D ( 'NONE', #4302, #3264, #35620 ) ;
#13158 =( NAMED_UNIT ( * ) PLANE_ANGLE_UNIT ( ) SI_UNIT ( $, .RADIAN. ) );
#13159 = PLANE ( 'NONE',  #19565 ) ;
#13160 = DIRECTION ( 'NONE',  ( 0.000000000000000000, 0.000000000000000000, 1.000000000000000000 ) ) ;
#13161 = DIRECTION ( 'NONE',  ( 0.000000000000000000, 0.000000000000000000, 1.000000000000000000 ) ) ;
#13162 = AXIS2_PLACEMENT_3D ( 'NONE', #49537, #6993, #10837 ) ;
#13163 = LINE ( 'NONE', #20611, #34029 ) ;
#13164 = CYLINDRICAL_SURFACE ( 'NONE', #26609, 1.750000000000015543 ) ;
#13165 = LINE ( 'NONE', #37051, #43652 ) ;
#13166 = ORIENTED_EDGE ( 'NONE', *, *, #23723, .F. ) ;
#13167 = CARTESIAN_POINT ( 'NONE',  ( -205.6708471809678827, -1.750000000000009548, 159.7931612910809065 ) ) ;
#13168 = VECTOR ( 'NONE', #26215, 1000.000000000000000 ) ;
#13170 = VECTOR ( 'NONE', #45389, 1000.000000000000000 ) ;
#13169 = DIRECTION ( 'NONE',  ( 0.5038710255240862468, 0.000000000000000000, 0.8637789008984334549 ) ) ;
#13171 = CARTESIAN_POINT ( 'NONE',  ( 181.0000000000000284, -174.9999999999999716, -111.0000000000001563 ) ) ;
#13172 =( LENGTH_UNIT ( ) NAMED_UNIT ( * ) SI_UNIT ( .MILLI., .METRE. ) );
#13173 = ORIENTED_EDGE ( 'NONE', *, *, #38682, .F. ) ;
#13174 = DIRECTION ( 'NONE',  ( -1.000000000000000000, 0.000000000000000000, -0.000000000000000000 ) ) ;
#13175 = EDGE_LOOP ( 'NONE', ( #39247, #46129, #48068, #12987 ) ) ;
#13177 = EDGE_CURVE ( 'NONE', #15989, #36849, #47387, .T. ) ;
#13176 = DIRECTION ( 'NONE',  ( -0.000000000000000000, -0.000000000000000000, -1.000000000000000000 ) ) ;
#13178 = CARTESIAN_POINT ( 'NONE',  ( 0.000000000000000000, -49.99999999999994316, 800.0000000000001137 ) ) ;
#13179 = CARTESIAN_POINT ( 'NONE',  ( -3.808200756227646089, -0.8261963378076270237, 9.741991644047246268 ) ) ;
#13180 = EDGE_CURVE ( 'NONE', #28520, #44581, #20998, .T. ) ;
#13181 = ORIENTED_EDGE ( 'NONE', *, *, #35712, .F. ) ;
#13182 = CARTESIAN_POINT ( 'NONE',  ( 14.91630425054810161, -7.943683830272123991, -9.008049429158102583 ) ) ;
#13183 = CARTESIAN_POINT ( 'NONE',  ( -0.7606162131530730397, 1.296876929034918691, 9.953784399990622589 ) ) ;
#13184 = CARTESIAN_POINT ( 'NONE',  ( 153.3040265531850537, 0.000000000000000000, -165.0000000000000000 ) ) ;
#13185 = CARTESIAN_POINT ( 'NONE',  ( 210.0000000000000568, 0.000000000000000000, -119.1817124430720440 ) ) ;
#13186 = EDGE_LOOP ( 'NONE', ( #45701, #22460, #23186, #5083 ) ) ;
#13187 = ORIENTED_EDGE ( 'NONE', *, *, #33064, .F. ) ;
#13188 = B_SPLINE_CURVE_WITH_KNOTS ( 'NONE', 3,
 ( #494, #27936, #47380, #43573 ),
 .UNSPECIFIED., .F., .F.,
 ( 4, 4 ),
 ( 0.9688112071879397824, 0.9724175925769220630 ),
 .UNSPECIFIED. ) ;
#13189 = DIRECTION ( 'NONE',  ( 0.000000000000000000, 0.000000000000000000, 1.000000000000000000 ) ) ;
#13190 = CYLINDRICAL_SURFACE ( 'NONE', #21389, 1.750000000000015543 ) ;
#13191 = AXIS2_PLACEMENT_3D ( 'NONE', #7279, #27294, #50587 ) ;
#13192 = VERTEX_POINT ( 'NONE', #43829 ) ;
#13193 = VERTEX_POINT ( 'NONE', #24599 ) ;
#13194 = CARTESIAN_POINT ( 'NONE',  ( 44.99506233596247995, 23.32283626942318833, 7.455576670931136185 ) ) ;
#13195 = CARTESIAN_POINT ( 'NONE',  ( 210.0000000000000568, 0.000000000000000000, -159.1817124430720298 ) ) ;
#13196 = CARTESIAN_POINT ( 'NONE',  ( -0.3862712429686977478, 1.188820645368937390, 10.00000000000000000 ) ) ;
#13197 = LINE ( 'NONE', #9355, #37086 ) ;
#13198 = ORIENTED_EDGE ( 'NONE', *, *, #49346, .T. ) ;
#13199 = ORIENTED_EDGE ( 'NONE', *, *, #1487, .T. ) ;
#13200 = EDGE_LOOP ( 'NONE', ( #4740, #19371, #15664, #39710 ) ) ;
#13201 = LINE ( 'NONE', #28858, #31657 ) ;
#13202 = PLANE ( 'NONE',  #48655 ) ;
#13203 = CARTESIAN_POINT ( 'NONE',  ( -21.58778298521296080, 25.34222074689773407, 3.199614146704519602 ) ) ;
#13204 = ORIENTED_EDGE ( 'NONE', *, *, #24409, .T. ) ;
#13205 = ORIENTED_EDGE ( 'NONE', *, *, #32827, .T. ) ;
#13206 = ADVANCED_FACE ( 'NONE', ( #1000 ), #40249, .T. ) ;
#13207 = CARTESIAN_POINT ( 'NONE',  ( -69.99999999999816680, 17.00000000000000000, 90.00000000000000000 ) ) ;
#13208 = CARTESIAN_POINT ( 'NONE',  ( 181.0000000000000000, -256.4999999999999432, -349.9999999999999432 ) ) ;
#13209 = ORIENTED_EDGE ( 'NONE', *, *, #38112, .F. ) ;
#13210 = VERTEX_POINT ( 'NONE', #744 ) ;
#13211 = CARTESIAN_POINT ( 'NONE',  ( 49.89397392339123627, -8.245536726716670373, 7.906207997025717304 ) ) ;
#13212 = CARTESIAN_POINT ( 'NONE',  ( -128.4459734468149463, 1.025126265847081664, 82.56828755692798438 ) ) ;
#13213 = ORIENTED_EDGE ( 'NONE', *, *, #14692, .F. ) ;
#13214 = LINE ( 'NONE', #21413, #6989 ) ;
#13215 = CARTESIAN_POINT ( 'NONE',  ( -86.69597344681496054, 0.000000000000000000, 165.0000000000000000 ) ) ;
#13216 = CARTESIAN_POINT ( 'NONE',  ( -2.051144455471382688, -1.664205274803698620, 9.847478953136990398 ) ) ;
#13217 = LINE ( 'NONE', #21170, #12208 ) ;
#13218 =( BOUNDED_CURVE ( )  B_SPLINE_CURVE ( 3, ( #37925, #3492, #34313, #26610 ),
 .UNSPECIFIED., .F., .F. ) 
 B_SPLINE_CURVE_WITH_KNOTS ( ( 4, 4 ),
 ( 0.000000000000000000, 1.570796326794896558 ),
 .UNSPECIFIED. ) 
 CURVE ( )  GEOMETRIC_REPRESENTATION_ITEM ( )  RATIONAL_B_SPLINE_CURVE ( ( 1.000000000000000000, 0.8047378541243649375, 0.8047378541243649375, 1.000000000000000000 ) ) 
 REPRESENTATION_ITEM ( '' )  );
#13219 = CARTESIAN_POINT ( 'NONE',  ( 153.3040265531850537, -1.750000000000009992, 0.8182875569279768335 ) ) ;
#13220 = ORIENTED_EDGE ( 'NONE', *, *, #18938, .F. ) ;
#13221 = CARTESIAN_POINT ( 'NONE',  ( 168.9999999999999716, -164.9999999999999432, -115.0000000000001847 ) ) ;
#13222 = VECTOR ( 'NONE', #10612, 1000.000000000000000 ) ;
#13223 = DIRECTION ( 'NONE',  ( 1.000000000000000000, 0.000000000000000000, 0.000000000000000000 ) ) ;
#13224 = CARTESIAN_POINT ( 'NONE',  ( -5.083187235775261215, -8.611690166631138510, 9.646707543097347681 ) ) ;
#13225 = CARTESIAN_POINT ( 'NONE',  ( 344.0000000000000568, 169.0000000000000000, 349.9999999999998295 ) ) ;
#13226 = AXIS2_PLACEMENT_3D ( 'NONE', #8181, #23573, #16374 ) ;
#13227 = CARTESIAN_POINT ( 'NONE',  ( 214.9999999999999432, -175.0000000000000000, 497.2965085865001811 ) ) ;
#13228 = SPHERICAL_SURFACE ( 'NONE', #21290, 0.5000000000000000000 ) ;
#13229 = AXIS2_PLACEMENT_3D ( 'NONE', #39578, #2254, #16476 ) ;
#13230 = CARTESIAN_POINT ( 'NONE',  ( 16.73672383626881199, 2.341008440548111302, -9.008049429158100807 ) ) ;
#13231 = VERTEX_POINT ( 'NONE', #20740 ) ;
#13232 = CARTESIAN_POINT ( 'NONE',  ( -12.78770032058971395, -31.68259716188267916, 7.455576670931136185 ) ) ;
#13233 = FACE_OUTER_BOUND ( 'NONE', #20690, .T. ) ;
#13234 = CARTESIAN_POINT ( 'NONE',  ( -168.4459734468149463, 0.000000000000000000, -165.0000000000000000 ) ) ;
#13235 = CARTESIAN_POINT ( 'NONE',  ( 11.73320209285708415, -11.96063479729170886, 9.403735324607438884 ) ) ;
#13236 = DIRECTION ( 'NONE',  ( -0.000000000000000000, -0.000000000000000000, 1.000000000000000000 ) ) ;
#13237 = VERTEX_POINT ( 'NONE', #27690 ) ;
#13238 = DIRECTION ( 'NONE',  ( 1.860490536778032451E-50, 0.000000000000000000, 1.000000000000000000 ) ) ;
#13239 = ORIENTED_EDGE ( 'NONE', *, *, #18370, .T. ) ;
#13240 = DIRECTION ( 'NONE',  ( -1.000000000000000000, -0.000000000000000000, -0.000000000000000000 ) ) ;
#13241 = DIRECTION ( 'NONE',  ( 0.000000000000000000, 0.000000000000000000, 1.000000000000000000 ) ) ;
#13242 = ORIENTED_EDGE ( 'NONE', *, *, #37547, .T. ) ;
#13243 = FACE_OUTER_BOUND ( 'NONE', #26757, .T. ) ;
#13244 = CARTESIAN_POINT ( 'NONE',  ( 35.05402655318504657, 2.143131898507880377E-16, 2.568287556927978166 ) ) ;
#13245 = EDGE_LOOP ( 'NONE', ( #44673, #34491, #1629, #27606, #20204, #20705 ) ) ;
#13246 = ORIENTED_EDGE ( 'NONE', *, *, #49692, .T. ) ;
#13247 = VECTOR ( 'NONE', #37781, 1000.000000000000000 ) ;
#13248 = LINE ( 'NONE', #40215, #35666 ) ;
#13249 = CARTESIAN_POINT ( 'NONE',  ( -225.0000000000000568, -165.6999999999999602, 254.8599999999999852 ) ) ;
#13250 = DIRECTION ( 'NONE',  ( -0.000000000000000000, -0.000000000000000000, -1.000000000000000000 ) ) ;
#13251 = ORIENTED_EDGE ( 'NONE', *, *, #15140, .T. ) ;
#13252 = ADVANCED_FACE ( 'NONE', ( #8709 ), #16639, .F. ) ;
#13253 = CARTESIAN_POINT ( 'NONE',  ( 113.3040265531850537, -1.749999999999997335, 80.81828755692798438 ) ) ;
#13254 = VECTOR ( 'NONE', #3634, 1000.000000000000000 ) ;
#13255 = FACE_OUTER_BOUND ( 'NONE', #3109, .T. ) ;
#13256 = ORIENTED_EDGE ( 'NONE', *, *, #17337, .T. ) ;
#13257 = ORIENTED_EDGE ( 'NONE', *, *, #11835, .F. ) ;
#13258 = ORIENTED_EDGE ( 'NONE', *, *, #7072, .F. ) ;
#13259 = DIRECTION ( 'NONE',  ( -0.000000000000000000, -1.000000000000000000, -0.000000000000000000 ) ) ;
#13260 = EDGE_CURVE ( 'NONE', #47621, #39178, #8199, .T. ) ;
#13261 = CARTESIAN_POINT ( 'NONE',  ( -64.99999999999783995, 17.00000000000000000, 95.00000000000000000 ) ) ;
#13262 = ORIENTED_EDGE ( 'NONE', *, *, #34934, .T. ) ;
#13263 = EDGE_CURVE ( 'NONE', #35061, #3446, #31807, .T. ) ;
#13264 = LINE ( 'NONE', #16622, #6117 ) ;
#13265 = DIRECTION ( 'NONE',  ( 1.000000000000000000, 0.000000000000000000, 0.000000000000000000 ) ) ;
#13266 = EDGE_CURVE ( 'NONE', #14822, #29017, #39756, .T. ) ;
#13267 =( BOUNDED_CURVE ( )  B_SPLINE_CURVE ( 3, ( #17674, #25633, #21271, #45096 ),
 .UNSPECIFIED., .F., .F. ) 
 B_SPLINE_CURVE_WITH_KNOTS ( ( 4, 4 ),
 ( 3.141592653589793116, 4.712388980384689674 ),
 .UNSPECIFIED. ) 
 CURVE ( )  GEOMETRIC_REPRESENTATION_ITEM ( )  RATIONAL_B_SPLINE_CURVE ( ( 1.000000000000000000, 0.8047378541243649375, 0.8047378541243649375, 1.000000000000000000 ) ) 
 REPRESENTATION_ITEM ( '' )  );
#13268 = CARTESIAN_POINT ( 'NONE',  ( -44.94597344681493922, 2.143131898507880377E-16, 42.56828755692798438 ) ) ;
#13269 = FACE_BOUND ( 'NONE', #39205, .T. ) ;
#13270 = CARTESIAN_POINT ( 'NONE',  ( -50.13037131770486354, 2.688010569040066411, 741.9425600500171640 ) ) ;
#13271 = DIRECTION ( 'NONE',  ( 0.000000000000000000, 0.000000000000000000, 1.000000000000000000 ) ) ;
#13272 =( BOUNDED_CURVE ( )  B_SPLINE_CURVE ( 3, ( #29088, #9584, #25230, #40880 ),
 .UNSPECIFIED., .F., .F. ) 
 B_SPLINE_CURVE_WITH_KNOTS ( ( 4, 4 ),
 ( 1.570796326794896558, 3.141592653589793116 ),
 .UNSPECIFIED. ) 
 CURVE ( )  GEOMETRIC_REPRESENTATION_ITEM ( )  RATIONAL_B_SPLINE_CURVE ( ( 1.000000000000000000, 0.8047378541243649375, 0.8047378541243649375, 1.000000000000000000 ) ) 
 REPRESENTATION_ITEM ( '' )  );
#13273 = CYLINDRICAL_SURFACE ( 'NONE', #5971, 1.750000000000015543 ) ;
#13274 = EDGE_CURVE ( 'NONE', #11426, #2228, #1753, .T. ) ;
#13275 = FACE_OUTER_BOUND ( 'NONE', #41252, .T. ) ;
#13276 = CARTESIAN_POINT ( 'NONE',  ( 350.0000000000000000, -164.9999999999999432, 359.9999999999997726 ) ) ;
#13277 = LINE ( 'NONE', #2245, #33092 ) ;
#13278 = VECTOR ( 'NONE', #11968, 1000.000000000000000 ) ;
#13279 = ORIENTED_EDGE ( 'NONE', *, *, #2969, .F. ) ;
#13280 = DIRECTION ( 'NONE',  ( -0.000000000000000000, -0.000000000000000000, -1.000000000000000000 ) ) ;
#13281 = CARTESIAN_POINT ( 'NONE',  ( -84.94597344681494633, 2.143131898507880377E-16, -157.4317124430720582 ) ) ;
#13282 = CARTESIAN_POINT ( 'NONE',  ( 3.886636751349460628, -37.33392444503267171, 6.057468652304066836 ) ) ;
#13283 = EDGE_CURVE ( 'NONE', #41907, #16490, #37180, .T. ) ;
#13284 = EDGE_CURVE ( 'NONE', #6842, #41828, #49154, .T. ) ;
#13285 = DIRECTION ( 'NONE',  ( -0.000000000000000000, -0.000000000000000000, -1.000000000000000000 ) ) ;
#13286 = MECHANICAL_DESIGN_GEOMETRIC_PRESENTATION_REPRESENTATION (  '', ( #39544 ), #16668 ) ;
#13288 = ORIENTED_EDGE ( 'NONE', *, *, #16440, .F. ) ;
#13287 = ADVANCED_FACE ( 'NONE', ( #25857, #5586 ), #21491, .T. ) ;
#13289 = CARTESIAN_POINT ( 'NONE',  ( -125.6708471809678542, 1.749999999999996891, -80.20683870891909351 ) ) ;
#13290 = EDGE_CURVE ( 'NONE', #41885, #10222, #33563, .T. ) ;
#13291 = VECTOR ( 'NONE', #1287, 1000.000000000000000 ) ;
#13292 = CARTESIAN_POINT ( 'NONE',  ( -5.000000000000000000, -184.7999999999999545, 359.7999999999997840 ) ) ;
#13293 = EDGE_LOOP ( 'NONE', ( #32537, #9073, #1670 ) ) ;
#13294 = EDGE_CURVE ( 'NONE', #35576, #18285, #10597, .T. ) ;
#13295 = FACE_OUTER_BOUND ( 'NONE', #12473, .T. ) ;
#13296 = CARTESIAN_POINT ( 'NONE',  ( 214.9999999999999432, 173.0000000000000000, 352.0000000000000000 ) ) ;
#13297 = PLANE ( 'NONE',  #25179 ) ;
#13298 = ADVANCED_FACE ( 'NONE', ( #45068 ), #41245, .T. ) ;
#13299 = ORIENTED_EDGE ( 'NONE', *, *, #37460, .T. ) ;
#13300 = CARTESIAN_POINT ( 'NONE',  ( -0.4402108221912932051, 2.015156302359635720, 9.891980816043068003 ) ) ;
#13301 = B_SPLINE_SURFACE_WITH_KNOTS ( 'NONE', 3, 3, ( 
 ( #2151, #44955, #22148, #14174 ),
 ( #25487, #32688, #45459, #10354 ),
 ( #28838, #26005, #25747, #49036 ),
 ( #40887, #1399, #13182, #25239 ) ),
 .UNSPECIFIED., .F., .F., .F.,
 ( 4, 4 ),
 ( 4, 4 ),
 ( 0.000000000000000000, 1.000000000000000000 ),
 ( 0.000000000000000000, 1.000000000000000000 ),
 .UNSPECIFIED. ) ;
#13302 = ORIENTED_EDGE ( 'NONE', *, *, #13978, .F. ) ;
#13303 = VERTEX_POINT ( 'NONE', #2000 ) ;
#13304 = VERTEX_POINT ( 'NONE', #6100 ) ;
#13305 = FACE_OUTER_BOUND ( 'NONE', #40318, .T. ) ;
#13306 = CARTESIAN_POINT ( 'NONE',  ( 75.05402655318509630, 1.025126265847089657, -80.93171244307201562 ) ) ;
#13307 = VERTEX_POINT ( 'NONE', #21999 ) ;
#13308 = DIRECTION ( 'NONE',  ( 0.000000000000000000, 0.000000000000000000, 1.000000000000000000 ) ) ;
#13309 = DIRECTION ( 'NONE',  ( 0.9770330068457271366, 0.000000000000000000, 0.2130880182788258970 ) ) ;
#13310 = DIRECTION ( 'NONE',  ( -0.000000000000000000, -1.000000000000000000, -0.000000000000000000 ) ) ;
#13311 = VECTOR ( 'NONE', #23434, 1000.000000000000000 ) ;
#13312 = FACE_OUTER_BOUND ( 'NONE', #18532, .T. ) ;
#13313 = EDGE_CURVE ( 'NONE', #50400, #7894, #23724, .T. ) ;
#13314 = ORIENTED_EDGE ( 'NONE', *, *, #43350, .T. ) ;
#13315 = CARTESIAN_POINT ( 'NONE',  ( -46.69597344681494633, 0.000000000000000000, 165.0000000000000000 ) ) ;
#13316 = EDGE_CURVE ( 'NONE', #4874, #40803, #19257, .T. ) ;
#13317 = ORIENTED_EDGE ( 'NONE', *, *, #8467, .T. ) ;
#13318 = EDGE_CURVE ( 'NONE', #6437, #15488, #48645, .T. ) ;
#13319 = DIRECTION ( 'NONE',  ( 0.000000000000000000, 0.000000000000000000, 1.000000000000000000 ) ) ;
#13320 = EDGE_LOOP ( 'NONE', ( #31388, #2354, #17250, #12331, #27032, #48552 ) ) ;
#13321 = VECTOR ( 'NONE', #23652, 1000.000000000000000 ) ;
#13322 = ORIENTED_EDGE ( 'NONE', *, *, #19405, .T. ) ;
#13323 = ORIENTED_EDGE ( 'NONE', *, *, #3186, .T. ) ;
#13324 = FACE_OUTER_BOUND ( 'NONE', #7773, .T. ) ;
#13325 = VECTOR ( 'NONE', #48943, 1000.000000000000000 ) ;
#13326 = DIRECTION ( 'NONE',  ( -0.000000000000000000, -0.000000000000000000, 1.000000000000000000 ) ) ;
#13327 = ORIENTED_EDGE ( 'NONE', *, *, #18324, .F. ) ;
#13328 = AXIS2_PLACEMENT_3D ( 'NONE', #47712, #37499, #21560 ) ;
#13329 = EDGE_CURVE ( 'NONE', #19934, #42661, #25605, .T. ) ;
#13330 = CARTESIAN_POINT ( 'NONE',  ( -1.114871695981121125, 0.4953159757245923500, 9.963925895596188909 ) ) ;
#13331 = CARTESIAN_POINT ( 'NONE',  ( -84.94597344681494633, 2.143131898507880377E-16, 79.06828755692797017 ) ) ;
#13332 = DIRECTION ( 'NONE',  ( -0.000000000000000000, -0.000000000000000000, -1.000000000000000000 ) ) ;
#13333 = AXIS2_PLACEMENT_3D ( 'NONE', #45347, #29732, #22025 ) ;
#13334 = ORIENTED_EDGE ( 'NONE', *, *, #3735, .T. ) ;
#13335 = CARTESIAN_POINT ( 'NONE',  ( 181.0000000000000568, 175.0000000000000284, 339.9999999999998863 ) ) ;
#13336 = CARTESIAN_POINT ( 'NONE',  ( 166.9999999999999716, -81.49999999999997158, -115.0000000000001563 ) ) ;
#13337 = CARTESIAN_POINT ( 'NONE',  ( 20.21530556545302559, -31.58467066308217497, -9.422646554964174470 ) ) ;
#13338 = EDGE_LOOP ( 'NONE', ( #4031, #28848, #46401, #45540, #37037, #27413 ) ) ;
#13339 = EDGE_CURVE ( 'NONE', #8304, #40728, #34076, .T. ) ;
#13340 = ORIENTED_EDGE ( 'NONE', *, *, #47793, .T. ) ;
#13341 = APPLICATION_PROTOCOL_DEFINITION ( 'draft international standard', 'automotive_design', 1998, #35511 ) ;
#13342 = LINE ( 'NONE', #28255, #36815 ) ;
#13343 = LINE ( 'NONE', #39813, #36532 ) ;
#13344 = ADVANCED_FACE ( 'NONE', ( #29963 ), #28946, .F. ) ;
#13345 = CARTESIAN_POINT ( 'NONE',  ( -17.51065725283106289, 28.41934970907792746, -9.367992836599954742 ) ) ;
#13346 = CARTESIAN_POINT ( 'NONE',  ( -14.91630425054805187, 7.943683830272224355, -9.008049429158100807 ) ) ;
#13347 = ORIENTED_EDGE ( 'NONE', *, *, #32223, .T. ) ;
#13348 = CYLINDRICAL_SURFACE ( 'NONE', #30441, 1.750000000000001554 ) ;
#13349 = CARTESIAN_POINT ( 'NONE',  ( -556.7900739183570522, 54.43801056904003133, -65.53102910462104091 ) ) ;
#13350 = CARTESIAN_POINT ( 'NONE',  ( -4.999999999999948486, -204.9999999999999716, -230.2499999999999716 ) ) ;
#13351 = DIRECTION ( 'NONE',  ( -1.000000000000000000, 0.000000000000000000, -0.000000000000000000 ) ) ;
#13353 = EDGE_LOOP ( 'NONE', ( #14141, #47914, #1966, #11450 ) ) ;
#13352 = EDGE_CURVE ( 'NONE', #46080, #46658, #17647, .T. ) ;
#13354 = DIRECTION ( 'NONE',  ( -0.000000000000000000, -1.000000000000000000, -0.000000000000000000 ) ) ;
#13355 = EDGE_CURVE ( 'NONE', #45423, #3850, #44822, .T. ) ;
#13356 = ORIENTED_EDGE ( 'NONE', *, *, #47630, .T. ) ;
#13357 = CARTESIAN_POINT ( 'NONE',  ( 26.18032376592674737, -21.95228666728361233, 7.455576670931136185 ) ) ;
#13358 = AXIS2_PLACEMENT_3D ( 'NONE', #11992, #8398, #39454 ) ;
#13359 = ORIENTED_EDGE ( 'NONE', *, *, #18113, .F. ) ;
#13360 = CARTESIAN_POINT ( 'NONE',  ( -124.9459734468149463, 2.143131898507847836E-16, 165.0000000000000000 ) ) ;
#13361 = AXIS2_PLACEMENT_3D ( 'NONE', #8766, #12336, #32106 ) ;
#13362 = CARTESIAN_POINT ( 'NONE',  ( -86.69597344681496054, 0.000000000000000000, 165.0000000000000000 ) ) ;
#13363 = ADVANCED_FACE ( 'NONE', ( #45319 ), #9442, .T. ) ;
#13364 =( LENGTH_UNIT ( ) NAMED_UNIT ( * ) SI_UNIT ( .MILLI., .METRE. ) );
#13365 = VERTEX_POINT ( 'NONE', #5849 ) ;
#13366 = VECTOR ( 'NONE', #41953, 1000.000000000000000 ) ;
#13367 = ADVANCED_FACE ( 'NONE', ( #17885 ), #4024, .F. ) ;
#13368 = EDGE_CURVE ( 'NONE', #4257, #8296, #39192, .T. ) ;
#13369 = CARTESIAN_POINT ( 'NONE',  ( 0.7658683902953711264, -0.9641952520609267108, 9.975326647350893694 ) ) ;
#13370 = AXIS2_PLACEMENT_3D ( 'NONE', #4658, #4889, #47701 ) ;
#13371 = ORIENTED_EDGE ( 'NONE', *, *, #35080, .T. ) ;
#13372 = CARTESIAN_POINT ( 'NONE',  ( 344.0000000000000568, 167.0000000000000000, 341.9999999999998295 ) ) ;
#13373 = CARTESIAN_POINT ( 'NONE',  ( 3.231548175622897645, -9.463461120997347820, 9.282506307616472441 ) ) ;
#13374 = DIRECTION ( 'NONE',  ( -0.000000000000000000, -1.000000000000000000, -0.000000000000000000 ) ) ;
#13375 = CYLINDRICAL_SURFACE ( 'NONE', #19311, 1.750000000000008438 ) ;
#13376 = CARTESIAN_POINT ( 'NONE',  ( 135.0000000000003411, 17.00000000000000000, -60.00000000000000000 ) ) ;
#13377 = VERTEX_POINT ( 'NONE', #18893 ) ;
#13378 = ORIENTED_EDGE ( 'NONE', *, *, #31800, .T. ) ;
#13379 = FACE_OUTER_BOUND ( 'NONE', #18837, .T. ) ;
#13380 = ORIENTED_EDGE ( 'NONE', *, *, #12112, .T. ) ;
#13381 = ADVANCED_FACE ( 'NONE', ( #34572 ), #21505, .T. ) ;
#13382 = FACE_OUTER_BOUND ( 'NONE', #21860, .T. ) ;
#13383 = VERTEX_POINT ( 'NONE', #49659 ) ;
#13384 = CARTESIAN_POINT ( 'NONE',  ( 0.08756411784060347259, -1.703854692067152676, 9.912102921404990497 ) ) ;
#13385 = CARTESIAN_POINT ( 'NONE',  ( 151.5540265531850537, 0.000000000000000000, 79.06828755692797017 ) ) ;
#13386 = ORIENTED_EDGE ( 'NONE', *, *, #11099, .T. ) ;
#13387 = DIRECTION ( 'NONE',  ( -0.000000000000000000, -0.000000000000000000, -1.000000000000000000 ) ) ;
#13388 = DIRECTION ( 'NONE',  ( -0.000000000000000000, -0.000000000000000000, -1.000000000000000000 ) ) ;
#13389 = CARTESIAN_POINT ( 'NONE',  ( -194.9999999999999432, 173.0000000000000000, 132.0000000000000000 ) ) ;
#13390 = CARTESIAN_POINT ( 'NONE',  ( 75.05402655318509630, -1.025126265847088991, -157.4317124430720582 ) ) ;
#13391 = ORIENTED_EDGE ( 'NONE', *, *, #33473, .F. ) ;
#13392 = ORIENTED_EDGE ( 'NONE', *, *, #18171, .F. ) ;
#13393 = AXIS2_PLACEMENT_3D ( 'NONE', #45403, #37016, #33156 ) ;
#13394 = ORIENTED_EDGE ( 'NONE', *, *, #25238, .F. ) ;
#13395 = DIRECTION ( 'NONE',  ( -0.000000000000000000, -0.000000000000000000, -1.000000000000000000 ) ) ;
#13396 = CARTESIAN_POINT ( 'NONE',  ( 14.91630425054810161, -7.943683830272122215, -9.008049429158100807 ) ) ;
#13397 = VECTOR ( 'NONE', #37088, 1000.000000000000000 ) ;
#13398 = DIRECTION ( 'NONE',  ( 0.000000000000000000, 0.000000000000000000, 1.000000000000000000 ) ) ;
#13399 = FACE_OUTER_BOUND ( 'NONE', #20074, .T. ) ;
#13400 = ORIENTED_EDGE ( 'NONE', *, *, #17678, .T. ) ;
#13401 = LINE ( 'NONE', #36787, #6199 ) ;
#13402 = EDGE_LOOP ( 'NONE', ( #16924, #21158, #33097, #40111, #37212, #36131 ) ) ;
#13403 = CARTESIAN_POINT ( 'NONE',  ( -25.79500241909648395, 7.611558401714507482, 229.0000000000000000 ) ) ;
#13404 = DIRECTION ( 'NONE',  ( -1.000000000000000000, -0.000000000000000000, -0.000000000000000000 ) ) ;
#13405 = DIRECTION ( 'NONE',  ( -1.000000000000000000, 0.000000000000000000, 0.000000000000000000 ) ) ;
#13406 = DIRECTION ( 'NONE',  ( 0.000000000000000000, -0.000000000000000000, -1.000000000000000000 ) ) ;
#13407 = DIRECTION ( 'NONE',  ( -1.000000000000000000, -0.000000000000000000, -0.000000000000000000 ) ) ;
#13408 = CARTESIAN_POINT ( 'NONE',  ( -128.4459734468149179, 0.000000000000000000, 165.0000000000000000 ) ) ;
#13409 = ORIENTED_EDGE ( 'NONE', *, *, #38710, .F. ) ;
#13410 = DIRECTION ( 'NONE',  ( 0.000000000000000000, 1.000000000000000000, 0.000000000000000000 ) ) ;
#13411 = B_SPLINE_SURFACE_WITH_KNOTS ( 'NONE', 3, 3, ( 
 ( #15873, #12516, #47126, #15615 ),
 ( #23306, #8434, #24088, #16128 ),
 ( #42795, #12029, #27171, #4071 ),
 ( #27672, #31026, #47374, #39233 ) ),
 .UNSPECIFIED., .F., .F., .F.,
 ( 4, 4 ),
 ( 4, 4 ),
 ( 0.000000000000000000, 1.000000000000000000 ),
 ( 0.000000000000000000, 1.000000000000000000 ),
 .UNSPECIFIED. ) ;
#13412 = CYLINDRICAL_SURFACE ( 'NONE', #12213, 1.750000000000001554 ) ;
#13413 = CARTESIAN_POINT ( 'NONE',  ( 341.9999999999999432, 174.9999999999996589, -356.0000000000003411 ) ) ;
#13414 = B_SPLINE_CURVE_WITH_KNOTS ( 'NONE', 3,
 ( #17493, #25448, #6442, #44659 ),
 .UNSPECIFIED., .F., .F.,
 ( 4, 4 ),
 ( 0.000000000000000000, 0.2637263876330696033 ),
 .UNSPECIFIED. ) ;
#13415 =( BOUNDED_CURVE ( )  B_SPLINE_CURVE ( 3, ( #15211, #30875, #31115, #22897 ),
 .UNSPECIFIED., .F., .F. ) 
 B_SPLINE_CURVE_WITH_KNOTS ( ( 4, 4 ),
 ( 0.000000000000000000, 1.570796326794896558 ),
 .UNSPECIFIED. ) 
 CURVE ( )  GEOMETRIC_REPRESENTATION_ITEM ( )  RATIONAL_B_SPLINE_CURVE ( ( 1.000000000000000000, 0.8047378541243649375, 0.8047378541243649375, 1.000000000000000000 ) ) 
 REPRESENTATION_ITEM ( '' )  );
#13416 = EDGE_CURVE ( 'NONE', #13689, #31054, #22051, .T. ) ;
#13417 = AXIS2_PLACEMENT_3D ( 'NONE', #48764, #37298, #22806 ) ;
#13418 = CARTESIAN_POINT ( 'NONE',  ( -0.7603004677363125463, 1.297166976436572750, 9.936141075511203624 ) ) ;
#13419 = ADVANCED_FACE ( 'NONE', ( #14548 ), #11467, .T. ) ;
#13420 = VERTEX_POINT ( 'NONE', #23257 ) ;
#13421 = CARTESIAN_POINT ( 'NONE',  ( 193.3040265531851105, 0.000000000000000000, -165.0000000000000000 ) ) ;
#13422 = VERTEX_POINT ( 'NONE', #46330 ) ;
#13423 = CARTESIAN_POINT ( 'NONE',  ( -4.945973446814903696, 2.143131898507912917E-16, -77.43171244307198720 ) ) ;
#13424 =( BOUNDED_CURVE ( )  B_SPLINE_CURVE ( 3, ( #7933, #38721, #31281, #229 ),
 .UNSPECIFIED., .F., .F. ) 
 B_SPLINE_CURVE_WITH_KNOTS ( ( 4, 4 ),
 ( 3.141592653589793116, 4.712388980384689674 ),
 .UNSPECIFIED. ) 
 CURVE ( )  GEOMETRIC_REPRESENTATION_ITEM ( )  RATIONAL_B_SPLINE_CURVE ( ( 1.000000000000000000, 0.8047378541243649375, 0.8047378541243649375, 1.000000000000000000 ) ) 
 REPRESENTATION_ITEM ( '' )  );
#13425 = LINE ( 'NONE', #40642, #37316 ) ;
#13426 = ADVANCED_FACE ( 'NONE', ( #26863 ), #5093, .T. ) ;
#13427 = CARTESIAN_POINT ( 'NONE',  ( 1.332485441698145534, -1.351730126698036827, 9.900811091504554184 ) ) ;
#13428 = ORIENTED_EDGE ( 'NONE', *, *, #3554, .F. ) ;
#13429 = EDGE_CURVE ( 'NONE', #47506, #16542, #44205, .T. ) ;
#13430 = ADVANCED_FACE ( 'NONE', ( #38940 ), #50670, .T. ) ;
#13431 = ORIENTED_EDGE ( 'NONE', *, *, #8899, .T. ) ;
#13432 = LINE ( 'NONE', #1895, #26241 ) ;
#13433 = VECTOR ( 'NONE', #31325, 1000.000000000000000 ) ;
#13434 = CARTESIAN_POINT ( 'NONE',  ( 339.9999999999998863, -180.9999999999999716, 339.9999999999997726 ) ) ;
#13435 = VECTOR ( 'NONE', #25312, 1000.000000000000000 ) ;
#13436 = FACE_OUTER_BOUND ( 'NONE', #18168, .T. ) ;
#13437 = CARTESIAN_POINT ( 'NONE',  ( 2.948105490344985480, 9.555557232197198658, 9.282506307616484875 ) ) ;
#13438 = AXIS2_PLACEMENT_3D ( 'NONE', #48643, #40501, #25602 ) ;
#13439 = EDGE_CURVE ( 'NONE', #19764, #42454, #45458, .T. ) ;
#13440 =( BOUNDED_CURVE ( )  B_SPLINE_CURVE ( 3, ( #31672, #3160, #11139, #18810 ),
 .UNSPECIFIED., .F., .F. ) 
 B_SPLINE_CURVE_WITH_KNOTS ( ( 4, 4 ),
 ( 4.712388980384689674, 6.283185307179586232 ),
 .UNSPECIFIED. ) 
 CURVE ( )  GEOMETRIC_REPRESENTATION_ITEM ( )  RATIONAL_B_SPLINE_CURVE ( ( 1.000000000000000000, 0.8047378541243649375, 0.8047378541243649375, 1.000000000000000000 ) ) 
 REPRESENTATION_ITEM ( '' )  );
#13441 = EDGE_LOOP ( 'NONE', ( #26361, #45805, #41824, #40753 ) ) ;
#13442 = ORIENTED_EDGE ( 'NONE', *, *, #28625, .F. ) ;
#13443 = CARTESIAN_POINT ( 'NONE',  ( 0.000000000000000000, 184.8000000000000114, -340.2000000000001592 ) ) ;
#13444 = AXIS2_PLACEMENT_3D ( 'NONE', #17661, #40518, #41019 ) ;
#13445 = LINE ( 'NONE', #44967, #26310 ) ;
#13446 = ORIENTED_EDGE ( 'NONE', *, *, #24457, .F. ) ;
#13447 = EDGE_LOOP ( 'NONE', ( #31735, #10288, #47367, #40265 ) ) ;
#13448 = CARTESIAN_POINT ( 'NONE',  ( -84.94597344681494633, 2.143131898507880377E-16, -40.93171244307202983 ) ) ;
#13449 = CARTESIAN_POINT ( 'NONE',  ( 191.5540265531851105, 0.000000000000000000, 165.0000000000000000 ) ) ;
#13450 = CARTESIAN_POINT ( 'NONE',  ( -22.69295089195507131, -45.31600496604688999, 7.455576670931136185 ) ) ;
#13451 = CARTESIAN_POINT ( 'NONE',  ( -1.468446590252919348, -0.3226319952343834063, 9.953784399990620813 ) ) ;
#13452 = ORIENTED_EDGE ( 'NONE', *, *, #9244, .F. ) ;
#13453 = ORIENTED_EDGE ( 'NONE', *, *, #47690, .T. ) ;
#13454 = ORIENTED_EDGE ( 'NONE', *, *, #32507, .F. ) ;
#13455 = DIRECTION ( 'NONE',  ( 0.000000000000000000, -0.9749645535258953943, -0.2223603367690637489 ) ) ;
#13456 = LINE ( 'NONE', #45483, #48590 ) ;
#13457 = AXIS2_PLACEMENT_3D ( 'NONE', #8440, #47130, #7676 ) ;
#13458 = ORIENTED_EDGE ( 'NONE', *, *, #1101, .F. ) ;
#13459 = ORIENTED_EDGE ( 'NONE', *, *, #39613, .F. ) ;
#13460 = CARTESIAN_POINT ( 'NONE',  ( -25.63461350838931097, 43.17876197216396150, -8.016098858316205167 ) ) ;
#13461 = LINE ( 'NONE', #31975, #42892 ) ;
#13462 = ORIENTED_EDGE ( 'NONE', *, *, #41488, .F. ) ;
#13463 = ORIENTED_EDGE ( 'NONE', *, *, #43129, .T. ) ;
#13464 = EDGE_CURVE ( 'NONE', #43486, #48005, #4041, .T. ) ;
#13465 = LINE ( 'NONE', #37597, #22519 ) ;
#13466 = FACE_OUTER_BOUND ( 'NONE', #28327, .T. ) ;
#13467 = ORIENTED_EDGE ( 'NONE', *, *, #44930, .T. ) ;
#13468 = CARTESIAN_POINT ( 'NONE',  ( -19.99999999999908695, 17.00000000000000000, -24.99999999999999289 ) ) ;
#13469 = CARTESIAN_POINT ( 'NONE',  ( 34.99999999999997868, 16.00000000000000000, -90.00000000000000000 ) ) ;
#13470 = FACE_OUTER_BOUND ( 'NONE', #9712, .T. ) ;
#13471 = DIRECTION ( 'NONE',  ( 0.000000000000000000, 0.000000000000000000, 1.000000000000000000 ) ) ;
#13472 = AXIS2_PLACEMENT_3D ( 'NONE', #28289, #43923, #8798 ) ;
#13473 = DIRECTION ( 'NONE',  ( -1.000000000000000000, 0.000000000000000000, 0.000000000000000000 ) ) ;
#13474 = ORIENTED_EDGE ( 'NONE', *, *, #11779, .T. ) ;
#13475 = VECTOR ( 'NONE', #7510, 1000.000000000000000 ) ;
#13476 = CARTESIAN_POINT ( 'NONE',  ( -34.08355720199904226, 2.371364769369340042, 7.455576670931136185 ) ) ;
#13477 = CYLINDRICAL_SURFACE ( 'NONE', #28970, 1.750000000000008438 ) ;
#13478 = DIRECTION ( 'NONE',  ( 1.000000000000000000, 0.000000000000000000, 0.000000000000000000 ) ) ;
#13479 = AXIS2_PLACEMENT_3D ( 'NONE', #19125, #15547, #34814 ) ;
#13480 = DIRECTION ( 'NONE',  ( -0.000000000000000000, -0.000000000000000000, -1.000000000000000000 ) ) ;
#13481 =( BOUNDED_CURVE ( )  B_SPLINE_CURVE ( 3, ( #49002, #29554, #25976, #10060 ),
 .UNSPECIFIED., .F., .F. ) 
 B_SPLINE_CURVE_WITH_KNOTS ( ( 4, 4 ),
 ( 3.141592653589793116, 4.712388980384689674 ),
 .UNSPECIFIED. ) 
 CURVE ( )  GEOMETRIC_REPRESENTATION_ITEM ( )  RATIONAL_B_SPLINE_CURVE ( ( 1.000000000000000000, 0.8047378541243649375, 0.8047378541243649375, 1.000000000000000000 ) ) 
 REPRESENTATION_ITEM ( '' )  );
#13482 = CARTESIAN_POINT ( 'NONE',  ( 31.55402655318503236, 0.000000000000000000, 122.5682875569279702 ) ) ;
#13483 = CARTESIAN_POINT ( 'NONE',  ( 341.6568542494923690, 185.0000000000000568, -360.0000000000001705 ) ) ;
#13484 = LINE ( 'NONE', #17088, #18099 ) ;
#13485 = VERTEX_POINT ( 'NONE', #32242 ) ;
#13486 = CARTESIAN_POINT ( 'NONE',  ( -0.3370904143228963812, 0.2449105217885287067, 10.00000000000000000 ) ) ;
#13487 = VECTOR ( 'NONE', #44997, 1000.000000000000000 ) ;
#13488 = CARTESIAN_POINT ( 'NONE',  ( -114.9999999999978542, 16.00000000000000000, 95.00000000000000000 ) ) ;
#13489 = CIRCLE ( 'NONE', #15961, 40.00000000000000000 ) ;
#13490 = DIRECTION ( 'NONE',  ( -1.000000000000000000, 0.000000000000000000, 0.000000000000000000 ) ) ;
#13491 = EDGE_CURVE ( 'NONE', #49245, #39424, #23780, .T. ) ;
#13492 = PLANE ( 'NONE',  #2015 ) ;
#13493 = CARTESIAN_POINT ( 'NONE',  ( 195.0540265531851105, 2.143131898507880377E-16, 39.06828755692798438 ) ) ;
#13494 = ORIENTED_EDGE ( 'NONE', *, *, #12340, .T. ) ;
#13495 = LINE ( 'NONE', #25062, #40486 ) ;
#13496 = ORIENTED_EDGE ( 'NONE', *, *, #46870, .T. ) ;
#13497 = DIRECTION ( 'NONE',  ( -1.000000000000000000, -0.000000000000000000, -0.000000000000000000 ) ) ;
#13498 = CARTESIAN_POINT ( 'NONE',  ( 168.9999999999999716, -168.9999999999999432, -340.0000000000001137 ) ) ;
#13499 = ORIENTED_EDGE ( 'NONE', *, *, #11102, .F. ) ;
#13500 = DIRECTION ( 'NONE',  ( 1.000000000000000000, 0.000000000000000000, 0.000000000000000000 ) ) ;
#13501 = CARTESIAN_POINT ( 'NONE',  ( 164.9999999999999716, 16.00000000000000000, 115.0000000000000142 ) ) ;
#13502 = AXIS2_PLACEMENT_3D ( 'NONE', #8672, #11753, #12253 ) ;
#13503 = ORIENTED_EDGE ( 'NONE', *, *, #7027, .F. ) ;
#13504 = VERTEX_POINT ( 'NONE', #27637 ) ;
#13505 = VECTOR ( 'NONE', #25587, 1000.000000000000000 ) ;
#13506 = DIRECTION ( 'NONE',  ( 0.000000000000000000, 0.000000000000000000, 1.000000000000000000 ) ) ;
#13507 = CARTESIAN_POINT ( 'NONE',  ( 356.0000000000000000, 175.0000000000000284, -110.0000000000002132 ) ) ;
#13508 = CARTESIAN_POINT ( 'NONE',  ( -18.67411147745623978, -27.51799019669813973, -3.760136334089591248 ) ) ;
#13509 = EDGE_LOOP ( 'NONE', ( #40529, #36898, #39777, #14009 ) ) ;
#13510 = CARTESIAN_POINT ( 'NONE',  ( 33.30402655318503946, -1.750000000000009992, -159.1817124430720298 ) ) ;
#13511 = LINE ( 'NONE', #44798, #24740 ) ;
#13512 = VERTEX_POINT ( 'NONE', #35855 ) ;
#13513 =( BOUNDED_CURVE ( )  B_SPLINE_CURVE ( 3, ( #36144, #26283, #21928, #33985 ),
 .UNSPECIFIED., .F., .F. ) 
 B_SPLINE_CURVE_WITH_KNOTS ( ( 4, 4 ),
 ( 5.551115123125777022E-14, 1.570796326794896558 ),
 .UNSPECIFIED. ) 
 CURVE ( )  GEOMETRIC_REPRESENTATION_ITEM ( )  RATIONAL_B_SPLINE_CURVE ( ( 1.000000000000000000, 0.8047378541243781491, 0.8047378541243781491, 1.000000000000000000 ) ) 
 REPRESENTATION_ITEM ( '' )  );
#13514 = VERTEX_POINT ( 'NONE', #24039 ) ;
#13515 = ORIENTED_EDGE ( 'NONE', *, *, #18113, .T. ) ;
#13516 = CARTESIAN_POINT ( 'NONE',  ( 153.3040265531850537, -1.750000000000009992, 160.8182875569279702 ) ) ;
#13517 = CARTESIAN_POINT ( 'NONE',  ( -120.0000000000000426, 16.00000000000000000, -114.9999999999999858 ) ) ;
#13518 = ORIENTED_EDGE ( 'NONE', *, *, #14196, .T. ) ;
#13519 = EDGE_CURVE ( 'NONE', #46863, #19251, #945, .T. ) ;
#13520 = CARTESIAN_POINT ( 'NONE',  ( 0.9600884595229846052, -0.8493647100668649808, 9.957892297621013356 ) ) ;
#13521 = CARTESIAN_POINT ( 'NONE',  ( -36.70770892944847930, 7.840405911382138271, 6.057468652304065948 ) ) ;
#13522 = VECTOR ( 'NONE', #18339, 1000.000000000000000 ) ;
#13523 = LINE ( 'NONE', #2237, #22755 ) ;
#13524 = CARTESIAN_POINT ( 'NONE',  ( -0.7479701569695257346, -0.9668092547116119428, 9.969517326150317160 ) ) ;
#13525 = APPLICATION_CONTEXT ( 'automotive_design' ) ;
#13526 = CARTESIAN_POINT ( 'NONE',  ( 185.0000000000000000, -184.9999999999999716, -356.0000000000001705 ) ) ;
#13527 = AXIS2_PLACEMENT_3D ( 'NONE', #28631, #16841, #47592 ) ;
#13528 = CARTESIAN_POINT ( 'NONE',  ( 1.780619886013945052, 1.041246721325614466, 9.886433018048068178 ) ) ;
#13529 = DIRECTION ( 'NONE',  ( -0.000000000000000000, 1.000000000000000000, -2.406552799042969348E-16 ) ) ;
#13530 = CARTESIAN_POINT ( 'NONE',  ( -48.44597344681495343, 0.000000000000000000, 165.0000000000000000 ) ) ;
#13531 = CARTESIAN_POINT ( 'NONE',  ( 45.64490844644691236, 21.32281559348795952, 8.807470649214879543 ) ) ;
#13532 = CARTESIAN_POINT ( 'NONE',  ( 183.0000000000000000, -81.50000000000000000, -340.0000000000001137 ) ) ;
#13533 =( GEOMETRIC_REPRESENTATION_CONTEXT ( 3 ) GLOBAL_UNCERTAINTY_ASSIGNED_CONTEXT ( ( #3910 ) ) GLOBAL_UNIT_ASSIGNED_CONTEXT ( ( #38612, #3427, #30914 ) ) REPRESENTATION_CONTEXT ( 'NONE', 'WORKASPACE' ) );
#13535 = VECTOR ( 'NONE', #36197, 1000.000000000000000 ) ;
#13534 = DIRECTION ( 'NONE',  ( -1.000000000000000000, 0.000000000000000000, -0.000000000000000000 ) ) ;
#13536 = ORIENTED_EDGE ( 'NONE', *, *, #37344, .T. ) ;
#13537 = CARTESIAN_POINT ( 'NONE',  ( 181.0000000000000284, -174.9999999999999716, -113.0000000000001563 ) ) ;
#13538 = PLANE ( 'NONE',  #6980 ) ;
#13539 = VERTEX_POINT ( 'NONE', #42679 ) ;
#13540 = AXIS2_PLACEMENT_3D ( 'NONE', #40495, #24588, #25341 ) ;
#13541 = CARTESIAN_POINT ( 'NONE',  ( -9.999630309108516357, -0.09931773306744247354, 9.289350385289115053 ) ) ;
#13542 = ORIENTED_EDGE ( 'NONE', *, *, #1102, .T. ) ;
#13543 = CARTESIAN_POINT ( 'NONE',  ( 31.55402655318503236, 0.000000000000000000, -80.93171244307204404 ) ) ;
#13544 = CARTESIAN_POINT ( 'NONE',  ( 181.0000000000000284, 2.775557561562891351E-14, -97.00000000000014211 ) ) ;
#13545 = VERTEX_POINT ( 'NONE', #680 ) ;
#13546 = CARTESIAN_POINT ( 'NONE',  ( -7.721099712662037540, -1.750000000000023537, 119.7931612910808781 ) ) ;
#13547 = ADVANCED_FACE ( 'NONE', ( #8640 ), #20420, .T. ) ;
#13548 = LINE ( 'NONE', #21500, #49393 ) ;
#13549 = DIRECTION ( 'NONE',  ( -0.000000000000000000, -1.000000000000000000, -0.000000000000000000 ) ) ;
#13550 = ORIENTED_EDGE ( 'NONE', *, *, #21784, .T. ) ;
#13551 = CARTESIAN_POINT ( 'NONE',  ( -208.4459734468149463, 0.000000000000000000, 122.5682875569279702 ) ) ;
#13552 = ORIENTED_EDGE ( 'NONE', *, *, #12792, .T. ) ;
#13553 = ORIENTED_EDGE ( 'NONE', *, *, #37138, .F. ) ;
#13554 = LINE ( 'NONE', #32126, #40190 ) ;
#13555 = VECTOR ( 'NONE', #11110, 1000.000000000000227 ) ;
#13556 = ORIENTED_EDGE ( 'NONE', *, *, #27593, .F. ) ;
#13557 = CARTESIAN_POINT ( 'NONE',  ( 135.0000000000015632, 17.00000000000000000, 60.00000000000000000 ) ) ;
#13558 = CARTESIAN_POINT ( 'NONE',  ( 0.3370904143228959926, -0.2449105217885284291, 10.00000000000000000 ) ) ;
#13559 = AXIS2_PLACEMENT_3D ( 'NONE', #36069, #36592, #43492 ) ;
#13560 = ORIENTED_EDGE ( 'NONE', *, *, #49690, .T. ) ;
#13561 = DIRECTION ( 'NONE',  ( -0.000000000000000000, -1.000000000000000000, -0.000000000000000000 ) ) ;
#13562 = CARTESIAN_POINT ( 'NONE',  ( 31.55402655318503236, 1.025126265847089213, -0.9317124430720324924 ) ) ;
#13563 = EDGE_CURVE ( 'NONE', #4867, #29402, #20174, .T. ) ;
#13564 = LINE ( 'NONE', #33340, #26551 ) ;
#13565 = AXIS2_PLACEMENT_3D ( 'NONE', #27569, #24220, #39882 ) ;
#13566 = EDGE_CURVE ( 'NONE', #38882, #2039, #8139, .T. ) ;
#13567 = CARTESIAN_POINT ( 'NONE',  ( 32.27890028733795447, 1.750000000000009326, 1.843413822775066269 ) ) ;
#13568 = ORIENTED_EDGE ( 'NONE', *, *, #2632, .T. ) ;
#13569 = PLANE ( 'NONE',  #9196 ) ;
#13570 = EDGE_CURVE ( 'NONE', #5553, #22510, #19602, .T. ) ;
#13571 =( BOUNDED_CURVE ( )  B_SPLINE_CURVE ( 3, ( #6598, #22253, #1997, #17881 ),
 .UNSPECIFIED., .F., .F. ) 
 B_SPLINE_CURVE_WITH_KNOTS ( ( 4, 4 ),
 ( 3.141592653589793116, 4.712388980384689674 ),
 .UNSPECIFIED. ) 
 CURVE ( )  GEOMETRIC_REPRESENTATION_ITEM ( )  RATIONAL_B_SPLINE_CURVE ( ( 1.000000000000000000, 0.8047378541243649375, 0.8047378541243649375, 1.000000000000000000 ) ) 
 REPRESENTATION_ITEM ( '' )  );
#13572 = VECTOR ( 'NONE', #2531, 1000.000000000000000 ) ;
#13573 = EDGE_LOOP ( 'NONE', ( #7006, #42644, #45732, #25475, #44998, #23480, #39214, #16931 ) ) ;
#13574 = CARTESIAN_POINT ( 'NONE',  ( 0.000000000000000000, 326.6272189349111841, 136.0946745562129649 ) ) ;
#13575 = CARTESIAN_POINT ( 'NONE',  ( 8.001683061421385190, 5.997755262142701937, 9.282506307616484875 ) ) ;
#13576 = ORIENTED_EDGE ( 'NONE', *, *, #31226, .T. ) ;
#13577 = AXIS2_PLACEMENT_3D ( 'NONE', #19777, #24408, #27488 ) ;
#13578 = ORIENTED_EDGE ( 'NONE', *, *, #34700, .T. ) ;
#13579 = ORIENTED_EDGE ( 'NONE', *, *, #9817, .F. ) ;
#13580 = DIRECTION ( 'NONE',  ( 0.000000000000000000, 0.000000000000000000, 1.000000000000000000 ) ) ;
#13581 =( BOUNDED_CURVE ( )  B_SPLINE_CURVE ( 3, ( #28514, #44139, #9011, #24665 ),
 .UNSPECIFIED., .F., .F. ) 
 B_SPLINE_CURVE_WITH_KNOTS ( ( 4, 4 ),
 ( 3.140184917367520258E-16, 1.570796326794896780 ),
 .UNSPECIFIED. ) 
 CURVE ( )  GEOMETRIC_REPRESENTATION_ITEM ( )  RATIONAL_B_SPLINE_CURVE ( ( 1.000000000000000000, 0.8047378541243649375, 0.8047378541243649375, 1.000000000000000000 ) ) 
 REPRESENTATION_ITEM ( '' )  );
#13582 = PLANE ( 'NONE',  #15202 ) ;
#13583 = EDGE_CURVE ( 'NONE', #43433, #9119, #6526, .T. ) ;
#13584 = ORIENTED_EDGE ( 'NONE', *, *, #41556, .F. ) ;
#13585 = ADVANCED_FACE ( 'NONE', ( #15824 ), #5022, .T. ) ;
#13586 = VECTOR ( 'NONE', #33808, 1000.000000000000000 ) ;
#13587 = VECTOR ( 'NONE', #13857, 1000.000000000000000 ) ;
#13588 = CARTESIAN_POINT ( 'NONE',  ( -42.51732812238059722, -47.49695244670218131, -5.000000000000000000 ) ) ;
#13589 = DIRECTION ( 'NONE',  ( 0.000000000000000000, 0.000000000000000000, 1.000000000000000000 ) ) ;
#13590 = DIRECTION ( 'NONE',  ( 1.000000000000000000, -1.331116318405244905E-23, -4.759647537211363479E-16 ) ) ;
#13591 = EDGE_CURVE ( 'NONE', #20650, #28031, #8387, .T. ) ;
#13592 = ADVANCED_FACE ( 'NONE', ( #16081 ), #16584, .F. ) ;
#13593 = ORIENTED_EDGE ( 'NONE', *, *, #28633, .F. ) ;
#13594 = LINE ( 'NONE', #2547, #4019 ) ;
#13595 = CARTESIAN_POINT ( 'NONE',  ( 33.30402655318503946, 0.000000000000000000, 165.0000000000000000 ) ) ;
#13596 = EDGE_CURVE ( 'NONE', #34539, #28572, #10424, .T. ) ;
#13597 = CARTESIAN_POINT ( 'NONE',  ( 73.30402655318508209, 1.750000000000010658, -119.1817124430720440 ) ) ;
#13598 = VERTEX_POINT ( 'NONE', #48083 ) ;
#13599 = CARTESIAN_POINT ( 'NONE',  ( -206.6959734468149463, -1.750000000000010214, -39.18171244307202983 ) ) ;
#13600 = CARTESIAN_POINT ( 'NONE',  ( 168.9999999999999716, -252.5000000000000000, -114.9999999999999574 ) ) ;
#13601 = VECTOR ( 'NONE', #21330, 1000.000000000000000 ) ;
#13602 = DIRECTION ( 'NONE',  ( -1.000000000000000000, -0.000000000000000000, -0.000000000000000000 ) ) ;
#13603 = DIRECTION ( 'NONE',  ( -1.000000000000000000, 0.000000000000000000, 0.000000000000000000 ) ) ;
#13604 = VERTEX_POINT ( 'NONE', #187 ) ;
#13605 = CARTESIAN_POINT ( 'NONE',  ( -50.11058929355264979, 7.578863168071929834, 7.455576670931136185 ) ) ;
#13606 = CARTESIAN_POINT ( 'NONE',  ( 15.00000000000000000, -46.01315789473684248, -5.916985404131818171 ) ) ;
#13607 = DIRECTION ( 'NONE',  ( 2.220446049250312588E-16, 0.7071067811865475727, -0.7071067811865474617 ) ) ;
#13608 = CARTESIAN_POINT ( 'NONE',  ( 168.9999999999999716, -272.4999999999999432, -343.9999999999999432 ) ) ;
#13609 = EDGE_CURVE ( 'NONE', #28419, #33773, #28627, .T. ) ;
#13610 = VERTEX_POINT ( 'NONE', #47077 ) ;
#13611 = ADVANCED_FACE ( 'NONE', ( #12226 ), #43269, .F. ) ;
#13612 = LINE ( 'NONE', #14107, #5932 ) ;
#13613 = EDGE_LOOP ( 'NONE', ( #7551, #43012, #2246, #21443, #32571, #1736 ) ) ;
#13614 = EDGE_CURVE ( 'NONE', #30474, #8581, #1449, .T. ) ;
#13615 = CARTESIAN_POINT ( 'NONE',  ( 113.3040265531850537, -1.749999999999997113, -39.18171244307202983 ) ) ;
#13616 = VECTOR ( 'NONE', #29502, 1000.000000000000000 ) ;
#13617 = ORIENTED_EDGE ( 'NONE', *, *, #2147, .F. ) ;
#13618 = DIRECTION ( 'NONE',  ( -1.000000000000000000, -0.000000000000000000, -0.000000000000000000 ) ) ;
#13619 = EDGE_CURVE ( 'NONE', #33463, #40720, #10587, .T. ) ;
#13620 = DIRECTION ( 'NONE',  ( 0.000000000000000000, 0.000000000000000000, -1.000000000000000000 ) ) ;
#13621 = PLANE ( 'NONE',  #37174 ) ;
#13622 = VERTEX_POINT ( 'NONE', #17589 ) ;
#13623 = ADVANCED_FACE ( 'NONE', ( #10139 ), #6791, .T. ) ;
#13624 = CARTESIAN_POINT ( 'NONE',  ( -26.25702031264333058, 26.77347351953860155, 8.914903342594559632 ) ) ;
#13625 = VERTEX_POINT ( 'NONE', #26052 ) ;
#13626 = FACE_OUTER_BOUND ( 'NONE', #35626, .T. ) ;
#13627 = FACE_OUTER_BOUND ( 'NONE', #30325, .T. ) ;
#13628 = CARTESIAN_POINT ( 'NONE',  ( 0.000000000000000000, -397.9839762253770346, 197.0020682315616796 ) ) ;
#13629 = DIRECTION ( 'NONE',  ( 0.000000000000000000, 0.000000000000000000, 1.000000000000000000 ) ) ;
#13630 = DIRECTION ( 'NONE',  ( 0.000000000000000000, 0.000000000000000000, -1.000000000000000000 ) ) ;
#13631 = ORIENTED_EDGE ( 'NONE', *, *, #20926, .T. ) ;
#13632 = VERTEX_POINT ( 'NONE', #1693 ) ;
#13633 = CARTESIAN_POINT ( 'NONE',  ( 5.107674452598005566, -2.961810711067763169, 9.586754400234161366 ) ) ;
#13634 = EDGE_LOOP ( 'NONE', ( #8215, #41683, #12178, #21390, #14473, #45286, #8856, #43300 ) ) ;
#13635 = VECTOR ( 'NONE', #25190, 1000.000000000000000 ) ;
#13636 = CARTESIAN_POINT ( 'NONE',  ( -24.19621561048240821, -28.69654500124497076, -5.338708898921617596 ) ) ;
#13637 = DIRECTION ( 'NONE',  ( -0.000000000000000000, -0.000000000000000000, -1.000000000000000000 ) ) ;
#13638 = EDGE_CURVE ( 'NONE', #48180, #43354, #33760, .T. ) ;
#13639 = ORIENTED_EDGE ( 'NONE', *, *, #18399, .T. ) ;
#13640 = DIRECTION ( 'NONE',  ( -1.156482317317871478E-16, -1.000000000000000000, 0.000000000000000000 ) ) ;
#13641 = B_SPLINE_CURVE_WITH_KNOTS ( 'NONE', 3,
 ( #26876, #50164, #42511, #7388 ),
 .UNSPECIFIED., .F., .F.,
 ( 4, 4 ),
 ( 0.0004299334430849200642, 0.0007706806524479787148 ),
 .UNSPECIFIED. ) ;
#13642 = DIRECTION ( 'NONE',  ( -1.000000000000000000, -0.000000000000000000, -0.000000000000000000 ) ) ;
#13643 = ORIENTED_EDGE ( 'NONE', *, *, #8899, .F. ) ;
#13644 = EDGE_CURVE ( 'NONE', #12217, #42650, #49095, .T. ) ;
#13645 = CARTESIAN_POINT ( 'NONE',  ( -86.69597344681496054, 0.000000000000000000, 165.0000000000000000 ) ) ;
#13646 = CARTESIAN_POINT ( 'NONE',  ( 80.00000000000216005, 17.00000000000000000, 95.00000000000000000 ) ) ;
#13647 = CARTESIAN_POINT ( 'NONE',  ( 35.05402655318504657, 2.143131898507880377E-16, 159.0682875569279702 ) ) ;
#13649 = CIRCLE ( 'NONE', #34074, 0.5000000000000004441 ) ;
#13648 = CARTESIAN_POINT ( 'NONE',  ( 1.460157059060433360, -1.483633425177079745, 9.888808121373918070 ) ) ;
#13650 = EDGE_CURVE ( 'NONE', #19888, #25919, #11782, .T. ) ;
#13652 = ORIENTED_EDGE ( 'NONE', *, *, #10529, .T. ) ;
#13651 = EDGE_CURVE ( 'NONE', #48972, #23500, #6305, .T. ) ;
#13653 = ORIENTED_EDGE ( 'NONE', *, *, #43830, .F. ) ;
#13654 = VERTEX_POINT ( 'NONE', #29642 ) ;
#13655 = CARTESIAN_POINT ( 'NONE',  ( 42.99990394833793061, 47.95759300784327905, 5.000000000000000000 ) ) ;
#13656 = EDGE_CURVE ( 'NONE', #45648, #15688, #2387, .T. ) ;
#13657 = DIRECTION ( 'NONE',  ( 0.000000000000000000, 0.000000000000000000, 1.000000000000000000 ) ) ;
#13658 = CYLINDRICAL_SURFACE ( 'NONE', #40499, 4.000000000000003553 ) ;
#13659 = EDGE_CURVE ( 'NONE', #26096, #31600, #35040, .T. ) ;
#13660 = CYLINDRICAL_SURFACE ( 'NONE', #34623, 1.750000000000015543 ) ;
#13661 = ORIENTED_EDGE ( 'NONE', *, *, #20982, .T. ) ;
#13662 = AXIS2_PLACEMENT_3D ( 'NONE', #41773, #18421, #37954 ) ;
#13663 = DIRECTION ( 'NONE',  ( 1.860490536778032451E-50, 0.000000000000000000, -1.000000000000000000 ) ) ;
#13664 = ORIENTED_EDGE ( 'NONE', *, *, #30574, .T. ) ;
#13665 = DIRECTION ( 'NONE',  ( -0.000000000000000000, -0.000000000000000000, -1.000000000000000000 ) ) ;
#13666 = DIRECTION ( 'NONE',  ( -1.000000000000000000, -0.000000000000000000, -0.000000000000000000 ) ) ;
#13667 = LINE ( 'NONE', #48775, #26692 ) ;
#13668 = FACE_OUTER_BOUND ( 'NONE', #1328, .T. ) ;
#13669 = LINE ( 'NONE', #25731, #17594 ) ;
#13670 = CARTESIAN_POINT ( 'NONE',  ( -5.000000000000000000, -165.1999999999999602, 340.1999999999997044 ) ) ;
#13671 = ORIENTED_EDGE ( 'NONE', *, *, #31288, .T. ) ;
#13672 = DIRECTION ( 'NONE',  ( 0.000000000000000000, 0.000000000000000000, -1.000000000000000000 ) ) ;
#13673 = FACE_OUTER_BOUND ( 'NONE', #11787, .T. ) ;
#13674 = CYLINDRICAL_SURFACE ( 'NONE', #25807, 2.000000000000001776 ) ;
#13675 = PLANE ( 'NONE',  #36363 ) ;
#13676 = ORIENTED_EDGE ( 'NONE', *, *, #12070, .F. ) ;
#13677 = ADVANCED_FACE ( 'NONE', ( #25289 ), #48846, .F. ) ;
#13678 = CARTESIAN_POINT ( 'NONE',  ( 35.00000000000152767, 17.00000000000000000, 35.00000000000000000 ) ) ;
#13679 = ORIENTED_EDGE ( 'NONE', *, *, #13355, .F. ) ;
#13680 = LINE ( 'NONE', #44946, #31163 ) ;
#13681 = CARTESIAN_POINT ( 'NONE',  ( -114.9999999999987779, 16.00000000000000000, 30.00000000000000000 ) ) ;
#13682 = DIRECTION ( 'NONE',  ( 9.711650524620651178E-33, -1.223873602809432483E-48, 1.000000000000000000 ) ) ;
#13683 = ORIENTED_EDGE ( 'NONE', *, *, #28630, .T. ) ;
#13684 = CARTESIAN_POINT ( 'NONE',  ( -69.99999999999909051, 16.00000000000000000, -24.99999999999999289 ) ) ;
#13685 = CARTESIAN_POINT ( 'NONE',  ( 1.011271242968694084, -0.7347315653655782652, -3.333333333333333481 ) ) ;
#13686 = CARTESIAN_POINT ( 'NONE',  ( 210.0000000000000568, 0.000000000000000000, 160.8182875569279702 ) ) ;
#13687 = CARTESIAN_POINT ( 'NONE',  ( 49.67735855322978011, -8.912210285361751971, 8.356839323120299312 ) ) ;
#13688 = EDGE_CURVE ( 'NONE', #12938, #36125, #9888, .T. ) ;
#13689 = VERTEX_POINT ( 'NONE', #21684 ) ;
#13690 = ORIENTED_EDGE ( 'NONE', *, *, #1060, .F. ) ;
#13691 = CARTESIAN_POINT ( 'NONE',  ( -2.178343065408716139, -16.64136160116211727, -9.233365092205394475 ) ) ;
#13692 = DIRECTION ( 'NONE',  ( -5.473822126268816076E-48, 1.000000000000000000, 1.654361225106055350E-24 ) ) ;
#13693 = EDGE_LOOP ( 'NONE', ( #25741, #30810, #30183, #11260 ) ) ;
#13694 = VERTEX_POINT ( 'NONE', #37375 ) ;
#13695 = LINE ( 'NONE', #29358, #8412 ) ;
#13696 = PLANE ( 'NONE',  #24152 ) ;
#13697 = LINE ( 'NONE', #48556, #25922 ) ;
#13698 = CARTESIAN_POINT ( 'NONE',  ( 195.0540265531851105, 2.143131898507880377E-16, -77.43171244307204404 ) ) ;
#13699 = ADVANCED_FACE ( 'NONE', ( #48336 ), #2198, .F. ) ;
#13700 = ORIENTED_EDGE ( 'NONE', *, *, #8625, .T. ) ;
#13701 = VERTEX_POINT ( 'NONE', #324 ) ;
#13702 = DIRECTION ( 'NONE',  ( 1.000000000000000000, -0.000000000000000000, -0.000000000000000000 ) ) ;
#13703 = CARTESIAN_POINT ( 'NONE',  ( 0.6721397084974982672, 9.977385840602783773, 2.154851817814940063E-15 ) ) ;
#13704 = EDGE_CURVE ( 'NONE', #30746, #31478, #12116, .T. ) ;
#13705 = EDGE_CURVE ( 'NONE', #3658, #21143, #12086, .T. ) ;
#13706 = AXIS2_PLACEMENT_3D ( 'NONE', #13880, #21090, #6210 ) ;
#13707 = ORIENTED_EDGE ( 'NONE', *, *, #4065, .F. ) ;
#13708 = EDGE_LOOP ( 'NONE', ( #24468, #48629, #46981, #15725, #48721, #14470 ) ) ;
#13709 = CARTESIAN_POINT ( 'NONE',  ( 210.0000000000000568, 0.000000000000000000, -39.18171244307202983 ) ) ;
#13710 = CARTESIAN_POINT ( 'NONE',  ( -45.21167770612412085, -22.65616271077779942, 7.906207997025717304 ) ) ;
#13711 = ADVANCED_FACE ( 'NONE', ( #4160 ), #35475, .F. ) ;
#13712 = VERTEX_POINT ( 'NONE', #12350 ) ;
#13713 = EDGE_LOOP ( 'NONE', ( #37142, #10769, #31318, #42080 ) ) ;
#13714 = EDGE_CURVE ( 'NONE', #45927, #19269, #40253, .T. ) ;
#13715 = CYLINDRICAL_SURFACE ( 'NONE', #32389, 2.000000000000001776 ) ;
#13716 = CARTESIAN_POINT ( 'NONE',  ( -0.1287570809895602630, -0.3962735484563142396, -10.00000000000000000 ) ) ;
#13717 = VERTEX_POINT ( 'NONE', #23407 ) ;
#13718 = EDGE_CURVE ( 'NONE', #43146, #35494, #26991, .T. ) ;
#13719 = FACE_OUTER_BOUND ( 'NONE', #18003, .T. ) ;
#13720 =( BOUNDED_CURVE ( )  B_SPLINE_CURVE ( 3, ( #37774, #26208, #14401, #25704 ),
 .UNSPECIFIED., .F., .F. ) 
 B_SPLINE_CURVE_WITH_KNOTS ( ( 4, 4 ),
 ( 0.000000000000000000, 1.570796326794896558 ),
 .UNSPECIFIED. ) 
 CURVE ( )  GEOMETRIC_REPRESENTATION_ITEM ( )  RATIONAL_B_SPLINE_CURVE ( ( 1.000000000000000000, 0.8047378541243649375, 0.8047378541243649375, 1.000000000000000000 ) ) 
 REPRESENTATION_ITEM ( '' )  );
#13721 = LINE ( 'NONE', #48578, #8229 ) ;
#13722 = CARTESIAN_POINT ( 'NONE',  ( 168.9999999999999716, -256.4999999999999432, -349.9999999999999432 ) ) ;
#13723 = CARTESIAN_POINT ( 'NONE',  ( -126.6959734468149321, 0.000000000000000000, 165.0000000000000000 ) ) ;
#13724 = CARTESIAN_POINT ( 'NONE',  ( 210.0000000000000568, 0.000000000000000000, 80.81828755692798438 ) ) ;
#13725 = ORIENTED_EDGE ( 'NONE', *, *, #7489, .F. ) ;
#13726 = FACE_OUTER_BOUND ( 'NONE', #2817, .T. ) ;
#13727 =( BOUNDED_CURVE ( )  B_SPLINE_CURVE ( 3, ( #23899, #35467, #315, #15954 ),
 .UNSPECIFIED., .F., .F. ) 
 B_SPLINE_CURVE_WITH_KNOTS ( ( 4, 4 ),
 ( 3.141592653589793116, 4.712388980384700332 ),
 .UNSPECIFIED. ) 
 CURVE ( )  GEOMETRIC_REPRESENTATION_ITEM ( )  RATIONAL_B_SPLINE_CURVE ( ( 1.000000000000000000, 0.8047378541243626060, 0.8047378541243626060, 1.000000000000000000 ) ) 
 REPRESENTATION_ITEM ( '' )  );
#13728 = DIRECTION ( 'NONE',  ( -1.000000000000000000, 0.000000000000000000, 0.000000000000000000 ) ) ;
#13729 = EDGE_CURVE ( 'NONE', #39145, #14767, #43837, .T. ) ;
#13730 = LINE ( 'NONE', #48584, #27747 ) ;
#13731 = CARTESIAN_POINT ( 'NONE',  ( 1.222012661920449439, -0.2471648704738783342, 9.981352469109934233 ) ) ;
#13732 = FACE_OUTER_BOUND ( 'NONE', #41282, .T. ) ;
#13733 = CARTESIAN_POINT ( 'NONE',  ( 151.5540265531850537, 0.000000000000000000, -80.93171244307201562 ) ) ;
#13734 = CARTESIAN_POINT ( 'NONE',  ( 181.0000000000000000, -268.5000000000000000, -114.9999999999999147 ) ) ;
#13735 = DIRECTION ( 'NONE',  ( 0.000000000000000000, 0.000000000000000000, 1.000000000000000000 ) ) ;
#13736 =( BOUNDED_CURVE ( )  B_SPLINE_CURVE ( 3, ( #6168, #7181, #22822, #49474 ),
 .UNSPECIFIED., .F., .F. ) 
 B_SPLINE_CURVE_WITH_KNOTS ( ( 4, 4 ),
 ( 3.141592653589793116, 4.712388980384689674 ),
 .UNSPECIFIED. ) 
 CURVE ( )  GEOMETRIC_REPRESENTATION_ITEM ( )  RATIONAL_B_SPLINE_CURVE ( ( 1.000000000000000000, 0.8047378541243649375, 0.8047378541243649375, 1.000000000000000000 ) ) 
 REPRESENTATION_ITEM ( '' )  );
#13737 = CARTESIAN_POINT ( 'NONE',  ( 30.77287599203632951, 12.70002479445995824, 3.199614146704519602 ) ) ;
#13738 = VERTEX_POINT ( 'NONE', #19535 ) ;
#13739 = DIRECTION ( 'NONE',  ( 0.000000000000000000, 1.000000000000000000, -1.544785076050074834E-48 ) ) ;
#13740 = CARTESIAN_POINT ( 'NONE',  ( -44.99506233596265048, -23.32283626942287569, 7.455576670931136185 ) ) ;
#13741 = CYLINDRICAL_SURFACE ( 'NONE', #49092, 1.749999999999987566 ) ;
#13742 = CARTESIAN_POINT ( 'NONE',  ( 1.011271242968677653, 0.7347315653656002477, 3.333333333333333481 ) ) ;
#13743 = ORIENTED_EDGE ( 'NONE', *, *, #24341, .F. ) ;
#13744 = DIRECTION ( 'NONE',  ( -1.000000000000000000, -0.000000000000000000, -0.000000000000000000 ) ) ;
#13745 = EDGE_LOOP ( 'NONE', ( #24062, #21241, #1176, #1806, #4669, #48041 ) ) ;
#13746 = CARTESIAN_POINT ( 'NONE',  ( 0.000000000000000000, 6.912230148066165647, -5.000000000000000000 ) ) ;
#13747 = ADVANCED_FACE ( 'NONE', ( #11607 ), #64, .T. ) ;
#13748 = CARTESIAN_POINT ( 'NONE',  ( 1.780619886013945052, 1.041246721325614466, 9.886433018048068178 ) ) ;
#13749 = ORIENTED_EDGE ( 'NONE', *, *, #15563, .F. ) ;
#13750 = LINE ( 'NONE', #45032, #15575 ) ;
#13751 = LINE ( 'NONE', #47862, #6882 ) ;
#13752 = ORIENTED_EDGE ( 'NONE', *, *, #34971, .F. ) ;
#13753 = ORIENTED_EDGE ( 'NONE', *, *, #35680, .T. ) ;
#13754 = CARTESIAN_POINT ( 'NONE',  ( -1.249999999999999778, 0.000000000000000000, 10.00000000000000000 ) ) ;
#13755 = DIRECTION ( 'NONE',  ( 0.000000000000000000, -1.000000000000000000, -3.186989995019654210E-49 ) ) ;
#13756 = CARTESIAN_POINT ( 'NONE',  ( 21.61731705588930907, 25.43568671410602278, -9.367992836599954742 ) ) ;
#13757 = ORIENTED_EDGE ( 'NONE', *, *, #45371, .F. ) ;
#13758 = EDGE_CURVE ( 'NONE', #24673, #9673, #15698, .T. ) ;
#13759 = CARTESIAN_POINT ( 'NONE',  ( 33.89193117067290473, -21.24469349090191983, 910.0000000000000000 ) ) ;
#13760 = ADVANCED_FACE ( 'NONE', ( #39318 ), #43393, .F. ) ;
#13761 = CARTESIAN_POINT ( 'NONE',  ( 0.000000000000000000, -182.9999999999999716, -356.0000000000002274 ) ) ;
#13762 = DIRECTION ( 'NONE',  ( 0.000000000000000000, 1.000000000000000000, 0.000000000000000000 ) ) ;
#13763 = VERTEX_POINT ( 'NONE', #42632 ) ;
#13764 = VERTEX_POINT ( 'NONE', #7506 ) ;
#13765 = DIRECTION ( 'NONE',  ( 0.000000000000000000, 1.000000000000000000, 0.000000000000000000 ) ) ;
#13766 = DIRECTION ( 'NONE',  ( 1.000000000000000000, 0.000000000000000000, 0.000000000000000000 ) ) ;
#13767 = VERTEX_POINT ( 'NONE', #4410 ) ;
#13768 = EDGE_CURVE ( 'NONE', #49939, #36396, #3177, .T. ) ;
#13769 = LINE ( 'NONE', #25840, #19028 ) ;
#13770 = ADVANCED_FACE ( 'NONE', ( #575 ), #15201, .T. ) ;
#13771 = CARTESIAN_POINT ( 'NONE',  ( 111.5540265531850679, 0.000000000000000000, 165.0000000000000000 ) ) ;
#13772 = LINE ( 'NONE', #5575, #48414 ) ;
#13773 = VECTOR ( 'NONE', #36413, 1000.000000000000000 ) ;
#13774 = FACE_OUTER_BOUND ( 'NONE', #32709, .T. ) ;
#13775 = ADVANCED_FACE ( 'NONE', ( #7243, #46961 ), #34979, .T. ) ;
#13776 = CARTESIAN_POINT ( 'NONE',  ( 33.14391172085757375, 37.72293746533119929, -8.016098858316199838 ) ) ;
#13777 = CARTESIAN_POINT ( 'NONE',  ( -86.69597344681494633, -1.750000000000009992, -159.1817124430720298 ) ) ;
#13778 = LINE ( 'NONE', #25851, #15402 ) ;
#13779 = CARTESIAN_POINT ( 'NONE',  ( 191.5540265531850537, 1.025126265847089657, 79.06828755692797017 ) ) ;
#13780 = PLANE ( 'NONE',  #3577 ) ;
#13781 = VERTEX_POINT ( 'NONE', #27513 ) ;
#13782 = DIRECTION ( 'NONE',  ( 2.242130092700023170E-16, -0.7071067811865475727, 0.7071067811865474617 ) ) ;
#13783 = B_SPLINE_CURVE_WITH_KNOTS ( 'NONE', 3,
 ( #2223, #33527, #29668, #45289, #5561, #45040 ),
 .UNSPECIFIED., .F., .F.,
 ( 4, 2, 4 ),
 ( 3.127317220692751144E-18, 0.009882509389272367203, 0.01976501877854473094 ),
 .UNSPECIFIED. ) ;
#13784 = CARTESIAN_POINT ( 'NONE',  ( 153.3040265531850537, 0.000000000000000000, 165.0000000000000000 ) ) ;
#13785 = CARTESIAN_POINT ( 'NONE',  ( -164.9999999999990905, 16.00000000000000000, 0.000000000000000000 ) ) ;
#13786 = ORIENTED_EDGE ( 'NONE', *, *, #41008, .F. ) ;
#13787 = FACE_OUTER_BOUND ( 'NONE', #39519, .T. ) ;
#13788 = CARTESIAN_POINT ( 'NONE',  ( 30.00000000000187228, 17.00000000000000000, 65.00000000000000000 ) ) ;
#13789 = ORIENTED_EDGE ( 'NONE', *, *, #29996, .T. ) ;
#13790 = CARTESIAN_POINT ( 'NONE',  ( 153.3040265531850537, -1.750000000000010658, -119.1817124430720440 ) ) ;
#13791 = CARTESIAN_POINT ( 'NONE',  ( 30.00000000000217781, 17.00000000000000000, 95.00000000000000000 ) ) ;
#13792 = CARTESIAN_POINT ( 'NONE',  ( 39.35269538308637038, -42.31198943095992604, 742.8425600500171413 ) ) ;
#13793 = CYLINDRICAL_SURFACE ( 'NONE', #34015, 1.750000000000008438 ) ;
#13794 = ORIENTED_EDGE ( 'NONE', *, *, #26633, .T. ) ;
#13795 = SURFACE_STYLE_USAGE ( .BOTH. , #21261 ) ;
#13796 = ORIENTED_EDGE ( 'NONE', *, *, #39072, .T. ) ;
#13797 = ORIENTED_EDGE ( 'NONE', *, *, #10458, .T. ) ;
#13798 = EDGE_CURVE ( 'NONE', #35927, #1398, #40923, .T. ) ;
#13799 = PLANE ( 'NONE',  #11555 ) ;
#13800 = AXIS2_PLACEMENT_3D ( 'NONE', #5972, #41380, #37311 ) ;
#13801 = ORIENTED_EDGE ( 'NONE', *, *, #9600, .F. ) ;
#13802 = CARTESIAN_POINT ( 'NONE',  ( -168.4459734468149463, 0.000000000000000000, 42.56828755692798438 ) ) ;
#13803 = CARTESIAN_POINT ( 'NONE',  ( -194.9999999999999432, -172.9999999999999716, 232.0000000000000284 ) ) ;
#13804 = ORIENTED_EDGE ( 'NONE', *, *, #6040, .T. ) ;
#13805 = DIRECTION ( 'NONE',  ( 0.000000000000000000, -1.000000000000000000, -3.186989995019654210E-49 ) ) ;
#13806 = DIRECTION ( 'NONE',  ( -0.000000000000000000, 0.000000000000000000, 1.000000000000000000 ) ) ;
#13807 = FACE_OUTER_BOUND ( 'NONE', #3867, .T. ) ;
#13808 = B_SPLINE_CURVE_WITH_KNOTS ( 'NONE', 3,
 ( #8186, #12274, #7940, #26912 ),
 .UNSPECIFIED., .F., .F.,
 ( 4, 4 ),
 ( 0.9890644561681873892, 1.000000000000000000 ),
 .UNSPECIFIED. ) ;
#13809 = ORIENTED_EDGE ( 'NONE', *, *, #25295, .F. ) ;
#13810 = FACE_OUTER_BOUND ( 'NONE', #40579, .T. ) ;
#13811 = FACE_OUTER_BOUND ( 'NONE', #10793, .T. ) ;
#13812 = VERTEX_POINT ( 'NONE', #32119 ) ;
#13813 = CARTESIAN_POINT ( 'NONE',  ( 35.00000000000186162, 17.00000000000000000, 65.00000000000000000 ) ) ;
#13814 = LINE ( 'NONE', #5116, #19566 ) ;
#13815 = EDGE_LOOP ( 'NONE', ( #28967, #4364, #1304, #13347 ) ) ;
#13816 = ORIENTED_EDGE ( 'NONE', *, *, #9951, .T. ) ;
#13817 = ORIENTED_EDGE ( 'NONE', *, *, #14833, .T. ) ;
#13818 = LINE ( 'NONE', #45108, #49088 ) ;
#13819 = CARTESIAN_POINT ( 'NONE',  ( 151.5540265531850537, 2.143131898507880377E-16, -160.9317124430720298 ) ) ;
#13820 = B_SPLINE_SURFACE_WITH_KNOTS ( 'NONE', 3, 3, ( 
 ( #2292, #17193, #40294, #20781 ),
 ( #25653, #36461, #1303, #32864 ),
 ( #32604, #16950, #40544, #48188 ),
 ( #6147, #40795, #44367, #9487 ) ),
 .UNSPECIFIED., .F., .F., .F.,
 ( 4, 4 ),
 ( 4, 4 ),
 ( 0.000000000000000000, 1.000000000000000000 ),
 ( 0.000000000000000000, 1.000000000000000000 ),
 .UNSPECIFIED. ) ;
#13821 = ORIENTED_EDGE ( 'NONE', *, *, #16934, .F. ) ;
#13822 = LINE ( 'NONE', #6145, #31560 ) ;
#13823 = CARTESIAN_POINT ( 'NONE',  ( 1.250000000000000222, 0.000000000000000000, -10.00000000000000000 ) ) ;
#13824 = DIRECTION ( 'NONE',  ( -1.000000000000000000, -0.000000000000000000, -0.000000000000000000 ) ) ;
#13825 = FACE_OUTER_BOUND ( 'NONE', #695, .T. ) ;
#13826 = ORIENTED_EDGE ( 'NONE', *, *, #27439, .F. ) ;
#13827 = CARTESIAN_POINT ( 'NONE',  ( 35.05402655318504657, 1.025126265847089213, -0.9317124430720324924 ) ) ;
#13829 = ADVANCED_FACE ( 'NONE', ( #47714 ), #16707, .T. ) ;
#13828 = CYLINDRICAL_SURFACE ( 'NONE', #19367, 1.750000000000001554 ) ;
#13830 = CARTESIAN_POINT ( 'NONE',  ( 214.9999999999999432, 164.9999999999999716, 500.0000000000000000 ) ) ;
#13831 = VERTEX_POINT ( 'NONE', #1577 ) ;
#13832 = DIRECTION ( 'NONE',  ( -0.000000000000000000, -1.000000000000000000, -0.000000000000000000 ) ) ;
#13833 = CARTESIAN_POINT ( 'NONE',  ( -36.46533180484016157, -8.777022568848208195, -9.011255500499647297 ) ) ;
#13834 = VECTOR ( 'NONE', #49968, 1000.000000000000000 ) ;
#13835 = CARTESIAN_POINT ( 'NONE',  ( -0.9489147763969763005, 2.465022012282187536, 9.847478953136931779 ) ) ;
#13836 = CARTESIAN_POINT ( 'NONE',  ( 343.9999999999993747, 183.0000000000000568, 357.9999999999998295 ) ) ;
#13837 = VERTEX_POINT ( 'NONE', #47969 ) ;
#13838 = AXIS2_PLACEMENT_3D ( 'NONE', #44931, #33931, #25469 ) ;
#13839 = VECTOR ( 'NONE', #18681, 1000.000000000000000 ) ;
#13840 = CARTESIAN_POINT ( 'NONE',  ( -46.69597344681494633, 0.000000000000000000, 165.0000000000000000 ) ) ;
#13841 = AXIS2_PLACEMENT_3D ( 'NONE', #43323, #32055, #47897 ) ;
#13842 = CARTESIAN_POINT ( 'NONE',  ( -206.6959734468149463, 1.750000000000010658, 80.81828755692798438 ) ) ;
#13843 = FACE_OUTER_BOUND ( 'NONE', #61, .T. ) ;
#13844 = CARTESIAN_POINT ( 'NONE',  ( -3.996390545799824334, 16.57371371864897469, 8.953103998512858652 ) ) ;
#13845 = CARTESIAN_POINT ( 'NONE',  ( -47.72109971266203132, 1.750000000000010436, 79.79316129108087807 ) ) ;
#13846 = AXIS2_PLACEMENT_3D ( 'NONE', #21944, #37616, #2445 ) ;
#13847 = ORIENTED_EDGE ( 'NONE', *, *, #16062, .F. ) ;
#13848 = DIRECTION ( 'NONE',  ( -0.000000000000000000, 1.000000000000000000, -0.000000000000000000 ) ) ;
#13849 = ORIENTED_EDGE ( 'NONE', *, *, #26524, .F. ) ;
#13850 = CARTESIAN_POINT ( 'NONE',  ( -4.763548243873389154, 16.57409059453848599, 8.727788335465566760 ) ) ;
#13851 = VERTEX_POINT ( 'NONE', #40572 ) ;
#13852 = LINE ( 'NONE', #14111, #4119 ) ;
#13853 = DIRECTION ( 'NONE',  ( 1.000000000000000000, 0.000000000000000000, 0.000000000000000000 ) ) ;
#13854 = CARTESIAN_POINT ( 'NONE',  ( 75.05402655318509630, 2.143131898507880377E-16, 119.0682875569279560 ) ) ;
#13855 = EDGE_LOOP ( 'NONE', ( #4543, #24552, #33388, #40524 ) ) ;
#13856 =( BOUNDED_CURVE ( )  B_SPLINE_CURVE ( 3, ( #13898, #49519, #45685, #37303 ),
 .UNSPECIFIED., .F., .F. ) 
 B_SPLINE_CURVE_WITH_KNOTS ( ( 4, 4 ),
 ( 3.141592653589793116, 4.712388980384689674 ),
 .UNSPECIFIED. ) 
 CURVE ( )  GEOMETRIC_REPRESENTATION_ITEM ( )  RATIONAL_B_SPLINE_CURVE ( ( 1.000000000000000000, 0.8047378541243649375, 0.8047378541243649375, 1.000000000000000000 ) ) 
 REPRESENTATION_ITEM ( '' )  );
#13857 = DIRECTION ( 'NONE',  ( -1.000000000000000000, -0.000000000000000000, -0.000000000000000000 ) ) ;
#13858 = ORIENTED_EDGE ( 'NONE', *, *, #28790, .T. ) ;
#13859 = CARTESIAN_POINT ( 'NONE',  ( 210.0000000000000568, 2.143131898507880377E-16, -160.9317124430720298 ) ) ;
#13860 = DIRECTION ( 'NONE',  ( 1.000000000000000000, 0.000000000000000000, -0.000000000000000000 ) ) ;
#13861 = LINE ( 'NONE', #38273, #22945 ) ;
#13862 = DIRECTION ( 'NONE',  ( -1.000000000000000000, 3.172065745548403743E-16, -1.587271980518778491E-16 ) ) ;
#13863 = PLANE ( 'NONE',  #25749 ) ;
#13864 =( BOUNDED_CURVE ( )  B_SPLINE_CURVE ( 3, ( #25655, #30506, #45115, #14597 ),
 .UNSPECIFIED., .F., .F. ) 
 B_SPLINE_CURVE_WITH_KNOTS ( ( 4, 4 ),
 ( 4.712388980384689674, 6.283185307179586232 ),
 .UNSPECIFIED. ) 
 CURVE ( )  GEOMETRIC_REPRESENTATION_ITEM ( )  RATIONAL_B_SPLINE_CURVE ( ( 1.000000000000000000, 0.8047378541243649375, 0.8047378541243649375, 1.000000000000000000 ) ) 
 REPRESENTATION_ITEM ( '' )  );
#13865 = ORIENTED_EDGE ( 'NONE', *, *, #3919, .T. ) ;
#13866 = ORIENTED_EDGE ( 'NONE', *, *, #30254, .T. ) ;
#13867 = FACE_OUTER_BOUND ( 'NONE', #41845, .T. ) ;
#13868 = VECTOR ( 'NONE', #29345, 1000.000000000000000 ) ;
#13869 = AXIS2_PLACEMENT_3D ( 'NONE', #12601, #24674, #17222 ) ;
#13870 = CIRCLE ( 'NONE', #39290, 2.000000000000001776 ) ;
#13871 = ORIENTED_EDGE ( 'NONE', *, *, #7664, .T. ) ;
#13872 = CARTESIAN_POINT ( 'NONE',  ( 114.3291528190321173, -1.749999999999996669, 81.84341382277506227 ) ) ;
#13873 = LINE ( 'NONE', #37026, #1868 ) ;
#13874 = ORIENTED_EDGE ( 'NONE', *, *, #35351, .F. ) ;
#13875 = CARTESIAN_POINT ( 'NONE',  ( -168.4459734468149463, 0.000000000000000000, -37.43171244307205825 ) ) ;
#13876 = VECTOR ( 'NONE', #9480, 1000.000000000000000 ) ;
#13877 = B_SPLINE_CURVE_WITH_KNOTS ( 'NONE', 3,
 ( #29964, #14807, #37428, #18644 ),
 .UNSPECIFIED., .F., .F.,
 ( 4, 4 ),
 ( 8.673617379884035472E-19, 0.002458791966311098948 ),
 .UNSPECIFIED. ) ;
#13878 = CARTESIAN_POINT ( 'NONE',  ( 71.55402655318506788, 2.143131898507880377E-16, -160.9317124430720298 ) ) ;
#13879 = ORIENTED_EDGE ( 'NONE', *, *, #48708, .T. ) ;
#13880 = CARTESIAN_POINT ( 'NONE',  ( 135.0000000000006253, 17.00000000000000000, -54.99999999999999289 ) ) ;
#13881 = CARTESIAN_POINT ( 'NONE',  ( -114.9999999999981526, 17.00000000000000000, 90.00000000000000000 ) ) ;
#13882 = FACE_OUTER_BOUND ( 'NONE', #25310, .T. ) ;
#13883 = VECTOR ( 'NONE', #14501, 1000.000000000000000 ) ;
#13884 = FACE_OUTER_BOUND ( 'NONE', #19931, .T. ) ;
#13885 = ORIENTED_EDGE ( 'NONE', *, *, #38710, .T. ) ;
#13886 = EDGE_CURVE ( 'NONE', #42504, #46782, #47436, .T. ) ;
#13887 = ORIENTED_EDGE ( 'NONE', *, *, #19976, .T. ) ;
#13888 = EDGE_LOOP ( 'NONE', ( #32093, #6282, #12542, #13896, #963, #8091 ) ) ;
#13890 = EDGE_CURVE ( 'NONE', #3258, #49766, #32372, .T. ) ;
#13889 = CARTESIAN_POINT ( 'NONE',  ( -45.67084718096785423, -1.750000000000009548, 41.84341382277508359 ) ) ;
#13891 = CARTESIAN_POINT ( 'NONE',  ( -10.00419011302953010, 8.486842105263161073, -18.42339408367722697 ) ) ;
#13892 = CARTESIAN_POINT ( 'NONE',  ( 356.0000000000000000, -164.9999999999999432, 339.9999999999998295 ) ) ;
#13893 = ORIENTED_EDGE ( 'NONE', *, *, #28193, .T. ) ;
#13894 = ADVANCED_FACE ( 'NONE', ( #48719 ), #1443, .T. ) ;
#13895 = CARTESIAN_POINT ( 'NONE',  ( 0.2996946835594631597, 1.197003681518481910, 9.969907203203804968 ) ) ;
#13896 = ORIENTED_EDGE ( 'NONE', *, *, #2030, .F. ) ;
#13897 = ADVANCED_FACE ( 'NONE', ( #29020 ), #33143, .T. ) ;
#13898 = CARTESIAN_POINT ( 'NONE',  ( 195.0540265531851105, 2.143131898507880377E-16, -117.4317124430720725 ) ) ;
#13899 = CARTESIAN_POINT ( 'NONE',  ( 210.0000000000000568, 0.000000000000000000, -159.1817124430720298 ) ) ;
#13900 = CARTESIAN_POINT ( 'NONE',  ( -14.48769039275601145, -30.44468701195584970, 8.807470649214879543 ) ) ;
#13901 = FACE_OUTER_BOUND ( 'NONE', #27817, .T. ) ;
#13902 = DIRECTION ( 'NONE',  ( -1.000000000000000000, 0.000000000000000000, 0.000000000000000000 ) ) ;
#13903 = LINE ( 'NONE', #33688, #12528 ) ;
#13904 = ORIENTED_EDGE ( 'NONE', *, *, #14543, .F. ) ;
#13905 = CARTESIAN_POINT ( 'NONE',  ( 74.32915281903215998, -1.750000000000009548, 39.79316129108089228 ) ) ;
#13906 = FACE_OUTER_BOUND ( 'NONE', #49585, .T. ) ;
#13907 = LINE ( 'NONE', #20618, #40573 ) ;
#13908 = VECTOR ( 'NONE', #30051, 1000.000000000000000 ) ;
#13909 = AXIS2_PLACEMENT_3D ( 'NONE', #40446, #5283, #48591 ) ;
#13910 = CYLINDRICAL_SURFACE ( 'NONE', #42882, 2.000000000000001776 ) ;
#13911 = ORIENTED_EDGE ( 'NONE', *, *, #43711, .T. ) ;
#13912 = CARTESIAN_POINT ( 'NONE',  ( -1.011271242968688533, 0.7347315653655859258, -10.00000000000000000 ) ) ;
#13913 = ORIENTED_EDGE ( 'NONE', *, *, #12501, .F. ) ;
#13914 = VECTOR ( 'NONE', #40982, 1000.000000000000000 ) ;
#13915 = FACE_OUTER_BOUND ( 'NONE', #46248, .T. ) ;
#13916 = DIRECTION ( 'NONE',  ( -1.000000000000000000, 0.000000000000000000, -2.958228394578794270E-31 ) ) ;
#13917 = VECTOR ( 'NONE', #49950, 1000.000000000000000 ) ;
#13918 = EDGE_CURVE ( 'NONE', #43354, #12746, #16971, .T. ) ;
#13919 = DIRECTION ( 'NONE',  ( -1.000000000000000000, 0.000000000000000000, 0.000000000000000000 ) ) ;
#13920 = EDGE_CURVE ( 'NONE', #25110, #40222, #8796, .T. ) ;
#13921 = VECTOR ( 'NONE', #31063, 1000.000000000000000 ) ;
#13922 = EDGE_CURVE ( 'NONE', #48356, #49781, #20437, .T. ) ;
#13923 = EDGE_CURVE ( 'NONE', #29240, #20400, #26964, .T. ) ;
#13924 = CARTESIAN_POINT ( 'NONE',  ( 84.99999999999997158, 16.00000000000000000, -114.9999999999999858 ) ) ;
#13925 = ORIENTED_EDGE ( 'NONE', *, *, #38250, .F. ) ;
#13926 = CARTESIAN_POINT ( 'NONE',  ( 14.48769039275578407, 30.44468701195595983, 8.807470649214879543 ) ) ;
#13927 = PLANE ( 'NONE',  #33622 ) ;
#13928 = ADVANCED_FACE ( 'NONE', ( #44146 ), #5155, .T. ) ;
#13929 = DIRECTION ( 'NONE',  ( 0.000000000000000000, 0.000000000000000000, 1.000000000000000000 ) ) ;
#13930 = EDGE_CURVE ( 'NONE', #25904, #40604, #17320, .T. ) ;
#13931 = ORIENTED_EDGE ( 'NONE', *, *, #33839, .T. ) ;
#13932 = ORIENTED_EDGE ( 'NONE', *, *, #32620, .T. ) ;
#13933 = DIRECTION ( 'NONE',  ( -0.000000000000000000, -1.000000000000000000, -0.000000000000000000 ) ) ;
#13934 = CARTESIAN_POINT ( 'NONE',  ( -128.4459734468149179, 0.000000000000000000, 165.0000000000000000 ) ) ;
#13935 = ORIENTED_EDGE ( 'NONE', *, *, #33053, .F. ) ;
#13936 = ORIENTED_EDGE ( 'NONE', *, *, #4728, .T. ) ;
#13937 = CARTESIAN_POINT ( 'NONE',  ( -84.94597344681493212, -1.025126265847089435, -40.93171244307204404 ) ) ;
#13938 = CARTESIAN_POINT ( 'NONE',  ( -14.99999999999906919, 17.00000000000000000, 0.000000000000000000 ) ) ;
#13939 = CARTESIAN_POINT ( 'NONE',  ( 33.30402655318503946, 1.750000000000009992, 160.8182875569279702 ) ) ;
#13940 = DIRECTION ( 'NONE',  ( -1.000000000000000000, -0.000000000000000000, -0.000000000000000000 ) ) ;
#13941 = EDGE_LOOP ( 'NONE', ( #9778, #7947 ) ) ;
#13942 = DIRECTION ( 'NONE',  ( 0.000000000000000000, 0.000000000000000000, 1.000000000000000000 ) ) ;
#13943 = EDGE_LOOP ( 'NONE', ( #19817, #7842, #32479, #7731 ) ) ;
#13944 = EDGE_CURVE ( 'NONE', #8857, #47433, #43536, .T. ) ;
#13945 = LINE ( 'NONE', #49314, #48761 ) ;
#13946 = VECTOR ( 'NONE', #36881, 1000.000000000000000 ) ;
#13947 = DIRECTION ( 'NONE',  ( -0.000000000000000000, -0.000000000000000000, -1.000000000000000000 ) ) ;
#13948 = VECTOR ( 'NONE', #31052, 1000.000000000000000 ) ;
#13949 = EDGE_CURVE ( 'NONE', #42411, #21262, #18950, .T. ) ;
#13950 = ADVANCED_FACE ( 'NONE', ( #34155 ), #2077, .T. ) ;
#13951 = ORIENTED_EDGE ( 'NONE', *, *, #40394, .F. ) ;
#13952 = SHAPE_REPRESENTATION ( 'frame_Default<As Machined>', ( #45486 ), #41416 ) ;
#13953 = ORIENTED_EDGE ( 'NONE', *, *, #525, .F. ) ;
#13954 = VECTOR ( 'NONE', #1239, 1000.000000000000000 ) ;
#13955 = DIRECTION ( 'NONE',  ( -1.000000000000000000, 0.000000000000000000, 0.000000000000000000 ) ) ;
#13956 = VECTOR ( 'NONE', #36595, 1000.000000000000000 ) ;
#13957 = ORIENTED_EDGE ( 'NONE', *, *, #17476, .T. ) ;
#13958 = CARTESIAN_POINT ( 'NONE',  ( -10.50000000000003375, 8.875661936878628921, -18.94832733001756253 ) ) ;
#13959 = VECTOR ( 'NONE', #1005, 1000.000000000000000 ) ;
#13960 = VERTEX_POINT ( 'NONE', #3067 ) ;
#13961 = B_SPLINE_CURVE_WITH_KNOTS ( 'NONE', 3,
 ( #47634, #15619, #35401, #4332 ),
 .UNSPECIFIED., .F., .F.,
 ( 4, 4 ),
 ( 1.470203731559684877E-17, 0.0004072981213151955220 ),
 .UNSPECIFIED. ) ;
#13962 = DIRECTION ( 'NONE',  ( -0.000000000000000000, -0.000000000000000000, -1.000000000000000000 ) ) ;
#13963 =( NAMED_UNIT ( * ) PLANE_ANGLE_UNIT ( ) SI_UNIT ( $, .RADIAN. ) );
#13964 = ORIENTED_EDGE ( 'NONE', *, *, #31285, .T. ) ;
#13965 = FACE_OUTER_BOUND ( 'NONE', #24128, .T. ) ;
#13966 = CARTESIAN_POINT ( 'NONE',  ( 113.3040265531850537, -1.749999999999997335, 120.8182875569279702 ) ) ;
#13967 = CARTESIAN_POINT ( 'NONE',  ( -0.9870575514055066613, -1.980598328282574316, 9.881002359080278907 ) ) ;
#13968 = CARTESIAN_POINT ( 'NONE',  ( 339.9999999999998863, -164.9999999999999432, 355.9999999999997726 ) ) ;
#13969 = DIRECTION ( 'NONE',  ( 1.000000000000000000, 0.000000000000000000, 0.000000000000000000 ) ) ;
#13970 = VERTEX_POINT ( 'NONE', #10771 ) ;
#13971 = ADVANCED_FACE ( 'NONE', ( #45644 ), #14374, .F. ) ;
#13972 = CARTESIAN_POINT ( 'NONE',  ( -208.4459734468149463, 0.000000000000000000, -80.93171244307201562 ) ) ;
#13973 = CARTESIAN_POINT ( 'NONE',  ( 155.0540265531850537, -1.025126265847089435, 162.5682875569279133 ) ) ;
#13974 = CARTESIAN_POINT ( 'NONE',  ( -164.9459734468149463, -1.025126265847089435, 122.5682875569280128 ) ) ;
#13975 = FACE_OUTER_BOUND ( 'NONE', #44771, .T. ) ;
#13976 = LINE ( 'NONE', #33005, #23191 ) ;
#13977 = FACE_OUTER_BOUND ( 'NONE', #8044, .T. ) ;
#13978 = EDGE_CURVE ( 'NONE', #47711, #25776, #4910, .T. ) ;
#13979 = DIRECTION ( 'NONE',  ( 0.000000000000000000, 2.537652627714642000E-15, 1.000000000000000000 ) ) ;
#13980 = CARTESIAN_POINT ( 'NONE',  ( 210.0000000000000568, 0.000000000000000000, 2.568287556927987048 ) ) ;
#13981 = CARTESIAN_POINT ( 'NONE',  ( 30.00000000000187228, 16.00000000000000000, 65.00000000000000000 ) ) ;
#13982 = AXIS2_PLACEMENT_3D ( 'NONE', #2705, #30162, #11183 ) ;
#13983 = VERTEX_POINT ( 'NONE', #18469 ) ;
#13984 = DIRECTION ( 'NONE',  ( -0.000000000000000000, -1.000000000000000000, -0.000000000000000000 ) ) ;
#13985 = EDGE_CURVE ( 'NONE', #29337, #39755, #22319, .T. ) ;
#13986 = VECTOR ( 'NONE', #19808, 1000.000000000000000 ) ;
#13987 = EDGE_CURVE ( 'NONE', #30057, #39651, #29775, .T. ) ;
#13988 = DIRECTION ( 'NONE',  ( 0.000000000000000000, -0.000000000000000000, 1.000000000000000000 ) ) ;
#13989 = CARTESIAN_POINT ( 'NONE',  ( 1.011271242968688311, -0.7347315653655855927, 10.00000000000000000 ) ) ;
#13990 = DIRECTION ( 'NONE',  ( 0.000000000000000000, 5.664403186863042467E-17, 1.000000000000000000 ) ) ;
#13991 = DIRECTION ( 'NONE',  ( -1.000000000000000000, -0.000000000000000000, -0.000000000000000000 ) ) ;
#13992 = EDGE_CURVE ( 'NONE', #15814, #18475, #38525, .T. ) ;
#13993 = ORIENTED_EDGE ( 'NONE', *, *, #38119, .F. ) ;
#13994 = VECTOR ( 'NONE', #16333, 1000.000000000000000 ) ;
#13995 = ORIENTED_EDGE ( 'NONE', *, *, #35555, .F. ) ;
#13996 = FACE_OUTER_BOUND ( 'NONE', #10047, .T. ) ;
#13997 = EDGE_CURVE ( 'NONE', #35640, #30619, #47478, .T. ) ;
#13998 = CARTESIAN_POINT ( 'NONE',  ( 75.05402655318509630, 1.025126265847089435, 39.06828755692797728 ) ) ;
#13999 = ORIENTED_EDGE ( 'NONE', *, *, #11102, .T. ) ;
#14000 = CARTESIAN_POINT ( 'NONE',  ( 6.875132362119187768, -50.00000000000000711, 8.356839323120299312 ) ) ;
#14001 = ORIENTED_EDGE ( 'NONE', *, *, #8762, .F. ) ;
#14002 = VERTEX_POINT ( 'NONE', #42068 ) ;
#14003 = ORIENTED_EDGE ( 'NONE', *, *, #31058, .T. ) ;
#14004 = ADVANCED_FACE ( 'NONE', ( #25422 ), #12884, .T. ) ;
#14005 = DIRECTION ( 'NONE',  ( -0.000000000000000000, -0.000000000000000000, 1.000000000000000000 ) ) ;
#14006 = CARTESIAN_POINT ( 'NONE',  ( 49.67735855322978011, -8.912210285361751971, 8.356839323120299312 ) ) ;
#14007 = PLANE ( 'NONE',  #38219 ) ;
#14008 =( BOUNDED_CURVE ( )  B_SPLINE_CURVE ( 3, ( #26454, #26716, #22606, #22098 ),
 .UNSPECIFIED., .F., .F. ) 
 B_SPLINE_CURVE_WITH_KNOTS ( ( 4, 4 ),
 ( 0.000000000000000000, 1.570796326794896558 ),
 .UNSPECIFIED. ) 
 CURVE ( )  GEOMETRIC_REPRESENTATION_ITEM ( )  RATIONAL_B_SPLINE_CURVE ( ( 1.000000000000000000, 0.8047378541243649375, 0.8047378541243649375, 1.000000000000000000 ) ) 
 REPRESENTATION_ITEM ( '' )  );
#14009 = ORIENTED_EDGE ( 'NONE', *, *, #38401, .T. ) ;
#14010 = CARTESIAN_POINT ( 'NONE',  ( -168.4459734468149463, 0.000000000000000000, -37.43171244307205825 ) ) ;
#14011 = EDGE_CURVE ( 'NONE', #45021, #36600, #41324, .T. ) ;
#14012 = CARTESIAN_POINT ( 'NONE',  ( -120.0000000000000426, 17.00000000000000000, -114.9999999999999858 ) ) ;
#14013 = DIRECTION ( 'NONE',  ( 3.172065745548403743E-16, 1.000000000000000000, 0.000000000000000000 ) ) ;
#14014 = ORIENTED_EDGE ( 'NONE', *, *, #36688, .T. ) ;
#14015 = VERTEX_POINT ( 'NONE', #37501 ) ;
#14016 = LINE ( 'NONE', #21978, #4919 ) ;
#14018 = CARTESIAN_POINT ( 'NONE',  ( -17.23491422248386584, 0.5912720620001978844, 8.727788335465566760 ) ) ;
#14017 =( BOUNDED_CURVE ( )  B_SPLINE_CURVE ( 3, ( #27904, #39959, #27649, #46843 ),
 .UNSPECIFIED., .F., .F. ) 
 B_SPLINE_CURVE_WITH_KNOTS ( ( 4, 4 ),
 ( 3.141592653589793116, 4.712388980384689674 ),
 .UNSPECIFIED. ) 
 CURVE ( )  GEOMETRIC_REPRESENTATION_ITEM ( )  RATIONAL_B_SPLINE_CURVE ( ( 1.000000000000000000, 0.8047378541243649375, 0.8047378541243649375, 1.000000000000000000 ) ) 
 REPRESENTATION_ITEM ( '' )  );
#14019 = LINE ( 'NONE', #18126, #46159 ) ;
#14020 = ORIENTED_EDGE ( 'NONE', *, *, #20481, .F. ) ;
#14021 = AXIS2_PLACEMENT_3D ( 'NONE', #34738, #46222, #3399 ) ;
#14022 = DIRECTION ( 'NONE',  ( -0.000000000000000000, -0.000000000000000000, -1.000000000000000000 ) ) ;
#14023 = DIRECTION ( 'NONE',  ( 2.958228394578793832E-31, 0.000000000000000000, 1.000000000000000000 ) ) ;
#14024 = CARTESIAN_POINT ( 'NONE',  ( -46.69597344681494633, -1.750000000000009992, -159.1817124430720298 ) ) ;
#14025 = LINE ( 'NONE', #41741, #30654 ) ;
#14026 = CARTESIAN_POINT ( 'NONE',  ( 21.58778298521313843, -25.34222074689757065, 3.199614146704519602 ) ) ;
#14027 = AXIS2_PLACEMENT_3D ( 'NONE', #32240, #1197, #16078 ) ;
#14028 = DIRECTION ( 'NONE',  ( 6.203854594147707562E-25, -2.067951531382569187E-25, 1.000000000000000000 ) ) ;
#14029 = CARTESIAN_POINT ( 'NONE',  ( 432.7825420346616170, 67.47808924524053964, -120.5992382549688955 ) ) ;
#14030 =( BOUNDED_CURVE ( )  B_SPLINE_CURVE ( 3, ( #20652, #19887, #15790, #8103 ),
 .UNSPECIFIED., .F., .F. ) 
 B_SPLINE_CURVE_WITH_KNOTS ( ( 4, 4 ),
 ( 3.141592653589793116, 4.712388980384689674 ),
 .UNSPECIFIED. ) 
 CURVE ( )  GEOMETRIC_REPRESENTATION_ITEM ( )  RATIONAL_B_SPLINE_CURVE ( ( 1.000000000000000000, 0.8047378541243649375, 0.8047378541243649375, 1.000000000000000000 ) ) 
 REPRESENTATION_ITEM ( '' )  );
#14031 = AXIS2_PLACEMENT_3D ( 'NONE', #50552, #26997, #38574 ) ;
#14032 = CARTESIAN_POINT ( 'NONE',  ( -168.4459734468149747, 1.025126265847089213, -0.9317124430720324924 ) ) ;
#14033 = DIRECTION ( 'NONE',  ( 1.000000000000000000, 0.000000000000000000, 0.000000000000000000 ) ) ;
#14034 = FACE_OUTER_BOUND ( 'NONE', #34092, .T. ) ;
#14035 = ORIENTED_EDGE ( 'NONE', *, *, #9205, .T. ) ;
#14036 = CARTESIAN_POINT ( 'NONE',  ( 80.00000000000186162, 17.00000000000000000, 65.00000000000000000 ) ) ;
#14037 = CARTESIAN_POINT ( 'NONE',  ( -5.000000000000000000, 165.2000000000000171, -340.2000000000001592 ) ) ;
#14038 = CARTESIAN_POINT ( 'NONE',  ( 4.999999999999999112, -175.0000000000000284, -346.2500000000002274 ) ) ;
#14039 = ORIENTED_EDGE ( 'NONE', *, *, #13416, .T. ) ;
#14040 = CARTESIAN_POINT ( 'NONE',  ( 32.27890028733795447, 1.750000000000010436, -80.20683870891910772 ) ) ;
#14041 = ADVANCED_FACE ( 'NONE', ( #33636 ), #45393, .T. ) ;
#14042 = EDGE_CURVE ( 'NONE', #46181, #23633, #50221, .T. ) ;
#14043 = CARTESIAN_POINT ( 'NONE',  ( -48.44597344681492501, 0.000000000000000000, 162.5682875569279702 ) ) ;
#14044 = ORIENTED_EDGE ( 'NONE', *, *, #20681, .T. ) ;
#14045 = CARTESIAN_POINT ( 'NONE',  ( -46.69597344681494633, -1.750000000000010214, 40.81828755692798438 ) ) ;
#14046 = CARTESIAN_POINT ( 'NONE',  ( 113.3040265531850537, 0.000000000000000000, 165.0000000000000000 ) ) ;
#14047 = CARTESIAN_POINT ( 'NONE',  ( 73.30402655318508209, 0.000000000000000000, 165.0000000000000000 ) ) ;
#14048 = CYLINDRICAL_SURFACE ( 'NONE', #25006, 1.749999999999973799 ) ;
#14049 = AXIS2_PLACEMENT_3D ( 'NONE', #34753, #50321, #31143 ) ;
#14050 = VECTOR ( 'NONE', #23242, 1000.000000000000114 ) ;
#14051 = EDGE_CURVE ( 'NONE', #11765, #27818, #39257, .T. ) ;
#14052 = ORIENTED_EDGE ( 'NONE', *, *, #8629, .T. ) ;
#14053 = CYLINDRICAL_SURFACE ( 'NONE', #29014, 4.000000000000003553 ) ;
#14054 = VERTEX_POINT ( 'NONE', #15395 ) ;
#14055 = ORIENTED_EDGE ( 'NONE', *, *, #8275, .T. ) ;
#14056 = EDGE_CURVE ( 'NONE', #42074, #33060, #43331, .T. ) ;
#14057 = FACE_OUTER_BOUND ( 'NONE', #20290, .T. ) ;
#14058 = EDGE_CURVE ( 'NONE', #27139, #46544, #46648, .T. ) ;
#14059 = ORIENTED_EDGE ( 'NONE', *, *, #5640, .T. ) ;
#14060 = VECTOR ( 'NONE', #12590, 1000.000000000000000 ) ;
#14061 = DIRECTION ( 'NONE',  ( 0.000000000000000000, 0.000000000000000000, 1.000000000000000000 ) ) ;
#14062 = DIRECTION ( 'NONE',  ( 0.000000000000000000, 0.000000000000000000, 1.000000000000000000 ) ) ;
#14063 = ORIENTED_EDGE ( 'NONE', *, *, #26843, .T. ) ;
#14064 = CARTESIAN_POINT ( 'NONE',  ( 155.0540265531850537, -1.025126265847089657, 79.06828755692797017 ) ) ;
#14065 = EDGE_CURVE ( 'NONE', #10600, #17731, #39513, .T. ) ;
#14066 = FACE_OUTER_BOUND ( 'NONE', #35807, .T. ) ;
#14067 = EDGE_CURVE ( 'NONE', #10796, #3283, #34909, .T. ) ;
#14068 = VECTOR ( 'NONE', #31757, 1000.000000000000000 ) ;
#14069 = CARTESIAN_POINT ( 'NONE',  ( 342.8284271247460993, 167.0000000000000284, -342.0000000000001705 ) ) ;
#14070 = ORIENTED_EDGE ( 'NONE', *, *, #32846, .T. ) ;
#14071 = DIRECTION ( 'NONE',  ( -0.000000000000000000, -1.000000000000000000, -0.000000000000000000 ) ) ;
#14072 = DIRECTION ( 'NONE',  ( -1.368455531567204171E-48, 1.000000000000000000, 2.265761274745217480E-16 ) ) ;
#14073 = LINE ( 'NONE', #49931, #32459 ) ;
#14074 = ORIENTED_EDGE ( 'NONE', *, *, #5253, .F. ) ;
#14075 = DIRECTION ( 'NONE',  ( -1.612977847700450206E-50, 0.000000000000000000, -1.000000000000000000 ) ) ;
#14076 = CARTESIAN_POINT ( 'NONE',  ( 85.00000000000029843, 17.00000000000000000, -60.00000000000000000 ) ) ;
#14077 = VERTEX_POINT ( 'NONE', #7188 ) ;
#14078 = ORIENTED_EDGE ( 'NONE', *, *, #39809, .F. ) ;
#14079 = EDGE_LOOP ( 'NONE', ( #3321, #31110 ) ) ;
#14080 = CARTESIAN_POINT ( 'NONE',  ( -0.8155877869437639927, -0.9072449372115535260, 9.963925895596188909 ) ) ;
#14081 = CARTESIAN_POINT ( 'NONE',  ( -7.200076171898729172, 0.000000000000000000, 33.33601305720110020 ) ) ;
#14082 = ORIENTED_EDGE ( 'NONE', *, *, #32411, .F. ) ;
#14083 = CARTESIAN_POINT ( 'NONE',  ( -8.277096487746778308, 33.14818118907697198, 7.455576670931136185 ) ) ;
#14084 = LINE ( 'NONE', #28746, #34460 ) ;
#14085 = FACE_BOUND ( 'NONE', #37139, .T. ) ;
#14086 = PLANE ( 'NONE',  #45624 ) ;
#14087 = ORIENTED_EDGE ( 'NONE', *, *, #47491, .F. ) ;
#14088 = FACE_OUTER_BOUND ( 'NONE', #28870, .T. ) ;
#14089 = CARTESIAN_POINT ( 'NONE',  ( 152.2789002873379900, -1.750000000000010214, -80.20683870891910772 ) ) ;
#14090 = AXIS2_PLACEMENT_3D ( 'NONE', #4385, #20026, #28493 ) ;
#14091 = DIRECTION ( 'NONE',  ( -1.000000000000000000, -0.000000000000000000, -0.000000000000000000 ) ) ;
#14093 = ADVANCED_FACE ( 'NONE', ( #7956 ), #31312, .T. ) ;
#14092 = VECTOR ( 'NONE', #38564, 1000.000000000000000 ) ;
#14094 = ORIENTED_EDGE ( 'NONE', *, *, #27370, .T. ) ;
#14095 = LINE ( 'NONE', #10754, #27371 ) ;
#14096 = CARTESIAN_POINT ( 'NONE',  ( -1.238491169206289877, -5.772936915099371014, 9.586754400234154261 ) ) ;
#14097 = VECTOR ( 'NONE', #23741, 1000.000000000000000 ) ;
#14098 = LINE ( 'NONE', #41310, #26519 ) ;
#14099 = LINE ( 'NONE', #36993, #24049 ) ;
#14100 = VERTEX_POINT ( 'NONE', #23854 ) ;
#14101 = CARTESIAN_POINT ( 'NONE',  ( 73.30402655318508209, 0.000000000000000000, 165.0000000000000000 ) ) ;
#14102 = CARTESIAN_POINT ( 'NONE',  ( -9.999999999999998224, 8.486842105263161073, -18.34680996553531784 ) ) ;
#14103 = DIRECTION ( 'NONE',  ( 0.000000000000000000, -1.000000000000000000, 0.000000000000000000 ) ) ;
#14104 = CARTESIAN_POINT ( 'NONE',  ( 210.0000000000000568, 0.000000000000000000, 120.8182875569279702 ) ) ;
#14105 = CARTESIAN_POINT ( 'NONE',  ( -165.0000000000000284, 16.00000000000000000, 65.00000000000000000 ) ) ;
#14106 = EDGE_LOOP ( 'NONE', ( #19858, #28986, #37562, #9621, #1656, #38329 ) ) ;
#14107 = CARTESIAN_POINT ( 'NONE',  ( 210.0000000000000568, 0.000000000000000000, -77.43171244307200141 ) ) ;
#14108 = VERTEX_POINT ( 'NONE', #4099 ) ;
#14109 = DIRECTION ( 'NONE',  ( 0.000000000000000000, 0.000000000000000000, 1.000000000000000000 ) ) ;
#14110 = EDGE_LOOP ( 'NONE', ( #30884, #47950, #2278, #26267 ) ) ;
#14111 = CARTESIAN_POINT ( 'NONE',  ( 210.0000000000000568, 0.000000000000000000, 162.5682875569279702 ) ) ;
#14112 = CARTESIAN_POINT ( 'NONE',  ( 1.104213410210670876, 0.6509177773818231039, 9.976582533991679824 ) ) ;
#14113 = AXIS2_PLACEMENT_3D ( 'NONE', #28098, #39916, #650 ) ;
#14114 = CARTESIAN_POINT ( 'NONE',  ( -4.945973446814916130, 1.025126265847097429, -80.93171244307204404 ) ) ;
#14115 = ORIENTED_EDGE ( 'NONE', *, *, #29082, .F. ) ;
#14116 = DIRECTION ( 'NONE',  ( -0.000000000000000000, -0.000000000000000000, -1.000000000000000000 ) ) ;
#14117 = ORIENTED_EDGE ( 'NONE', *, *, #42448, .T. ) ;
#14118 = LINE ( 'NONE', #22083, #13908 ) ;
#14119 = CARTESIAN_POINT ( 'NONE',  ( 2.277991179055260051, -9.750753554112558064, 3.092310436554651432 ) ) ;
#14120 = VECTOR ( 'NONE', #29192, 1000.000000000000000 ) ;
#14121 = CARTESIAN_POINT ( 'NONE',  ( -11.73320209285699889, 11.96063479729179768, 9.403735324607438884 ) ) ;
#14122 = DIRECTION ( 'NONE',  ( -0.000000000000000000, -0.000000000000000000, -1.000000000000000000 ) ) ;
#14123 = EDGE_CURVE ( 'NONE', #12977, #21718, #14765, .T. ) ;
#14124 = AXIS2_PLACEMENT_3D ( 'NONE', #46177, #6711, #14414 ) ;
#14125 = CARTESIAN_POINT ( 'NONE',  ( 210.0000000000000568, 2.143131898507881116E-16, -40.93171244307203693 ) ) ;
#14126 = VERTEX_POINT ( 'NONE', #27699 ) ;
#14127 = ORIENTED_EDGE ( 'NONE', *, *, #46529, .T. ) ;
#14128 = DIRECTION ( 'NONE',  ( 0.000000000000000000, 0.000000000000000000, 1.000000000000000000 ) ) ;
#14129 = ORIENTED_EDGE ( 'NONE', *, *, #8052, .F. ) ;
#14130 = VECTOR ( 'NONE', #41876, 1000.000000000000000 ) ;
#14131 = CARTESIAN_POINT ( 'NONE',  ( 80.00000000000217426, 17.00000000000000000, 115.0000000000000142 ) ) ;
#14132 = DIRECTION ( 'NONE',  ( 0.000000000000000000, 0.000000000000000000, 1.000000000000000000 ) ) ;
#14133 = EDGE_LOOP ( 'NONE', ( #19381, #6002, #40223, #11287 ) ) ;
#14134 = CARTESIAN_POINT ( 'NONE',  ( -1.080000014127418639, -0.7606467978654640749, 9.943883492372872723 ) ) ;
#14135 = DIRECTION ( 'NONE',  ( 1.000000000000000000, -0.000000000000000000, -0.000000000000000000 ) ) ;
#14136 = ORIENTED_EDGE ( 'NONE', *, *, #36268, .F. ) ;
#14137 = CARTESIAN_POINT ( 'NONE',  ( -36.08557433729204433, 35.58569447144795106, 7.455576670931136185 ) ) ;
#14138 = CARTESIAN_POINT ( 'NONE',  ( 181.0000000000000000, -97.49999999999998579, -350.0000000000001705 ) ) ;
#14139 = CARTESIAN_POINT ( 'NONE',  ( 32.27890028733795447, 1.750000000000009548, -118.1565861772249519 ) ) ;
#14140 = CARTESIAN_POINT ( 'NONE',  ( -31.46770792452106846, 38.94077080897363885, 3.199614146704519602 ) ) ;
#14141 = ORIENTED_EDGE ( 'NONE', *, *, #38548, .T. ) ;
#14142 = VERTEX_POINT ( 'NONE', #50488 ) ;
#14143 = DIRECTION ( 'NONE',  ( -1.000000000000000000, -0.000000000000000000, -0.000000000000000000 ) ) ;
#14144 = FACE_OUTER_BOUND ( 'NONE', #38958, .T. ) ;
#14145 = CARTESIAN_POINT ( 'NONE',  ( 210.0000000000000568, 0.000000000000000000, -77.43171244307200141 ) ) ;
#14146 = AXIS2_PLACEMENT_3D ( 'NONE', #1598, #40836, #17246 ) ;
#14147 = FACE_OUTER_BOUND ( 'NONE', #2386, .T. ) ;
#14148 = ORIENTED_EDGE ( 'NONE', *, *, #9050, .F. ) ;
#14149 = LINE ( 'NONE', #17513, #19253 ) ;
#14150 = ADVANCED_FACE ( 'NONE', ( #31050 ), #48080, .T. ) ;
#14151 = EDGE_LOOP ( 'NONE', ( #46547, #5274, #31066, #22344, #4899 ) ) ;
#14152 = CARTESIAN_POINT ( 'NONE',  ( 339.9999999999999432, 185.0000000000000284, -356.0000000000001705 ) ) ;
#14153 = LINE ( 'NONE', #25217, #14583 ) ;
#14154 = CARTESIAN_POINT ( 'NONE',  ( -5.888214538810513154, -16.20866436362413410, 8.727788335465566760 ) ) ;
#14155 = CARTESIAN_POINT ( 'NONE',  ( -1.270843316669170608, 0.6654759734677931915, 9.950105812514292936 ) ) ;
#14156 = CARTESIAN_POINT ( 'NONE',  ( 0.6215990105956902267, -1.608617984725389860, 9.928159647716132241 ) ) ;
#14157 = CARTESIAN_POINT ( 'NONE',  ( 31.55402655318503236, 0.000000000000000000, 82.56828755692798438 ) ) ;
#14158 = ORIENTED_EDGE ( 'NONE', *, *, #2018, .F. ) ;
#14159 = CARTESIAN_POINT ( 'NONE',  ( -6.695973446814940111, -1.750000000000023759, 40.81828755692798438 ) ) ;
#14160 = VECTOR ( 'NONE', #38671, 1000.000000000000000 ) ;
#14161 = CARTESIAN_POINT ( 'NONE',  ( -164.9999999999997442, 17.00000000000000000, -84.99999999999998579 ) ) ;
#14162 = CARTESIAN_POINT ( 'NONE',  ( 164.9999999999999716, -272.4999999999999432, -355.9999999999999432 ) ) ;
#14163 = VECTOR ( 'NONE', #15580, 1000.000000000000000 ) ;
#14164 = CARTESIAN_POINT ( 'NONE',  ( -88.44597344681497475, 0.000000000000000000, 42.56828755692799859 ) ) ;
#14165 = ORIENTED_EDGE ( 'NONE', *, *, #42796, .F. ) ;
#14166 = CARTESIAN_POINT ( 'NONE',  ( -46.69597344681494633, 0.000000000000000000, 165.0000000000000000 ) ) ;
#14167 = ORIENTED_EDGE ( 'NONE', *, *, #23969, .T. ) ;
#14168 = CARTESIAN_POINT ( 'NONE',  ( 111.5540265531850679, 0.000000000000000000, 165.0000000000000000 ) ) ;
#14169 = CARTESIAN_POINT ( 'NONE',  ( 1.468446590252912465, 0.3226319952343980058, 9.953784399990622589 ) ) ;
#14170 =( BOUNDED_CURVE ( )  B_SPLINE_CURVE ( 3, ( #30089, #9810, #34198, #22369 ),
 .UNSPECIFIED., .F., .F. ) 
 B_SPLINE_CURVE_WITH_KNOTS ( ( 4, 4 ),
 ( 1.570796326794883013, 3.141592653589793560 ),
 .UNSPECIFIED. ) 
 CURVE ( )  GEOMETRIC_REPRESENTATION_ITEM ( )  RATIONAL_B_SPLINE_CURVE ( ( 1.000000000000000000, 0.8047378541243617178, 0.8047378541243617178, 1.000000000000000000 ) ) 
 REPRESENTATION_ITEM ( '' )  );
#14172 = DIRECTION ( 'NONE',  ( -1.000000000000000000, 0.000000000000000000, 0.000000000000000000 ) ) ;
#14171 = B_SPLINE_CURVE_WITH_KNOTS ( 'NONE', 3,
 ( #5855, #48651, #33072, #18402 ),
 .UNSPECIFIED., .F., .F.,
 ( 4, 4 ),
 ( 8.673617379884035472E-19, 0.002466147708923230146 ),
 .UNSPECIFIED. ) ;
#14173 = ORIENTED_EDGE ( 'NONE', *, *, #24434, .F. ) ;
#14174 = CARTESIAN_POINT ( 'NONE',  ( 0.3862712429686727678, 1.188820645368945605, -10.00000000000000000 ) ) ;
#14175 = VERTEX_POINT ( 'NONE', #46132 ) ;
#14176 = DIRECTION ( 'NONE',  ( 0.000000000000000000, -0.000000000000000000, 1.000000000000000000 ) ) ;
#14177 = DIRECTION ( 'NONE',  ( -0.000000000000000000, -1.000000000000000000, -0.000000000000000000 ) ) ;
#14178 = CARTESIAN_POINT ( 'NONE',  ( 49.89397392339123627, -8.245536726716670373, 7.906207997025717304 ) ) ;
#14179 = EDGE_CURVE ( 'NONE', #47386, #26837, #48744, .T. ) ;
#14180 = ORIENTED_EDGE ( 'NONE', *, *, #745, .T. ) ;
#14181 = EDGE_LOOP ( 'NONE', ( #33244, #5405, #47307, #512, #34428, #45728, #10469, #38789, #3474, #35448, #26654, #41206, #47094, #26944, #40847, #2976, #32472, #4493, #1038, #17660, #1776, #38624, #42273, #2390, #37908, #21573, #22614, #46661 ) ) ;
#14182 = CARTESIAN_POINT ( 'NONE',  ( -207.7210997126620384, -1.750000000000009548, 161.8434138227750907 ) ) ;
#14183 = EDGE_CURVE ( 'NONE', #14529, #46434, #42823, .T. ) ;
#14184 = CARTESIAN_POINT ( 'NONE',  ( 85.00000000000029843, 16.00000000000000000, -60.00000000000000000 ) ) ;
#14185 = ADVANCED_FACE ( 'NONE', ( #263 ), #15641, .T. ) ;
#14186 = ORIENTED_EDGE ( 'NONE', *, *, #23501, .F. ) ;
#14187 = ORIENTED_EDGE ( 'NONE', *, *, #6824, .F. ) ;
#14188 = LINE ( 'NONE', #22657, #38065 ) ;
#14189 = PLANE ( 'NONE',  #41471 ) ;
#14190 = VECTOR ( 'NONE', #23423, 1000.000000000000000 ) ;
#14191 = FACE_OUTER_BOUND ( 'NONE', #24833, .T. ) ;
#14192 = ORIENTED_EDGE ( 'NONE', *, *, #10378, .F. ) ;
#14193 = CARTESIAN_POINT ( 'NONE',  ( 114.3291528190321173, -1.749999999999996225, -158.1565861772249377 ) ) ;
#14194 = AXIS2_PLACEMENT_3D ( 'NONE', #32735, #16833, #5781 ) ;
#14195 = VERTEX_POINT ( 'NONE', #38507 ) ;
#14196 = EDGE_CURVE ( 'NONE', #4014, #17305, #28951, .T. ) ;
#14197 = ADVANCED_FACE ( 'NONE', ( #44082 ), #36690, .F. ) ;
#14198 = CIRCLE ( 'NONE', #46141, 2.000000000000001776 ) ;
#14199 = CARTESIAN_POINT ( 'NONE',  ( -6.695973446814940111, -1.750000000000023759, -39.18171244307202983 ) ) ;
#14200 = EDGE_CURVE ( 'NONE', #8390, #15732, #3210, .T. ) ;
#14201 = FACE_BOUND ( 'NONE', #9058, .T. ) ;
#14202 = VECTOR ( 'NONE', #28827, 1000.000000000000000 ) ;
#14203 = ORIENTED_EDGE ( 'NONE', *, *, #44353, .F. ) ;
#14204 = ORIENTED_EDGE ( 'NONE', *, *, #38083, .T. ) ;
#14205 = LINE ( 'NONE', #29873, #30606 ) ;
#14206 = ORIENTED_EDGE ( 'NONE', *, *, #23297, .F. ) ;
#14207 = DIRECTION ( 'NONE',  ( 6.203854594147707562E-25, -2.067951531382569187E-25, 1.000000000000000000 ) ) ;
#14208 = EDGE_CURVE ( 'NONE', #25022, #44965, #1514, .T. ) ;
#14209 = ADVANCED_FACE ( 'NONE', ( #31815 ), #25113, .F. ) ;
#14210 = EDGE_LOOP ( 'NONE', ( #33498, #358, #9588, #8683, #46131 ) ) ;
#14211 = CARTESIAN_POINT ( 'NONE',  ( 355.9999999999999432, 185.0000000000002274, -360.0000000000003411 ) ) ;
#14212 = CARTESIAN_POINT ( 'NONE',  ( -8.445973446814976526, 0.000000000000000000, -157.4317124430720014 ) ) ;
#14213 = VERTEX_POINT ( 'NONE', #24611 ) ;
#14214 = CARTESIAN_POINT ( 'NONE',  ( 168.9999999999999716, -97.49999999999997158, -115.0000000000001563 ) ) ;
#14215 = EDGE_CURVE ( 'NONE', #936, #45355, #24232, .T. ) ;
#14216 = FACE_OUTER_BOUND ( 'NONE', #29720, .T. ) ;
#14217 = PLANE ( 'NONE',  #38345 ) ;
#14218 = DIRECTION ( 'NONE',  ( 0.000000000000000000, 0.000000000000000000, 1.000000000000000000 ) ) ;
#14219 = EDGE_CURVE ( 'NONE', #3380, #12550, #38052, .T. ) ;
#14220 = VECTOR ( 'NONE', #7035, 1000.000000000000000 ) ;
#14221 = DIRECTION ( 'NONE',  ( 1.000000000000000000, 0.000000000000000000, -4.625929269271542120E-16 ) ) ;
#14222 = ORIENTED_EDGE ( 'NONE', *, *, #6089, .F. ) ;
#14223 = CARTESIAN_POINT ( 'NONE',  ( -164.9459734468149463, 2.143131898507880377E-16, 82.56828755692798438 ) ) ;
#14224 = ADVANCED_FACE ( 'NONE', ( #9450 ), #32572, .F. ) ;
#14225 = CARTESIAN_POINT ( 'NONE',  ( 350.0000000000000000, 165.0000000000000000, -344.0000000000001705 ) ) ;
#14226 = CARTESIAN_POINT ( 'NONE',  ( -164.9459734468149463, 2.143131898507880377E-16, 122.5682875569279702 ) ) ;
#14227 = FACE_OUTER_BOUND ( 'NONE', #11477, .T. ) ;
#14228 = CYLINDRICAL_SURFACE ( 'NONE', #49368, 1.750000000000001554 ) ;
#14229 = CARTESIAN_POINT ( 'NONE',  ( -9.999999999999994671, -46.01315789473684248, -25.00000000000000000 ) ) ;
#14230 = AXIS2_PLACEMENT_3D ( 'NONE', #34924, #43102, #31830 ) ;
#14231 = CARTESIAN_POINT ( 'NONE',  ( 3.996390545799824334, -16.57371371864897469, 8.953103998512858652 ) ) ;
#14232 = VECTOR ( 'NONE', #40999, 1000.000000000000000 ) ;
#14233 = FACE_OUTER_BOUND ( 'NONE', #43673, .T. ) ;
#14234 = EDGE_CURVE ( 'NONE', #35315, #33292, #513, .T. ) ;
#14235 = CARTESIAN_POINT ( 'NONE',  ( -6.695973446814940111, -1.750000000000023759, -39.18171244307202983 ) ) ;
#14236 = VECTOR ( 'NONE', #5337, 1000.000000000000000 ) ;
#14237 = EDGE_LOOP ( 'NONE', ( #27382, #6260, #24483, #11746 ) ) ;
#14238 =( NAMED_UNIT ( * ) PLANE_ANGLE_UNIT ( ) SI_UNIT ( $, .RADIAN. ) );
#14239 = EDGE_CURVE ( 'NONE', #7572, #8778, #8459, .T. ) ;
#14240 = EDGE_CURVE ( 'NONE', #38712, #29224, #24856, .T. ) ;
#14241 = CARTESIAN_POINT ( 'NONE',  ( -29.61572577327014955, -16.11461842845715253, 8.807470649214879543 ) ) ;
#14242 = CARTESIAN_POINT ( 'NONE',  ( -13.35436367797847801, -31.26996044524040741, 7.906207997025717304 ) ) ;
#14243 = CARTESIAN_POINT ( 'NONE',  ( 340.0000000000000568, 165.0000000000000000, 349.9999999999998295 ) ) ;
#14244 = CARTESIAN_POINT ( 'NONE',  ( 37.19569680397832201, -4.820783179364443782, 8.100132398494510610 ) ) ;
#14245 = EDGE_CURVE ( 'NONE', #19216, #37443, #47651, .T. ) ;
#14246 = ORIENTED_EDGE ( 'NONE', *, *, #30501, .T. ) ;
#14247 = PRODUCT_DEFINITION_SHAPE ( 'NONE', 'NONE',  #842 ) ;
#14248 = ORIENTED_EDGE ( 'NONE', *, *, #35127, .T. ) ;
#14249 = DIRECTION ( 'NONE',  ( 0.4055129968046615185, -0.4055129968046615185, -0.8192181753629523833 ) ) ;
#14250 = ADVANCED_FACE ( 'NONE', ( #20495 ), #28207, .F. ) ;
#14251 = DIRECTION ( 'NONE',  ( -0.000000000000000000, -1.000000000000000000, 2.537652627714643577E-15 ) ) ;
#14252 = AXIS2_PLACEMENT_3D ( 'NONE', #22746, #25845, #10440 ) ;
#14253 = VERTEX_POINT ( 'NONE', #40014 ) ;
#14254 = CARTESIAN_POINT ( 'NONE',  ( -26.18032376592659105, 21.95228666728381128, 7.455576670931136185 ) ) ;
#14255 = CARTESIAN_POINT ( 'NONE',  ( 194.3291528190321742, 1.750000000000009548, -38.15658617722494483 ) ) ;
#14256 =( BOUNDED_CURVE ( )  B_SPLINE_CURVE ( 3, ( #41454, #17846, #10408, #25553 ),
 .UNSPECIFIED., .F., .F. ) 
 B_SPLINE_CURVE_WITH_KNOTS ( ( 4, 4 ),
 ( 3.141592653589793116, 4.712388980384689674 ),
 .UNSPECIFIED. ) 
 CURVE ( )  GEOMETRIC_REPRESENTATION_ITEM ( )  RATIONAL_B_SPLINE_CURVE ( ( 1.000000000000000000, 0.8047378541243649375, 0.8047378541243649375, 1.000000000000000000 ) ) 
 REPRESENTATION_ITEM ( '' )  );
#14257 = ORIENTED_EDGE ( 'NONE', *, *, #36242, .F. ) ;
#14258 = ORIENTED_EDGE ( 'NONE', *, *, #50091, .T. ) ;
#14259 = ORIENTED_EDGE ( 'NONE', *, *, #2988, .T. ) ;
#14260 = EDGE_CURVE ( 'NONE', #13781, #29572, #45028, .T. ) ;
#14261 = CARTESIAN_POINT ( 'NONE',  ( 164.9999999999999716, 17.00000000000000000, 90.00000000000000000 ) ) ;
#14262 = CARTESIAN_POINT ( 'NONE',  ( 33.86622497129647513, -3.037805405904928868, 7.906207997025717304 ) ) ;
#14263 = CARTESIAN_POINT ( 'NONE',  ( -1.011271242968693862, 0.7347315653655780432, 3.333333333333333481 ) ) ;
#14264 = ORIENTED_EDGE ( 'NONE', *, *, #9132, .T. ) ;
#14265 = CARTESIAN_POINT ( 'NONE',  ( 4.763548243873389154, -16.57409059453848599, 8.727788335465566760 ) ) ;
#14266 = FACE_OUTER_BOUND ( 'NONE', #23228, .T. ) ;
#14267 = DIRECTION ( 'NONE',  ( -1.000000000000000000, 0.000000000000000000, 0.000000000000000000 ) ) ;
#14268 = AXIS2_PLACEMENT_3D ( 'NONE', #21964, #6819, #34278 ) ;
#14269 = ORIENTED_EDGE ( 'NONE', *, *, #32772, .T. ) ;
#14270 = EDGE_CURVE ( 'NONE', #34291, #38172, #12802, .T. ) ;
#14271 = ORIENTED_EDGE ( 'NONE', *, *, #17043, .T. ) ;
#14272 = CARTESIAN_POINT ( 'NONE',  ( 113.3040265531850537, -1.749999999999997113, -39.18171244307202983 ) ) ;
#14273 = DIRECTION ( 'NONE',  ( 1.000000000000000000, 0.000000000000000000, 0.000000000000000000 ) ) ;
#14274 = ORIENTED_EDGE ( 'NONE', *, *, #36466, .T. ) ;
#14275 = VECTOR ( 'NONE', #42303, 1000.000000000000000 ) ;
#14276 = CARTESIAN_POINT ( 'NONE',  ( 210.0000000000000568, 2.143131898507880377E-16, -0.9317124430720331585 ) ) ;
#14277 = CARTESIAN_POINT ( 'NONE',  ( 355.9999999999999432, 174.9999999999996589, -356.0000000000003411 ) ) ;
#14278 = EDGE_CURVE ( 'NONE', #20660, #21333, #16915, .T. ) ;
#14279 = LINE ( 'NONE', #25590, #25995 ) ;
#14280 = LINE ( 'NONE', #38416, #36003 ) ;
#14281 = EDGE_CURVE ( 'NONE', #48113, #18968, #14171, .T. ) ;
#14282 = FACE_OUTER_BOUND ( 'NONE', #16402, .T. ) ;
#14283 = ORIENTED_EDGE ( 'NONE', *, *, #26962, .F. ) ;
#14284 = EDGE_CURVE ( 'NONE', #31660, #6290, #41756, .T. ) ;
#14285 = LINE ( 'NONE', #29951, #49575 ) ;
#14286 = EDGE_CURVE ( 'NONE', #2288, #3452, #33827, .T. ) ;
#14287 = DIRECTION ( 'NONE',  ( -0.000000000000000000, -0.000000000000000000, -1.000000000000000000 ) ) ;
#14288 = CARTESIAN_POINT ( 'NONE',  ( 185.0000000000000000, -272.5000000000000000, -104.9999999999999289 ) ) ;
#14289 = EDGE_CURVE ( 'NONE', #47880, #9147, #2509, .T. ) ;
#14290 = CARTESIAN_POINT ( 'NONE',  ( -3.231548175622898089, 9.463461120997347820, 9.282506307616472441 ) ) ;
#14291 = AXIS2_PLACEMENT_3D ( 'NONE', #37798, #49017, #49773 ) ;
#14292 = CARTESIAN_POINT ( 'NONE',  ( 135.0000000000003411, 17.00000000000000000, -84.99999999999998579 ) ) ;
#14293 = VECTOR ( 'NONE', #37610, 1000.000000000000000 ) ;
#14294 = VERTEX_POINT ( 'NONE', #9955 ) ;
#14295 = DIRECTION ( 'NONE',  ( -0.000000000000000000, -0.000000000000000000, -1.000000000000000000 ) ) ;
#14296 = DIRECTION ( 'NONE',  ( 0.000000000000000000, 1.000000000000000000, 0.000000000000000000 ) ) ;
#14297 = PLANE ( 'NONE',  #36152 ) ;
#14298 = ORIENTED_EDGE ( 'NONE', *, *, #92, .T. ) ;
#14299 = DIRECTION ( 'NONE',  ( -0.000000000000000000, -0.000000000000000000, -1.000000000000000000 ) ) ;
#14300 = EDGE_CURVE ( 'NONE', #20217, #43954, #34083, .T. ) ;
#14301 = CARTESIAN_POINT ( 'NONE',  ( -1.902009873419727048, -1.028513407865101037, 9.882710035074770971 ) ) ;
#14302 = VECTOR ( 'NONE', #18923, 1000.000000000000000 ) ;
#14303 = ORIENTED_EDGE ( 'NONE', *, *, #36176, .T. ) ;
#14304 = CARTESIAN_POINT ( 'NONE',  ( 164.9999999999999716, 16.00000000000000000, 115.0000000000000142 ) ) ;
#14305 = DIRECTION ( 'NONE',  ( 0.000000000000000000, 0.000000000000000000, -1.000000000000000000 ) ) ;
#14306 = DIRECTION ( 'NONE',  ( -1.000000000000000000, 0.000000000000000000, 0.000000000000000000 ) ) ;
#14307 = DIRECTION ( 'NONE',  ( 0.000000000000000000, -1.000000000000000000, 3.469446951953611033E-15 ) ) ;
#14308 = ORIENTED_EDGE ( 'NONE', *, *, #3320, .F. ) ;
#14309 = CARTESIAN_POINT ( 'NONE',  ( 30.00000000000123279, 17.00000000000000000, 30.00000000000000000 ) ) ;
#14310 = ORIENTED_EDGE ( 'NONE', *, *, #35069, .T. ) ;
#14311 = EDGE_LOOP ( 'NONE', ( #31858, #32717, #39437, #37216 ) ) ;
#14312 = VECTOR ( 'NONE', #24345, 1000.000000000000000 ) ;
#14313 = CARTESIAN_POINT ( 'NONE',  ( -88.44597344681497475, 0.000000000000000000, -37.43171244307200141 ) ) ;
#14314 =( BOUNDED_CURVE ( )  B_SPLINE_CURVE ( 3, ( #16534, #17030, #39632, #4471 ),
 .UNSPECIFIED., .F., .F. ) 
 B_SPLINE_CURVE_WITH_KNOTS ( ( 4, 4 ),
 ( 4.712388980384689674, 6.283185307179586232 ),
 .UNSPECIFIED. ) 
 CURVE ( )  GEOMETRIC_REPRESENTATION_ITEM ( )  RATIONAL_B_SPLINE_CURVE ( ( 1.000000000000000000, 0.8047378541243649375, 0.8047378541243649375, 1.000000000000000000 ) ) 
 REPRESENTATION_ITEM ( '' )  );
#14315 = B_SPLINE_CURVE_WITH_KNOTS ( 'NONE', 3,
 ( #478, #31275, #27162, #11762 ),
 .UNSPECIFIED., .F., .F.,
 ( 4, 4 ),
 ( 0.000000000000000000, 0.2562577668812818232 ),
 .UNSPECIFIED. ) ;
#14316 = VERTEX_POINT ( 'NONE', #49416 ) ;
#14317 = DIRECTION ( 'NONE',  ( 0.000000000000000000, 0.000000000000000000, 1.000000000000000000 ) ) ;
#14318 = FACE_OUTER_BOUND ( 'NONE', #50168, .T. ) ;
#14319 = FACE_OUTER_BOUND ( 'NONE', #6618, .T. ) ;
#14320 = ADVANCED_FACE ( 'NONE', ( #17891 ), #10706, .T. ) ;
#14321 = CARTESIAN_POINT ( 'NONE',  ( 75.05402655318509630, 2.143131898507880377E-16, -0.9317124430720524764 ) ) ;
#14322 =( BOUNDED_CURVE ( )  B_SPLINE_CURVE ( 3, ( #4343, #24103, #43320, #4595 ),
 .UNSPECIFIED., .F., .F. ) 
 B_SPLINE_CURVE_WITH_KNOTS ( ( 4, 4 ),
 ( 4.712388980384689674, 6.283185307179586232 ),
 .UNSPECIFIED. ) 
 CURVE ( )  GEOMETRIC_REPRESENTATION_ITEM ( )  RATIONAL_B_SPLINE_CURVE ( ( 1.000000000000000000, 0.8047378541243649375, 0.8047378541243649375, 1.000000000000000000 ) ) 
 REPRESENTATION_ITEM ( '' )  );
#14323 = LINE ( 'NONE', #3022, #39105 ) ;
#14324 = ORIENTED_EDGE ( 'NONE', *, *, #34401, .T. ) ;
#14325 = CARTESIAN_POINT ( 'NONE',  ( 11.73320209285708415, -11.96063479729170886, 9.403735324607438884 ) ) ;
#14326 = FACE_OUTER_BOUND ( 'NONE', #35509, .T. ) ;
#14327 = FACE_OUTER_BOUND ( 'NONE', #36724, .T. ) ;
#14328 = VECTOR ( 'NONE', #46526, 1000.000000000000000 ) ;
#14329 = ORIENTED_EDGE ( 'NONE', *, *, #7775, .T. ) ;
#14330 = LINE ( 'NONE', #26134, #41511 ) ;
#14331 = LINE ( 'NONE', #10488, #45761 ) ;
#14332 = ORIENTED_EDGE ( 'NONE', *, *, #46919, .T. ) ;
#14333 = VECTOR ( 'NONE', #28263, 1000.000000000000000 ) ;
#14334 = VERTEX_POINT ( 'NONE', #18148 ) ;
#14335 = ORIENTED_EDGE ( 'NONE', *, *, #2018, .T. ) ;
#14336 = CARTESIAN_POINT ( 'NONE',  ( -1.193089574352124149, -0.2545860991493743564, 9.963925895596188909 ) ) ;
#14337 = CARTESIAN_POINT ( 'NONE',  ( -164.9999999999994031, 16.00000000000000000, -30.00000000000000000 ) ) ;
#14338 = ORIENTED_EDGE ( 'NONE', *, *, #26656, .T. ) ;
#14339 = FACE_OUTER_BOUND ( 'NONE', #41399, .T. ) ;
#14340 = CARTESIAN_POINT ( 'NONE',  ( 33.30402655318503946, 1.750000000000009992, 160.8182875569279702 ) ) ;
#14341 = PLANE ( 'NONE',  #31336 ) ;
#14342 = VECTOR ( 'NONE', #43951, 1000.000000000000000 ) ;
#14343 = EDGE_CURVE ( 'NONE', #42084, #26282, #6867, .T. ) ;
#14344 = CARTESIAN_POINT ( 'NONE',  ( 115.0540265531850395, 2.143131898507847836E-16, 119.0682875569279844 ) ) ;
#14345 = EDGE_CURVE ( 'NONE', #6960, #6508, #10462, .T. ) ;
#14346 = EDGE_LOOP ( 'NONE', ( #31218, #14772, #24561, #22270, #46906, #10888 ) ) ;
#14347 = VECTOR ( 'NONE', #45786, 1000.000000000000000 ) ;
#14348 = CARTESIAN_POINT ( 'NONE',  ( 3.694521163055066282, 0.7694713829383740267, 9.865049507598753209 ) ) ;
#14349 = CARTESIAN_POINT ( 'NONE',  ( 34.38425513258721367, -36.82177522737821107, 8.807470649214879543 ) ) ;
#14350 = EDGE_CURVE ( 'NONE', #28031, #47828, #22932, .T. ) ;
#14351 = EDGE_CURVE ( 'NONE', #41656, #2158, #9266, .T. ) ;
#14352 = CARTESIAN_POINT ( 'NONE',  ( -15.73090589902298042, -29.60029367929041655, 1.847720168420772691 ) ) ;
#14353 = AXIS2_PLACEMENT_3D ( 'NONE', #46748, #38610, #2911 ) ;
#14354 = ORIENTED_EDGE ( 'NONE', *, *, #29081, .F. ) ;
#14355 = ADVANCED_FACE ( 'NONE', ( #29710 ), #25614, .T. ) ;
#14356 = CONTEXT_DEPENDENT_SHAPE_REPRESENTATION ( #44975, #11421 ) ;
#14357 = EDGE_CURVE ( 'NONE', #40535, #33858, #21758, .T. ) ;
#14358 = CARTESIAN_POINT ( 'NONE',  ( 71.55402655318505367, 0.000000000000000000, 165.0000000000000000 ) ) ;
#14359 = DIRECTION ( 'NONE',  ( 0.000000000000000000, 1.000000000000000000, -1.822804496942679766E-16 ) ) ;
#14360 = CARTESIAN_POINT ( 'NONE',  ( -1.011271242968683426, -0.7347315653655928092, -3.333333333333333481 ) ) ;
#14361 = CARTESIAN_POINT ( 'NONE',  ( -119.9999999999994174, 17.00000000000000000, -30.00000000000000000 ) ) ;
#14362 = VERTEX_POINT ( 'NONE', #14553 ) ;
#14363 = CARTESIAN_POINT ( 'NONE',  ( 350.0000000000000000, 169.0000000000000000, -342.0000000000001705 ) ) ;
#14364 = CARTESIAN_POINT ( 'NONE',  ( -32.57170742938676256, -18.58316106410400437, 7.697694107796192675 ) ) ;
#14365 = ADVANCED_FACE ( 'NONE', ( #37937 ), #29213, .F. ) ;
#14366 = PLANE ( 'NONE',  #22014 ) ;
#14367 = CARTESIAN_POINT ( 'NONE',  ( 183.0000000000000000, -272.5000000000000000, -98.99999999999944578 ) ) ;
#14368 = DIRECTION ( 'NONE',  ( -1.000000000000000000, 0.000000000000000000, 0.000000000000000000 ) ) ;
#14369 = B_SPLINE_CURVE_WITH_KNOTS ( 'NONE', 3,
 ( #3801, #12259, #20452, #46608 ),
 .UNSPECIFIED., .F., .F.,
 ( 4, 4 ),
 ( 0.003717760131171406711, 0.009855840391686850749 ),
 .UNSPECIFIED. ) ;
#14370 = ORIENTED_EDGE ( 'NONE', *, *, #9613, .T. ) ;
#14371 = VECTOR ( 'NONE', #13121, 1000.000000000000114 ) ;
#14372 = DIRECTION ( 'NONE',  ( -0.000000000000000000, -0.000000000000000000, -1.000000000000000000 ) ) ;
#14373 = VERTEX_POINT ( 'NONE', #2750 ) ;
#14374 = PLANE ( 'NONE',  #13037 ) ;
#14375 = AXIS2_PLACEMENT_3D ( 'NONE', #9696, #26364, #2999 ) ;
#14376 = ORIENTED_EDGE ( 'NONE', *, *, #35896, .T. ) ;
#14377 = CARTESIAN_POINT ( 'NONE',  ( 339.9999999999999432, -166.9999999999999432, -344.0000000000001705 ) ) ;
#14378 = DIRECTION ( 'NONE',  ( 0.000000000000000000, -1.000000000000000000, 0.000000000000000000 ) ) ;
#14379 = AXIS2_PLACEMENT_3D ( 'NONE', #5645, #28756, #21300 ) ;
#14380 = ORIENTED_EDGE ( 'NONE', *, *, #24389, .T. ) ;
#14381 = ORIENTED_EDGE ( 'NONE', *, *, #21460, .F. ) ;
#14382 = AXIS2_PLACEMENT_3D ( 'NONE', #12585, #35966, #809 ) ;
#14383 = DIRECTION ( 'NONE',  ( -1.445602896647339410E-16, -1.000000000000000000, -0.000000000000000000 ) ) ;
#14384 = ORIENTED_EDGE ( 'NONE', *, *, #16984, .T. ) ;
#14385 = CARTESIAN_POINT ( 'NONE',  ( -215.0000000000000568, 164.9999999999999716, 372.0000000000000000 ) ) ;
#14386 = VECTOR ( 'NONE', #16132, 1000.000000000000000 ) ;
#14387 = DIRECTION ( 'NONE',  ( 0.000000000000000000, 0.000000000000000000, 1.000000000000000000 ) ) ;
#14388 = AXIS2_PLACEMENT_3D ( 'NONE', #34552, #6076, #14528 ) ;
#14389 = LINE ( 'NONE', #21848, #45831 ) ;
#14390 = CARTESIAN_POINT ( 'NONE',  ( 35.00000000000152767, 16.00000000000000000, 60.00000000000000000 ) ) ;
#14391 = FACE_OUTER_BOUND ( 'NONE', #24777, .T. ) ;
#14392 = ORIENTED_EDGE ( 'NONE', *, *, #9586, .T. ) ;
#14393 = EDGE_LOOP ( 'NONE', ( #19448, #20148, #32225, #20808 ) ) ;
#14394 = DIRECTION ( 'NONE',  ( 0.000000000000000000, 0.000000000000000000, 1.000000000000000000 ) ) ;
#14395 = AXIS2_PLACEMENT_3D ( 'NONE', #28384, #10130, #22435 ) ;
#14396 = EDGE_CURVE ( 'NONE', #24760, #30683, #40996, .T. ) ;
#14397 = ORIENTED_EDGE ( 'NONE', *, *, #3439, .T. ) ;
#14398 = CARTESIAN_POINT ( 'NONE',  ( -0.8811857040074874137, -1.919576306124732401, 9.890170120223997330 ) ) ;
#14399 = FACE_OUTER_BOUND ( 'NONE', #22289, .T. ) ;
#14400 = VERTEX_POINT ( 'NONE', #30210 ) ;
#14401 = CARTESIAN_POINT ( 'NONE',  ( 152.2789002873379900, -1.750000000000010214, -120.2068387089191219 ) ) ;
#14402 = DIRECTION ( 'NONE',  ( -0.000000000000000000, -0.000000000000000000, -1.000000000000000000 ) ) ;
#14403 = ORIENTED_EDGE ( 'NONE', *, *, #2483, .F. ) ;
#14404 = CARTESIAN_POINT ( 'NONE',  ( -2.053349722363707830, 0.3420258690445411864, 9.888808121373916293 ) ) ;
#14405 = CARTESIAN_POINT ( 'NONE',  ( 0.000000000000000000, 175.0000000000000284, -353.7500000000001705 ) ) ;
#14406 = CARTESIAN_POINT ( 'NONE',  ( 343.9999999999998863, -165.0000000000001137, -92.00000000000019895 ) ) ;
#14407 = VECTOR ( 'NONE', #45406, 1000.000000000000000 ) ;
#14408 = EDGE_CURVE ( 'NONE', #7516, #38646, #28559, .T. ) ;
#14409 = ORIENTED_EDGE ( 'NONE', *, *, #29114, .F. ) ;
#14410 = ORIENTED_EDGE ( 'NONE', *, *, #15637, .F. ) ;
#14411 = AXIS2_PLACEMENT_3D ( 'NONE', #32024, #44044, #8910 ) ;
#14412 = CARTESIAN_POINT ( 'NONE',  ( 115.0540265531850395, 2.143131898507847836E-16, 2.568287556927950632 ) ) ;
#14413 = VECTOR ( 'NONE', #38875, 1000.000000000000000 ) ;
#14414 = DIRECTION ( 'NONE',  ( 1.860490536778032451E-50, 0.000000000000000000, -1.000000000000000000 ) ) ;
#14415 = ORIENTED_EDGE ( 'NONE', *, *, #17340, .F. ) ;
#14416 = VERTEX_POINT ( 'NONE', #10211 ) ;
#14417 = EDGE_CURVE ( 'NONE', #23001, #41472, #42267, .T. ) ;
#14418 = CARTESIAN_POINT ( 'NONE',  ( 0.000000000000000000, 0.000000000000000000, 0.000000000000000000 ) ) ;
#14419 = ADVANCED_FACE ( 'NONE', ( #38436 ), #3251, .F. ) ;
#14420 = CARTESIAN_POINT ( 'NONE',  ( 5.781580041794017966, -8.177378108131177825, 3.215106848023477681 ) ) ;
#14421 = VECTOR ( 'NONE', #20972, 1000.000000000000000 ) ;
#14422 = DIRECTION ( 'NONE',  ( -0.000000000000000000, -0.000000000000000000, -1.000000000000000000 ) ) ;
#14423 = CARTESIAN_POINT ( 'NONE',  ( 154.3291528190321458, 1.750000000000009548, 1.843413822775065825 ) ) ;
#14424 = B_SPLINE_CURVE_WITH_KNOTS ( 'NONE', 3,
 ( #5367, #36712, #28972, #21272 ),
 .UNSPECIFIED., .F., .F.,
 ( 4, 4 ),
 ( 0.9895749839358305433, 1.000000000000000000 ),
 .UNSPECIFIED. ) ;
#14425 = FACE_OUTER_BOUND ( 'NONE', #49796, .T. ) ;
#14426 = CARTESIAN_POINT ( 'NONE',  ( 191.5540265531851105, 0.000000000000000000, 119.0682875569279702 ) ) ;
#14427=STYLED_ITEM('',(#50747),#21652);
#14428 = CARTESIAN_POINT ( 'NONE',  ( 14.49999999999999822, -46.12433806312137108, 6.404467680894761372 ) ) ;
#14429 = ORIENTED_EDGE ( 'NONE', *, *, #4628, .F. ) ;
#14430 = EDGE_CURVE ( 'NONE', #36214, #8241, #11472, .T. ) ;
#14431 = CARTESIAN_POINT ( 'NONE',  ( -29.38926261462342993, -40.45084971874754132, 0.000000000000000000 ) ) ;
#14432 = CARTESIAN_POINT ( 'NONE',  ( 85.00000000000056843, 17.00000000000000000, -30.00000000000000000 ) ) ;
#14433 = PLANE ( 'NONE',  #12694 ) ;
#14434 = VECTOR ( 'NONE', #33280, 1000.000000000000000 ) ;
#14435 = LINE ( 'NONE', #36801, #36254 ) ;
#14436 = ORIENTED_EDGE ( 'NONE', *, *, #21761, .T. ) ;
#14437 = DIRECTION ( 'NONE',  ( -1.000000000000000000, -0.000000000000000000, -0.000000000000000000 ) ) ;
#14438 = ORIENTED_EDGE ( 'NONE', *, *, #3049, .T. ) ;
#14439 = CYLINDRICAL_SURFACE ( 'NONE', #13162, 1.750000000000001554 ) ;
#14440 = LINE ( 'NONE', #10349, #7739 ) ;
#14441 = CARTESIAN_POINT ( 'NONE',  ( -114.9999999999991047, 16.00000000000000000, -24.99999999999999289 ) ) ;
#14442 = VERTEX_POINT ( 'NONE', #43015 ) ;
#14443 = AXIS2_PLACEMENT_3D ( 'NONE', #50313, #10856, #42910 ) ;
#14444 = AXIS2_PLACEMENT_3D ( 'NONE', #7725, #23364, #35945 ) ;
#14445 = LINE ( 'NONE', #37817, #30338 ) ;
#14446 = ORIENTED_EDGE ( 'NONE', *, *, #12729, .F. ) ;
#14447 = CARTESIAN_POINT ( 'NONE',  ( 1.080000014128428498, 0.7606467978644730898, 9.943883492372853183 ) ) ;
#14448 = AXIS2_PLACEMENT_3D ( 'NONE', #47997, #47743, #27550 ) ;
#14449 = LINE ( 'NONE', #30359, #804 ) ;
#14450 = CARTESIAN_POINT ( 'NONE',  ( -14.99999999999845812, 17.00000000000000000, 60.00000000000000000 ) ) ;
#14451 = ORIENTED_EDGE ( 'NONE', *, *, #40735, .T. ) ;
#14452 = EDGE_LOOP ( 'NONE', ( #14376, #34470, #16769, #34411 ) ) ;
#14453 = CARTESIAN_POINT ( 'NONE',  ( -44.94597344681493922, 2.143131898507880377E-16, 165.0000000000000000 ) ) ;
#14454 = EDGE_CURVE ( 'NONE', #23796, #36589, #4287, .T. ) ;
#14455 = AXIS2_PLACEMENT_3D ( 'NONE', #14910, #38536, #3351 ) ;
#14456 = ORIENTED_EDGE ( 'NONE', *, *, #19340, .F. ) ;
#14457 = VERTEX_POINT ( 'NONE', #18650 ) ;
#14458 = CARTESIAN_POINT ( 'NONE',  ( -86.69597344681494633, 1.750000000000010658, -79.18171244307201562 ) ) ;
#14459 = DIRECTION ( 'NONE',  ( -1.000000000000000000, 0.000000000000000000, 0.000000000000000000 ) ) ;
#14460 = DIRECTION ( 'NONE',  ( 0.000000000000000000, 0.000000000000000000, 1.000000000000000000 ) ) ;
#14461 = AXIS2_PLACEMENT_3D ( 'NONE', #1251, #21734, #33310 ) ;
#14462 = ORIENTED_EDGE ( 'NONE', *, *, #37131, .T. ) ;
#14463 = LINE ( 'NONE', #37836, #43185 ) ;
#14464 = ORIENTED_EDGE ( 'NONE', *, *, #18350, .F. ) ;
#14465 = AXIS2_PLACEMENT_3D ( 'NONE', #3398, #594, #46725 ) ;
#14466 = DIRECTION ( 'NONE',  ( 1.000000000000000000, 0.000000000000000000, 0.000000000000000000 ) ) ;
#14467 = CARTESIAN_POINT ( 'NONE',  ( -165.0000000000000284, 16.00000000000000000, 0.000000000000000000 ) ) ;
#14468 = VERTEX_POINT ( 'NONE', #19425 ) ;
#14469 = ORIENTED_EDGE ( 'NONE', *, *, #42131, .F. ) ;
#14470 = ORIENTED_EDGE ( 'NONE', *, *, #40472, .T. ) ;
#14471 = CARTESIAN_POINT ( 'NONE',  ( 210.0000000000000568, 0.000000000000000000, -117.4317124430720298 ) ) ;
#14472 = CARTESIAN_POINT ( 'NONE',  ( 155.0540265531850537, 2.143131898507880377E-16, 165.0000000000000000 ) ) ;
#14473 = ORIENTED_EDGE ( 'NONE', *, *, #37076, .F. ) ;
#14474 = CYLINDRICAL_SURFACE ( 'NONE', #46032, 1.750000000000015543 ) ;
#14475 = VERTEX_POINT ( 'NONE', #30466 ) ;
#14476 = CARTESIAN_POINT ( 'NONE',  ( -2.948105490345101387, -9.555557232197246620, 9.282506307616472441 ) ) ;
#14477 = DIRECTION ( 'NONE',  ( -0.000000000000000000, 1.000000000000000000, -1.604368532695312981E-16 ) ) ;
#14478 = VERTEX_POINT ( 'NONE', #11989 ) ;
#14479 = CARTESIAN_POINT ( 'NONE',  ( -24.47767542868268364, 23.18653802921800278, 8.807470649214879543 ) ) ;
#14480 = CARTESIAN_POINT ( 'NONE',  ( 115.0540265531850395, -1.025126265847081886, 119.0682875569279702 ) ) ;
#14481 = DIRECTION ( 'NONE',  ( 0.000000000000000000, 0.000000000000000000, 1.000000000000000000 ) ) ;
#14482 = DIRECTION ( 'NONE',  ( 0.000000000000000000, 0.000000000000000000, -1.000000000000000000 ) ) ;
#14483 = AXIS2_PLACEMENT_3D ( 'NONE', #45103, #9224, #9474 ) ;
#14484 = CARTESIAN_POINT ( 'NONE',  ( 33.30402655318503946, 1.750000000000010658, -79.18171244307201562 ) ) ;
#14485 = ORIENTED_EDGE ( 'NONE', *, *, #304, .F. ) ;
#14486 = EDGE_CURVE ( 'NONE', #18872, #49251, #46339, .T. ) ;
#14487 = CARTESIAN_POINT ( 'NONE',  ( 210.0000000000000568, 0.000000000000000000, 160.8182875569279702 ) ) ;
#14488 = DIRECTION ( 'NONE',  ( -1.860490536778032451E-50, 0.000000000000000000, 1.000000000000000000 ) ) ;
#14489 =( BOUNDED_CURVE ( )  B_SPLINE_CURVE ( 3, ( #43658, #4918, #31645, #11875 ),
 .UNSPECIFIED., .F., .F. ) 
 B_SPLINE_CURVE_WITH_KNOTS ( ( 4, 4 ),
 ( 4.712388980384689674, 6.283185307179586232 ),
 .UNSPECIFIED. ) 
 CURVE ( )  GEOMETRIC_REPRESENTATION_ITEM ( )  RATIONAL_B_SPLINE_CURVE ( ( 1.000000000000000000, 0.8047378541243649375, 0.8047378541243649375, 1.000000000000000000 ) ) 
 REPRESENTATION_ITEM ( '' )  );
#14490 = CARTESIAN_POINT ( 'NONE',  ( -166.6959734468149463, 1.750000000000009992, -159.1817124430720298 ) ) ;
#14491 = LINE ( 'NONE', #10637, #36575 ) ;
#14492 = CARTESIAN_POINT ( 'NONE',  ( 37.50000000000000000, 4.592425496802574367E-15, 10.00000000000000000 ) ) ;
#14493 = DIRECTION ( 'NONE',  ( 0.000000000000000000, 0.000000000000000000, 1.000000000000000000 ) ) ;
#14494 = CARTESIAN_POINT ( 'NONE',  ( 115.0540265531850395, -1.025126265847081442, -0.9317124430720195027 ) ) ;
#14495 = DIRECTION ( 'NONE',  ( 1.000000000000000000, -4.758098676964956461E-16, -8.975803739141899931E-48 ) ) ;
#14496 = PLANE ( 'NONE',  #41043 ) ;
#14497 = VECTOR ( 'NONE', #6275, 1000.000000000000000 ) ;
#14498 = ORIENTED_EDGE ( 'NONE', *, *, #33491, .T. ) ;
#14499 = CARTESIAN_POINT ( 'NONE',  ( 135.0000000000000000, 17.00000000000000000, -90.00000000000000000 ) ) ;
#14500 = CARTESIAN_POINT ( 'NONE',  ( 0.3862712429686894766, -1.188820645368940276, -10.00000000000000000 ) ) ;
#14501 = DIRECTION ( 'NONE',  ( 0.000000000000000000, 0.000000000000000000, 1.000000000000000000 ) ) ;
#14502 = LINE ( 'NONE', #14243, #42038 ) ;
#14503 = DIRECTION ( 'NONE',  ( -1.586032892321652236E-16, -1.000000000000000000, -2.288264760618012091E-48 ) ) ;
#14504 = ORIENTED_EDGE ( 'NONE', *, *, #26298, .T. ) ;
#14505 = EDGE_CURVE ( 'NONE', #14722, #13231, #21961, .T. ) ;
#14506 = VERTEX_POINT ( 'NONE', #34320 ) ;
#14507 = LINE ( 'NONE', #18344, #27523 ) ;
#14508 = CARTESIAN_POINT ( 'NONE',  ( 164.9999999999999716, 16.00000000000000000, 90.00000000000000000 ) ) ;
#14509 = ADVANCED_FACE ( 'NONE', ( #23540 ), #47085, .F. ) ;
#14510 = AXIS2_PLACEMENT_3D ( 'NONE', #36518, #27346, #46545 ) ;
#14511 = EDGE_LOOP ( 'NONE', ( #4180, #27960, #16867 ) ) ;
#14512 = CARTESIAN_POINT ( 'NONE',  ( -12.35406723005387875, 11.51001571518090039, 9.178419661560148768 ) ) ;
#14513 = CARTESIAN_POINT ( 'NONE',  ( 169.0000000000000000, -174.9999999999999716, -97.00000000000014211 ) ) ;
#14514 = CARTESIAN_POINT ( 'NONE',  ( 33.30402655318503946, 1.750000000000009992, 0.8182875569279768335 ) ) ;
#14515 = ORIENTED_EDGE ( 'NONE', *, *, #37787, .F. ) ;
#14516 = ORIENTED_EDGE ( 'NONE', *, *, #27381, .T. ) ;
#14517 = VERTEX_POINT ( 'NONE', #26619 ) ;
#14518 = CARTESIAN_POINT ( 'NONE',  ( 181.0000000000000000, -164.9999999999999432, 341.9999999999998863 ) ) ;
#14519 = CARTESIAN_POINT ( 'NONE',  ( -1.437255894074058515, 3.713052624461494755, 6.606856988583542645E-16 ) ) ;
#14520 = PLANE ( 'NONE',  #18514 ) ;
#14521 = ORIENTED_EDGE ( 'NONE', *, *, #36048, .F. ) ;
#14522 = CYLINDRICAL_SURFACE ( 'NONE', #30062, 1.750000000000010214 ) ;
#14523 = CARTESIAN_POINT ( 'NONE',  ( 350.0000000000000000, -180.9999999999999716, -344.0000000000001705 ) ) ;
#14524 = ORIENTED_EDGE ( 'NONE', *, *, #12940, .T. ) ;
#14525 = VERTEX_POINT ( 'NONE', #7125 ) ;
#14526 = DIRECTION ( 'NONE',  ( 0.000000000000000000, -0.000000000000000000, -1.000000000000000000 ) ) ;
#14527 = FACE_OUTER_BOUND ( 'NONE', #41843, .T. ) ;
#14528 = DIRECTION ( 'NONE',  ( 0.000000000000000000, 0.000000000000000000, -1.000000000000000000 ) ) ;
#14529 = VERTEX_POINT ( 'NONE', #22764 ) ;
#14530 = CARTESIAN_POINT ( 'NONE',  ( 210.0000000000000568, 0.000000000000000000, -119.1817124430720440 ) ) ;
#14531 = CARTESIAN_POINT ( 'NONE',  ( 152.2789002873379900, 1.750000000000010436, -120.2068387089191219 ) ) ;
#14532 = ADVANCED_FACE ( 'NONE', ( #34578 ), #42507, .F. ) ;
#14533 = CARTESIAN_POINT ( 'NONE',  ( -5.670847180967843570, 1.750000000000023537, 121.8434138227750623 ) ) ;
#14534 = FACE_OUTER_BOUND ( 'NONE', #12686, .T. ) ;
#14535 = EDGE_CURVE ( 'NONE', #8324, #19838, #35229, .T. ) ;
#14536 = CARTESIAN_POINT ( 'NONE',  ( -1.035950918207909632, -33.23661552194049307, -2.408242355805840784 ) ) ;
#14537 = ORIENTED_EDGE ( 'NONE', *, *, #23878, .F. ) ;
#14538 = CARTESIAN_POINT ( 'NONE',  ( 181.0000000000000568, 175.0000000000000284, 357.9999999999998863 ) ) ;
#14539 = EDGE_CURVE ( 'NONE', #43275, #37697, #34846, .T. ) ;
#14540 = DIRECTION ( 'NONE',  ( -0.000000000000000000, -0.000000000000000000, -1.000000000000000000 ) ) ;
#14541 = CARTESIAN_POINT ( 'NONE',  ( -46.69597344681494633, 1.750000000000009992, -159.1817124430720298 ) ) ;
#14542 = FACE_OUTER_BOUND ( 'NONE', #47913, .T. ) ;
#14543 = EDGE_CURVE ( 'NONE', #42571, #6887, #46580, .T. ) ;
#14544 = CARTESIAN_POINT ( 'NONE',  ( 0.1287570809895660084, -0.3962735484563127408, -10.00000000000000000 ) ) ;
#14545 = VECTOR ( 'NONE', #35272, 1000.000000000000114 ) ;
#14546 = CARTESIAN_POINT ( 'NONE',  ( 210.0000000000000568, 0.000000000000000000, -119.1817124430720440 ) ) ;
#14547 = ORIENTED_EDGE ( 'NONE', *, *, #49914, .F. ) ;
#14548 = FACE_OUTER_BOUND ( 'NONE', #7606, .T. ) ;
#14549 = CARTESIAN_POINT ( 'NONE',  ( -0.3862712429686895876, 1.188820645368940720, 10.00000000000000000 ) ) ;
#14550 = CARTESIAN_POINT ( 'NONE',  ( 153.3040265531850537, 1.750000000000010658, -119.1817124430720440 ) ) ;
#14551 = ORIENTED_EDGE ( 'NONE', *, *, #29009, .T. ) ;
#14552 = FILL_AREA_STYLE ('',( #37677 ) ) ;
#14553 = CARTESIAN_POINT ( 'NONE',  ( -5.000000000000000000, 184.8000000000000114, -340.2000000000001592 ) ) ;
#14554 =( BOUNDED_CURVE ( )  B_SPLINE_CURVE ( 3, ( #19809, #31889, #24688, #24439 ),
 .UNSPECIFIED., .F., .F. ) 
 B_SPLINE_CURVE_WITH_KNOTS ( ( 4, 4 ),
 ( 1.570796326794896558, 3.141592653589793116 ),
 .UNSPECIFIED. ) 
 CURVE ( )  GEOMETRIC_REPRESENTATION_ITEM ( )  RATIONAL_B_SPLINE_CURVE ( ( 1.000000000000000000, 0.8047378541243649375, 0.8047378541243649375, 1.000000000000000000 ) ) 
 REPRESENTATION_ITEM ( '' )  );
#14555 = VERTEX_POINT ( 'NONE', #19679 ) ;
#14556 = CARTESIAN_POINT ( 'NONE',  ( -114.9999999999981526, 16.00000000000000000, 90.00000000000000000 ) ) ;
#14557 = CYLINDRICAL_SURFACE ( 'NONE', #41833, 1.750000000000001554 ) ;
#14558 = CARTESIAN_POINT ( 'NONE',  ( 31.55402655318503236, 0.000000000000000000, -37.43171244307200141 ) ) ;
#14559 = DIRECTION ( 'NONE',  ( 0.000000000000000000, -1.000000000000000000, 0.000000000000000000 ) ) ;
#14560 = VECTOR ( 'NONE', #22188, 1000.000000000000000 ) ;
#14561 = VERTEX_POINT ( 'NONE', #11476 ) ;
#14562 = B_SPLINE_SURFACE_WITH_KNOTS ( 'NONE', 3, 3, ( 
 ( #15675, #50012, #34435, #14920 ),
 ( #46937, #27487, #26464, #11323 ),
 ( #6967, #38296, #46688, #30835 ),
 ( #43130, #11584, #23629, #3105 ) ),
 .UNSPECIFIED., .F., .F., .F.,
 ( 4, 4 ),
 ( 4, 4 ),
 ( 0.000000000000000000, 1.000000000000000000 ),
 ( 0.000000000000000000, 1.000000000000000000 ),
 .UNSPECIFIED. ) ;
#14563 = EDGE_CURVE ( 'NONE', #40360, #559, #14731, .T. ) ;
#14565 = ORIENTED_EDGE ( 'NONE', *, *, #18160, .T. ) ;
#14564 = ADVANCED_FACE ( 'NONE', ( #195 ), #43274, .T. ) ;
#14566 = VERTEX_POINT ( 'NONE', #39703 ) ;
#14567 = DIRECTION ( 'NONE',  ( -1.000000000000000000, 0.000000000000000000, -7.793956916774525800E-48 ) ) ;
#14568 = ADVANCED_FACE ( 'NONE', ( #444 ), #1205, .F. ) ;
#14569 = ADVANCED_FACE ( 'NONE', ( #39953 ), #1458, .T. ) ;
#14570 = EDGE_LOOP ( 'NONE', ( #46340, #8869, #18825, #38854 ) ) ;
#14571 = LINE ( 'NONE', #49429, #28646 ) ;
#14572 = FACE_OUTER_BOUND ( 'NONE', #42537, .T. ) ;
#14573 = DIRECTION ( 'NONE',  ( 1.000000000000000000, 0.000000000000000000, -0.000000000000000000 ) ) ;
#14574 = EDGE_CURVE ( 'NONE', #42421, #21654, #5919, .T. ) ;
#14575 = LINE ( 'NONE', #12936, #15769 ) ;
#14576 = EDGE_CURVE ( 'NONE', #6375, #40138, #27215, .T. ) ;
#14577 = LINE ( 'NONE', #9719, #2202 ) ;
#14578 = ORIENTED_EDGE ( 'NONE', *, *, #34416, .T. ) ;
#14579 = CARTESIAN_POINT ( 'NONE',  ( 22.69295089195473025, 45.31600496604705341, 7.455576670931136185 ) ) ;
#14580 = CARTESIAN_POINT ( 'NONE',  ( 75.05402655318509630, 1.025126265847089435, 159.0682875569279418 ) ) ;
#14581 = DIRECTION ( 'NONE',  ( 1.000000000000000000, 0.000000000000000000, -0.000000000000000000 ) ) ;
#14582 = ORIENTED_EDGE ( 'NONE', *, *, #34251, .T. ) ;
#14583 = VECTOR ( 'NONE', #17770, 1000.000000000000000 ) ;
#14584 = CARTESIAN_POINT ( 'NONE',  ( 1.335416683881728739, -0.4035165624854742394, 9.955131761384823363 ) ) ;
#14585 = LINE ( 'NONE', #38711, #6494 ) ;
#14586 = ORIENTED_EDGE ( 'NONE', *, *, #41387, .F. ) ;
#14587 = ORIENTED_EDGE ( 'NONE', *, *, #20828, .F. ) ;
#14588 = VERTEX_POINT ( 'NONE', #28895 ) ;
#14589 = DIRECTION ( 'NONE',  ( 1.942330104924128867E-32, 0.000000000000000000, 1.000000000000000000 ) ) ;
#14590 = FACE_OUTER_BOUND ( 'NONE', #9476, .T. ) ;
#14591 = ORIENTED_EDGE ( 'NONE', *, *, #17350, .T. ) ;
#14592 = ADVANCED_FACE ( 'NONE', ( #13233 ), #31755, .F. ) ;
#14593 = CARTESIAN_POINT ( 'NONE',  ( -165.0000000000000284, 16.00000000000000000, 115.0000000000000142 ) ) ;
#14594 = FACE_OUTER_BOUND ( 'NONE', #44467, .T. ) ;
#14595 = FACE_BOUND ( 'NONE', #47294, .T. ) ;
#14596 = EDGE_CURVE ( 'NONE', #4014, #47178, #24592, .T. ) ;
#14597 = CARTESIAN_POINT ( 'NONE',  ( 111.5540265531850679, 0.000000000000000000, 39.06828755692798438 ) ) ;
#14598 = DIRECTION ( 'NONE',  ( 0.000000000000000000, 1.000000000000000000, 0.000000000000000000 ) ) ;
#14599 = ADVANCED_FACE ( 'NONE', ( #23788 ), #40194, .T. ) ;
#14600 = ORIENTED_EDGE ( 'NONE', *, *, #49816, .F. ) ;
#14601 = CARTESIAN_POINT ( 'NONE',  ( -124.9459734468149321, -1.025126265847081886, 79.06828755692797017 ) ) ;
#14602 = CARTESIAN_POINT ( 'NONE',  ( 1.011271242968688311, -0.7347315653655855927, -3.333333333333333481 ) ) ;
#14603 = ORIENTED_EDGE ( 'NONE', *, *, #31934, .T. ) ;
#14604 = ITEM_DEFINED_TRANSFORMATION ( 'NONE', 'NONE', #44653,  #45486 ) ;
#14605 = DIRECTION ( 'NONE',  ( 0.000000000000000000, -1.000000000000000000, 0.000000000000000000 ) ) ;
#14606 = LINE ( 'NONE', #41807, #48765 ) ;
#14607 = B_SPLINE_CURVE_WITH_KNOTS ( 'NONE', 3,
 ( #24316, #8664, #28409, #7907 ),
 .UNSPECIFIED., .F., .F.,
 ( 4, 4 ),
 ( 0.000000000000000000, 0.001246897409371994052 ),
 .UNSPECIFIED. ) ;
#14608 = CYLINDRICAL_SURFACE ( 'NONE', #4401, 1.750000000000008438 ) ;
#14609 = CARTESIAN_POINT ( 'NONE',  ( -2.816440797479544234, 7.430518950465684114, 9.432811472610049819 ) ) ;
#14610 = VERTEX_POINT ( 'NONE', #27896 ) ;
#14611 = CARTESIAN_POINT ( 'NONE',  ( -23.31729631074215092, -24.19776167542410406, -8.016098858316199838 ) ) ;
#14612 = EDGE_CURVE ( 'NONE', #48914, #4790, #16420, .T. ) ;
#14613 = PLANE ( 'NONE',  #46601 ) ;
#14614 = CARTESIAN_POINT ( 'NONE',  ( 0.000000000000000000, 17.00000000000000000, 0.000000000000000000 ) ) ;
#14615 = CARTESIAN_POINT ( 'NONE',  ( -1.133908876584336367, -0.5183204401656656968, 9.981352469109934233 ) ) ;
#14616 = CARTESIAN_POINT ( 'NONE',  ( -88.44597344681494633, 1.025126265847089213, 162.5682875569279133 ) ) ;
#14617 =( BOUNDED_CURVE ( )  B_SPLINE_CURVE ( 3, ( #28701, #36160, #25109, #40757 ),
 .UNSPECIFIED., .F., .F. ) 
 B_SPLINE_CURVE_WITH_KNOTS ( ( 4, 4 ),
 ( 3.141592653589793116, 4.712388980384689674 ),
 .UNSPECIFIED. ) 
 CURVE ( )  GEOMETRIC_REPRESENTATION_ITEM ( )  RATIONAL_B_SPLINE_CURVE ( ( 1.000000000000000000, 0.8047378541243649375, 0.8047378541243649375, 1.000000000000000000 ) ) 
 REPRESENTATION_ITEM ( '' )  );
#14618 = ORIENTED_EDGE ( 'NONE', *, *, #39469, .F. ) ;
#14619 = CARTESIAN_POINT ( 'NONE',  ( 155.0540265531850537, 2.143131898507880377E-16, -37.43171244307205825 ) ) ;
#14621 = ORIENTED_EDGE ( 'NONE', *, *, #38576, .F. ) ;
#14620 = VECTOR ( 'NONE', #8077, 1000.000000000000000 ) ;
#14622 = DIRECTION ( 'NONE',  ( 0.000000000000000000, -1.000000000000000000, 0.000000000000000000 ) ) ;
#14623 = EDGE_CURVE ( 'NONE', #31155, #28209, #5531, .T. ) ;
#14624 = VERTEX_POINT ( 'NONE', #35860 ) ;
#14625 = CARTESIAN_POINT ( 'NONE',  ( -6.695973446814940111, 0.000000000000000000, -165.0000000000000000 ) ) ;
#14626 = DIRECTION ( 'NONE',  ( -1.000000000000000000, 0.000000000000000000, 0.000000000000000000 ) ) ;
#14627 =( BOUNDED_CURVE ( )  B_SPLINE_CURVE ( 3, ( #34516, #11404, #47022, #382 ),
 .UNSPECIFIED., .F., .F. ) 
 B_SPLINE_CURVE_WITH_KNOTS ( ( 4, 4 ),
 ( 4.712388980384689674, 6.283185307179586232 ),
 .UNSPECIFIED. ) 
 CURVE ( )  GEOMETRIC_REPRESENTATION_ITEM ( )  RATIONAL_B_SPLINE_CURVE ( ( 1.000000000000000000, 0.8047378541243649375, 0.8047378541243649375, 1.000000000000000000 ) ) 
 REPRESENTATION_ITEM ( '' )  );
#14628 = VERTEX_POINT ( 'NONE', #32003 ) ;
#14629 = LINE ( 'NONE', #3580, #42075 ) ;
#14630 = CLOSED_SHELL ( 'NONE', ( #38241, #27473, #38886, #29545, #29901, #9337, #47517, #2706, #31985, #35118, #39107, #49681, #25914, #43581, #18053, #30845, #26924, #31222 ) ) ;
#14631 = ORIENTED_EDGE ( 'NONE', *, *, #49627, .T. ) ;
#14632 = EDGE_CURVE ( 'NONE', #33538, #156, #47596, .T. ) ;
#14633 = DIRECTION ( 'NONE',  ( -3.172065784643302499E-16, -1.000000000000000000, 2.537652627714642000E-15 ) ) ;
#14634 = EDGE_CURVE ( 'NONE', #20782, #29885, #3714, .T. ) ;
#14635 = EDGE_LOOP ( 'NONE', ( #44522, #30050, #23714, #3927 ) ) ;
#14636 = CARTESIAN_POINT ( 'NONE',  ( 181.0000000000000568, 175.0000000000000284, 359.9999999999998863 ) ) ;
#14637 = CARTESIAN_POINT ( 'NONE',  ( -166.6959734468149463, -1.750000000000010658, 120.8182875569279702 ) ) ;
#14638 = CARTESIAN_POINT ( 'NONE',  ( -34.38425513258695077, 36.82177522737848108, 8.807470649214879543 ) ) ;
#14639 = CARTESIAN_POINT ( 'NONE',  ( 4.190615033700592740, 4.237471995405366343, 6.606856988583542645E-16 ) ) ;
#14640 = DIRECTION ( 'NONE',  ( -0.000000000000000000, -0.000000000000000000, -1.000000000000000000 ) ) ;
#14641 = ORIENTED_EDGE ( 'NONE', *, *, #6720, .T. ) ;
#14642 = ADVANCED_FACE ( 'NONE', ( #32250 ), #28400, .T. ) ;
#14643 = ORIENTED_EDGE ( 'NONE', *, *, #24692, .F. ) ;
#14644 = CARTESIAN_POINT ( 'NONE',  ( -34.08355720199904226, 2.371364769369340042, 7.455576670931136185 ) ) ;
#14645 = ADVANCED_FACE ( 'NONE', ( #24543 ), #40352, .T. ) ;
#14646 = EDGE_CURVE ( 'NONE', #27796, #7505, #5541, .T. ) ;
#14647 = ORIENTED_EDGE ( 'NONE', *, *, #1173, .T. ) ;
#14648 = CARTESIAN_POINT ( 'NONE',  ( 181.0000000000000000, -184.9999999999999716, -358.0000000000001705 ) ) ;
#14649 = CYLINDRICAL_SURFACE ( 'NONE', #46058, 1.750000000000015543 ) ;
#14650 = ORIENTED_EDGE ( 'NONE', *, *, #8680, .T. ) ;
#14651 = EDGE_CURVE ( 'NONE', #4161, #15488, #33012, .T. ) ;
#14652 = DIRECTION ( 'NONE',  ( -1.000000000000000000, -0.000000000000000000, -0.000000000000000000 ) ) ;
#14653 = EDGE_LOOP ( 'NONE', ( #10666, #44479, #9725, #38091, #18046 ) ) ;
#14654 = CARTESIAN_POINT ( 'NONE',  ( -124.9459734468149321, -1.025126265847081664, -117.4317124430720440 ) ) ;
#14655 = VECTOR ( 'NONE', #19346, 1000.000000000000000 ) ;
#14656 = CARTESIAN_POINT ( 'NONE',  ( 25.61277432017878297, -22.36370378792834757, 7.906207997025717304 ) ) ;
#14657 = DIRECTION ( 'NONE',  ( 0.000000000000000000, 0.000000000000000000, -1.000000000000000000 ) ) ;
#14658 = DIRECTION ( 'NONE',  ( 4.758098676964954489E-16, 1.000000000000000000, 1.751623080406021339E-46 ) ) ;
#14659 = VECTOR ( 'NONE', #1003, 1000.000000000000000 ) ;
#14660 = ORIENTED_EDGE ( 'NONE', *, *, #9599, .F. ) ;
#14661 = CARTESIAN_POINT ( 'NONE',  ( -84.94597344681494633, 2.143131898507880377E-16, 82.56828755692798438 ) ) ;
#14662 = VECTOR ( 'NONE', #32611, 1000.000000000000000 ) ;
#14663 = AXIS2_PLACEMENT_3D ( 'NONE', #23562, #50710, #46861 ) ;
#14664 = DIRECTION ( 'NONE',  ( -0.000000000000000000, -1.000000000000000000, -0.000000000000000000 ) ) ;
#14665 = LINE ( 'NONE', #30324, #5121 ) ;
#14666 = AXIS2_PLACEMENT_3D ( 'NONE', #35718, #24407, #4875 ) ;
#14667 = EDGE_LOOP ( 'NONE', ( #39976, #21218, #34390, #34231, #44832, #43367 ) ) ;
#14668 = EDGE_LOOP ( 'NONE', ( #4620, #37003, #20697, #35430 ) ) ;
#14670 = CARTESIAN_POINT ( 'NONE',  ( 350.0000000000000000, -168.9999999999999432, -342.0000000000001705 ) ) ;
#14669 = VECTOR ( 'NONE', #23027, 1000.000000000000000 ) ;
#14671 = CARTESIAN_POINT ( 'NONE',  ( 2.051144455471369810, 1.664205274803712831, 9.847478953136990398 ) ) ;
#14672 = CARTESIAN_POINT ( 'NONE',  ( 85.00000000000029843, 17.00000000000000000, -84.99999999999998579 ) ) ;
#14673 = CARTESIAN_POINT ( 'NONE',  ( 0.3896797354184660667, -1.262193838292004155, 9.943883492372872723 ) ) ;
#14674 = CARTESIAN_POINT ( 'NONE',  ( -19.99999999999908695, 17.00000000000000000, -24.99999999999999289 ) ) ;
#14675 = VERTEX_POINT ( 'NONE', #18093 ) ;
#14676 = CARTESIAN_POINT ( 'NONE',  ( 1.011271242968683648, 0.7347315653655930312, 10.00000000000000000 ) ) ;
#14677 = PRODUCT ( 'aluminum', 'aluminum', '', ( #16450 ) ) ;
#14678 = LINE ( 'NONE', #3122, #49035 ) ;
#14679 = CARTESIAN_POINT ( 'NONE',  ( -0.3862712429686895876, 1.188820645368940720, 10.00000000000000000 ) ) ;
#14680 = EDGE_CURVE ( 'NONE', #42413, #2747, #2450, .T. ) ;
#14681 = PLANE ( 'NONE',  #27228 ) ;
#14682 = ORIENTED_EDGE ( 'NONE', *, *, #7722, .F. ) ;
#14683 = DIRECTION ( 'NONE',  ( 1.333906992743555050E-23, -1.000000000000000000, 0.000000000000000000 ) ) ;
#14684 = VERTEX_POINT ( 'NONE', #34018 ) ;
#14685 = FACE_OUTER_BOUND ( 'NONE', #49360, .T. ) ;
#14686 = CARTESIAN_POINT ( 'NONE',  ( 34.99999999999997868, 16.00000000000000000, -114.9999999999999858 ) ) ;
#14687 = CARTESIAN_POINT ( 'NONE',  ( 164.9999999999999716, 17.00000000000000000, -30.00000000000001421 ) ) ;
#14688 = ORIENTED_EDGE ( 'NONE', *, *, #14954, .F. ) ;
#14689 = VECTOR ( 'NONE', #24537, 1000.000000000000000 ) ;
#14690 = EDGE_CURVE ( 'NONE', #45274, #16704, #10151, .T. ) ;
#14691 = AXIS2_PLACEMENT_3D ( 'NONE', #20116, #21125, #20365 ) ;
#14692 = EDGE_CURVE ( 'NONE', #24182, #865, #49355, .T. ) ;
#14693 = DIRECTION ( 'NONE',  ( 1.000000000000000000, 0.000000000000000000, 0.000000000000000000 ) ) ;
#14694 = ORIENTED_EDGE ( 'NONE', *, *, #19266, .F. ) ;
#14695 = CARTESIAN_POINT ( 'NONE',  ( 14.86945752723346637, 7.944783388879009145, 2.590526750877053086 ) ) ;
#14696 = DIRECTION ( 'NONE',  ( 1.000000000000000000, 0.000000000000000000, 0.000000000000000000 ) ) ;
#14697=STYLED_ITEM('',(#50747),#4445);
#14698 = CARTESIAN_POINT ( 'NONE',  ( -86.69597344681494633, -1.750000000000010658, 120.8182875569279702 ) ) ;
#14699 = AXIS2_PLACEMENT_3D ( 'NONE', #34902, #7821, #42817 ) ;
#14700 = ORIENTED_EDGE ( 'NONE', *, *, #23322, .T. ) ;
#14701 = ADVANCED_FACE ( 'NONE', ( #29904 ), #44421, .T. ) ;
#14702 = EDGE_LOOP ( 'NONE', ( #6933, #30460, #12375, #35757 ) ) ;
#14703 = LINE ( 'NONE', #6262, #7932 ) ;
#14704 = CARTESIAN_POINT ( 'NONE',  ( -14.99999999999937472, 17.00000000000000000, -30.00000000000000000 ) ) ;
#14705 = ADVANCED_FACE ( 'NONE', ( #44514 ), #21437, .T. ) ;
#14706 = EDGE_CURVE ( 'NONE', #44330, #16449, #29394, .T. ) ;
#14707 = AXIS2_PLACEMENT_3D ( 'NONE', #15519, #26818, #22953 ) ;
#14708 = ORIENTED_EDGE ( 'NONE', *, *, #49365, .T. ) ;
#14709 = VERTEX_POINT ( 'NONE', #17595 ) ;
#14710 = FACE_OUTER_BOUND ( 'NONE', #30676, .T. ) ;
#14711 = FACE_OUTER_BOUND ( 'NONE', #12570, .T. ) ;
#14712 = LINE ( 'NONE', #45976, #10862 ) ;
#14713 = ORIENTED_EDGE ( 'NONE', *, *, #50581, .F. ) ;
#14714 = CARTESIAN_POINT ( 'NONE',  ( 1.275927284277173834, -0.1224368140627448004, 9.976582533991679824 ) ) ;
#14715 = EDGE_CURVE ( 'NONE', #28470, #17971, #17844, .T. ) ;
#14716 = ORIENTED_EDGE ( 'NONE', *, *, #33766, .F. ) ;
#14717 = B_SPLINE_CURVE_WITH_KNOTS ( 'NONE', 3,
 ( #37785, #36784, #41366, #17999 ),
 .UNSPECIFIED., .F., .F.,
 ( 4, 4 ),
 ( 5.938563236642406840E-16, 0.009782300387714819301 ),
 .UNSPECIFIED. ) ;
#14718 = DIRECTION ( 'NONE',  ( 1.612977847700450206E-50, 0.000000000000000000, 1.000000000000000000 ) ) ;
#14719 = CARTESIAN_POINT ( 'NONE',  ( 153.3040265531850537, 1.750000000000010658, -79.18171244307201562 ) ) ;
#14720 = ORIENTED_EDGE ( 'NONE', *, *, #40067, .T. ) ;
#14721 = ORIENTED_EDGE ( 'NONE', *, *, #23750, .F. ) ;
#14722 = VERTEX_POINT ( 'NONE', #45016 ) ;
#14723 = CARTESIAN_POINT ( 'NONE',  ( 339.9999999999998863, -185.0000000000001421, 343.9999999999997726 ) ) ;
#14724 = CARTESIAN_POINT ( 'NONE',  ( -45.64490844644706868, -21.32281559348764333, 8.807470649214879543 ) ) ;
#14725 = VERTEX_POINT ( 'NONE', #9896 ) ;
#14726 = CARTESIAN_POINT ( 'NONE',  ( 35.05402655318504657, 2.143131898507880377E-16, 122.5682875569279702 ) ) ;
#14728 = ORIENTED_EDGE ( 'NONE', *, *, #719, .T. ) ;
#14727 = AXIS2_PLACEMENT_3D ( 'NONE', #45337, #42025, #14317 ) ;
#14729 = CARTESIAN_POINT ( 'NONE',  ( -8.445973446814914354, 2.143131898507880377E-16, -160.9317124430720298 ) ) ;
#14730 = PRESENTATION_STYLE_ASSIGNMENT (( #6289 ) ) ;
#14732 = ORIENTED_EDGE ( 'NONE', *, *, #11449, .T. ) ;
#14731 = CIRCLE ( 'NONE', #43402, 1.750000000000008438 ) ;
#14733 = CARTESIAN_POINT ( 'NONE',  ( -25.61277432017861955, 22.36370378792854297, 7.906207997025717304 ) ) ;
#14734 = CARTESIAN_POINT ( 'NONE',  ( 115.0540265531850395, 2.143131898507847836E-16, 119.0682875569279844 ) ) ;
#14735 = CARTESIAN_POINT ( 'NONE',  ( 13.35436367797824353, 31.26996044524050333, 7.906207997025717304 ) ) ;
#14736 = LINE ( 'NONE', #18074, #45754 ) ;
#14737 = AXIS2_PLACEMENT_3D ( 'NONE', #38570, #38058, #30348 ) ;
#14738 = CARTESIAN_POINT ( 'NONE',  ( 32.27890028733795447, 1.750000000000009548, -78.15658617722490931 ) ) ;
#14739 = ORIENTED_EDGE ( 'NONE', *, *, #32162, .T. ) ;
#14741 = VECTOR ( 'NONE', #287, 1000.000000000000000 ) ;
#14740 = CARTESIAN_POINT ( 'NONE',  ( -208.4459734468149463, 0.000000000000000000, 42.56828755692798438 ) ) ;
#14742 = ADVANCED_FACE ( 'NONE', ( #25551 ), #36698, .T. ) ;
#14743 = CARTESIAN_POINT ( 'NONE',  ( 0.5113015165352333691, 1.175527691268683395, 9.948547179989619238 ) ) ;
#14744 = DIRECTION ( 'NONE',  ( 0.000000000000000000, -1.000000000000000000, 0.000000000000000000 ) ) ;
#14745 = DIRECTION ( 'NONE',  ( -1.000000000000000000, 0.000000000000000000, 0.000000000000000000 ) ) ;
#14746 = ADVANCED_FACE ( 'NONE', ( #41954 ), #10902, .F. ) ;
#14747 = VECTOR ( 'NONE', #20007, 1000.000000000000000 ) ;
#14748 = DIRECTION ( 'NONE',  ( 0.000000000000000000, -1.000000000000000000, 1.604368532695312981E-16 ) ) ;
#14749 = CARTESIAN_POINT ( 'NONE',  ( -210.0000000000000568, 0.000000000000000000, 160.8182875569279702 ) ) ;
#14750 = FACE_BOUND ( 'NONE', #28963, .T. ) ;
#14751 = DIRECTION ( 'NONE',  ( 0.000000000000000000, 0.000000000000000000, -1.000000000000000000 ) ) ;
#14752 = ORIENTED_EDGE ( 'NONE', *, *, #27869, .F. ) ;
#14753 = CARTESIAN_POINT ( 'NONE',  ( -225.0000000000000568, 164.9999999999999716, 111.9999999999999858 ) ) ;
#14754 = CARTESIAN_POINT ( 'NONE',  ( 26.18032376592674737, -21.95228666728361233, 7.455576670931136185 ) ) ;
#14755 = CARTESIAN_POINT ( 'NONE',  ( -13.92102703536724384, -30.85732372859812500, 8.356839323120299312 ) ) ;
#14756 = CARTESIAN_POINT ( 'NONE',  ( 17.51065725283126895, -28.41934970907778890, -9.367992836599954742 ) ) ;
#14757 = LINE ( 'NONE', #46020, #44631 ) ;
#14758 = ORIENTED_EDGE ( 'NONE', *, *, #8771, .F. ) ;
#14759 = EDGE_LOOP ( 'NONE', ( #21385, #43174, #15137, #12477 ) ) ;
#14760 = VECTOR ( 'NONE', #45599, 1000.000000000000000 ) ;
#14761 = CARTESIAN_POINT ( 'NONE',  ( -0.3862712429686809279, -1.188820645368943163, 10.00000000000000000 ) ) ;
#14762 = CARTESIAN_POINT ( 'NONE',  ( 2.538055338523177440, 33.28424297489108596, -9.367992836599954742 ) ) ;
#14763 = VECTOR ( 'NONE', #43966, 1000.000000000000000 ) ;
#14764 =( BOUNDED_CURVE ( )  B_SPLINE_CURVE ( 3, ( #17851, #18102, #34028, #33022 ),
 .UNSPECIFIED., .F., .F. ) 
 B_SPLINE_CURVE_WITH_KNOTS ( ( 4, 4 ),
 ( 4.712388980384689674, 6.283185307179586232 ),
 .UNSPECIFIED. ) 
 CURVE ( )  GEOMETRIC_REPRESENTATION_ITEM ( )  RATIONAL_B_SPLINE_CURVE ( ( 1.000000000000000000, 0.8047378541243649375, 0.8047378541243649375, 1.000000000000000000 ) ) 
 REPRESENTATION_ITEM ( '' )  );
#14765 = B_SPLINE_CURVE_WITH_KNOTS ( 'NONE', 3,
 ( #7699, #35422, #35165, #22828 ),
 .UNSPECIFIED., .F., .F.,
 ( 4, 4 ),
 ( 0.01010185847678718787, 0.01012833122192013588 ),
 .UNSPECIFIED. ) ;
#14766 = CIRCLE ( 'NONE', #9069, 1.880036658038868103 ) ;
#14767 = VERTEX_POINT ( 'NONE', #11172 ) ;
#14768 = CARTESIAN_POINT ( 'NONE',  ( -124.9459734468149463, 2.143131898507847836E-16, 82.56828755692797017 ) ) ;
#14769 = DIRECTION ( 'NONE',  ( 0.000000000000000000, 0.000000000000000000, 1.000000000000000000 ) ) ;
#14770 = CARTESIAN_POINT ( 'NONE',  ( -3.996390545799824334, 16.57371371864897469, 8.953103998512858652 ) ) ;
#14771 = EDGE_LOOP ( 'NONE', ( #34337, #20149, #33278 ) ) ;
#14772 = ORIENTED_EDGE ( 'NONE', *, *, #37169, .T. ) ;
#14773 = ADVANCED_FACE ( 'NONE', ( #38631, #38376 ), #15518, .T. ) ;
#14774 = AXIS2_PLACEMENT_3D ( 'NONE', #23234, #18620, #38915 ) ;
#14775 =( BOUNDED_CURVE ( )  B_SPLINE_CURVE ( 3, ( #11647, #3423, #35022, #19072 ),
 .UNSPECIFIED., .F., .F. ) 
 B_SPLINE_CURVE_WITH_KNOTS ( ( 4, 4 ),
 ( 0.000000000000000000, 1.570796326794896558 ),
 .UNSPECIFIED. ) 
 CURVE ( )  GEOMETRIC_REPRESENTATION_ITEM ( )  RATIONAL_B_SPLINE_CURVE ( ( 1.000000000000000000, 0.8047378541243649375, 0.8047378541243649375, 1.000000000000000000 ) ) 
 REPRESENTATION_ITEM ( '' )  );
#14776 = ORIENTED_EDGE ( 'NONE', *, *, #39401, .T. ) ;
#14777 = CARTESIAN_POINT ( 'NONE',  ( 0.5113015165352333691, 1.175527691268683395, 9.948547179989619238 ) ) ;
#14778 = FACE_OUTER_BOUND ( 'NONE', #23548, .T. ) ;
#14779 = CARTESIAN_POINT ( 'NONE',  ( 7.500000000000000000, 224.9999999999999716, -240.0000000000000000 ) ) ;
#14780 = VERTEX_POINT ( 'NONE', #30412 ) ;
#14781 = FACE_OUTER_BOUND ( 'NONE', #30496, .T. ) ;
#14782 = CARTESIAN_POINT ( 'NONE',  ( 32.27890028733795447, -1.750000000000010214, 81.84341382277507648 ) ) ;
#14783 = SURFACE_SIDE_STYLE ('',( #42233 ) ) ;
#14784 = VERTEX_POINT ( 'NONE', #31183 ) ;
#14785 = ORIENTED_EDGE ( 'NONE', *, *, #7273, .T. ) ;
#14786 = CARTESIAN_POINT ( 'NONE',  ( 111.5540265531850679, 0.000000000000000000, 159.0682875569279702 ) ) ;
#14787 = CARTESIAN_POINT ( 'NONE',  ( -126.6959734468149321, -1.749999999999996891, 160.8182875569279702 ) ) ;
#14788 =( BOUNDED_CURVE ( )  B_SPLINE_CURVE ( 3, ( #49273, #36793, #49016, #41624 ),
 .UNSPECIFIED., .F., .F. ) 
 B_SPLINE_CURVE_WITH_KNOTS ( ( 4, 4 ),
 ( 4.712388980384689674, 6.283185307179586232 ),
 .UNSPECIFIED. ) 
 CURVE ( )  GEOMETRIC_REPRESENTATION_ITEM ( )  RATIONAL_B_SPLINE_CURVE ( ( 1.000000000000000000, 0.8047378541243649375, 0.8047378541243649375, 1.000000000000000000 ) ) 
 REPRESENTATION_ITEM ( '' )  );
#14789 = CARTESIAN_POINT ( 'NONE',  ( 152.2789002873379900, -1.750000000000010214, 119.7931612910808781 ) ) ;
#14790 = ORIENTED_EDGE ( 'NONE', *, *, #38529, .T. ) ;
#14791 = ORIENTED_EDGE ( 'NONE', *, *, #28995, .T. ) ;
#14792 = DIRECTION ( 'NONE',  ( -1.000000000000000000, -0.000000000000000000, -0.000000000000000000 ) ) ;
#14793 = CARTESIAN_POINT ( 'NONE',  ( 34.32915281903212446, 1.750000000000010214, -118.1565861772249519 ) ) ;
#14794 = FACE_OUTER_BOUND ( 'NONE', #2666, .T. ) ;
#14795 = CARTESIAN_POINT ( 'NONE',  ( -4.641001526964560142, -50.00000000000000711, -8.016098858316199838 ) ) ;
#14796 = ORIENTED_EDGE ( 'NONE', *, *, #50042, .F. ) ;
#14797 = DIRECTION ( 'NONE',  ( -0.000000000000000000, -1.000000000000000000, -0.000000000000000000 ) ) ;
#14798 = CARTESIAN_POINT ( 'NONE',  ( 10.00000000000000000, -250.0000000000000000, -224.9999999999999716 ) ) ;
#14799 = CARTESIAN_POINT ( 'NONE',  ( 6.204997580903516941, -7.388441598285492518, 229.0000000000000000 ) ) ;
#14800 = PLANE ( 'NONE',  #47333 ) ;
#14801 = AXIS2_PLACEMENT_3D ( 'NONE', #37391, #18345, #45777 ) ;
#14802 = CARTESIAN_POINT ( 'NONE',  ( -86.69597344681494633, 1.750000000000010658, -79.18171244307201562 ) ) ;
#14803 = VECTOR ( 'NONE', #33573, 1000.000000000000000 ) ;
#14804 = CARTESIAN_POINT ( 'NONE',  ( -543.5890838333644979, 54.43801056904003133, -176.2581102438216192 ) ) ;
#14805 = ORIENTED_EDGE ( 'NONE', *, *, #9520, .F. ) ;
#14806 = CARTESIAN_POINT ( 'NONE',  ( 26.18032376592674737, -21.95228666728361233, 7.455576670931136185 ) ) ;
#14807 = CARTESIAN_POINT ( 'NONE',  ( -37.09740935455761246, 5.526036232978498219, 8.506357886886741326 ) ) ;
#14808 = VECTOR ( 'NONE', #21001, 1000.000000000000000 ) ;
#14809 = B_SPLINE_CURVE_WITH_KNOTS ( 'NONE', 3,
 ( #31151, #6776, #26532, #30388 ),
 .UNSPECIFIED., .F., .F.,
 ( 4, 4 ),
 ( 8.940560153363745023E-19, 0.0003137973356796201589 ),
 .UNSPECIFIED. ) ;
#14810 = DIRECTION ( 'NONE',  ( -1.000000000000000000, -0.000000000000000000, -0.000000000000000000 ) ) ;
#14811 = ORIENTED_EDGE ( 'NONE', *, *, #37188, .T. ) ;
#14812 = CARTESIAN_POINT ( 'NONE',  ( 115.0540265531850395, 2.143131898507847836E-16, 165.0000000000000000 ) ) ;
#14813 = CARTESIAN_POINT ( 'NONE',  ( 350.0000000000001137, 169.0000000000000000, 355.9999999999997726 ) ) ;
#14814 = ORIENTED_EDGE ( 'NONE', *, *, #35565, .F. ) ;
#14815 = CARTESIAN_POINT ( 'NONE',  ( 356.0000000000000000, -165.0000000000001137, -349.9999999999998863 ) ) ;
#14816 = FACE_OUTER_BOUND ( 'NONE', #4443, .T. ) ;
#14817 = CARTESIAN_POINT ( 'NONE',  ( -0.2996946835593986558, -1.197003681518488794, 9.969907203203803192 ) ) ;
#14818 = LINE ( 'NONE', #42016, #20892 ) ;
#14819 = ORIENTED_EDGE ( 'NONE', *, *, #39731, .T. ) ;
#14820 = CARTESIAN_POINT ( 'NONE',  ( -1.011271242968688533, 0.7347315653655859258, 10.00000000000000000 ) ) ;
#14821 = B_SPLINE_CURVE_WITH_KNOTS ( 'NONE', 3,
 ( #21602, #48762, #15372, #7673 ),
 .UNSPECIFIED., .F., .F.,
 ( 4, 4 ),
 ( 0.000000000000000000, 0.001249001129225746874 ),
 .UNSPECIFIED. ) ;
#14822 = VERTEX_POINT ( 'NONE', #35049 ) ;
#14823 = ORIENTED_EDGE ( 'NONE', *, *, #11590, .F. ) ;
#14824 = FACE_OUTER_BOUND ( 'NONE', #35374, .T. ) ;
#14825 = ORIENTED_EDGE ( 'NONE', *, *, #35307, .F. ) ;
#14826 = FACE_OUTER_BOUND ( 'NONE', #10592, .T. ) ;
#14827 = FACE_OUTER_BOUND ( 'NONE', #16748, .T. ) ;
#14828 = CARTESIAN_POINT ( 'NONE',  ( 0.3440687301471855308, 1.609937937016769460, 9.936700280135880803 ) ) ;
#14829 = ADVANCED_FACE ( 'NONE', ( #7312 ), #46769, .T. ) ;
#14830 = DIRECTION ( 'NONE',  ( -0.000000000000000000, -0.000000000000000000, -1.000000000000000000 ) ) ;
#14831 = LINE ( 'NONE', #27401, #44770 ) ;
#14832 = ORIENTED_EDGE ( 'NONE', *, *, #32308, .T. ) ;
#14833 = EDGE_CURVE ( 'NONE', #22540, #27098, #19098, .T. ) ;
#14834 = DIRECTION ( 'NONE',  ( -1.000000000000000000, -0.000000000000000000, -0.000000000000000000 ) ) ;
#14835 = AXIS2_PLACEMENT_3D ( 'NONE', #20849, #43677, #44677 ) ;
#14836 = DIRECTION ( 'NONE',  ( 0.000000000000000000, 0.000000000000000000, 1.000000000000000000 ) ) ;
#14837 = CARTESIAN_POINT ( 'NONE',  ( -208.1473046169136580, 160.1880105690400171, 472.8425600500171981 ) ) ;
#14838 = EDGE_CURVE ( 'NONE', #15868, #34290, #16716, .T. ) ;
#14839 = CARTESIAN_POINT ( 'NONE',  ( -167.4999999999999432, -112.5000000000000000, 10.00000000000000000 ) ) ;
#14840 = ORIENTED_EDGE ( 'NONE', *, *, #40939, .F. ) ;
#14841 = CARTESIAN_POINT ( 'NONE',  ( 358.0000000000000568, -167.8284271247463550, -342.8284271247465540 ) ) ;
#14842 = FACE_OUTER_BOUND ( 'NONE', #2163, .T. ) ;
#14843 = EDGE_LOOP ( 'NONE', ( #43942, #17241, #42924, #29425, #22482, #39673 ) ) ;
#14844 = ORIENTED_EDGE ( 'NONE', *, *, #10830, .T. ) ;
#14845 = ORIENTED_EDGE ( 'NONE', *, *, #25993, .T. ) ;
#14846 = CARTESIAN_POINT ( 'NONE',  ( 166.9999999999999716, -174.9999999999999716, -356.0000000000001705 ) ) ;
#14847 = AXIS2_PLACEMENT_3D ( 'NONE', #5928, #9529, #5174 ) ;
#14848 = EDGE_CURVE ( 'NONE', #17123, #39145, #39661, .T. ) ;
#14849 = CARTESIAN_POINT ( 'NONE',  ( 343.9999999999999432, -183.0000000000001421, 358.0000000000001137 ) ) ;
#14850 = VECTOR ( 'NONE', #1453, 1000.000000000000000 ) ;
#14851 = VERTEX_POINT ( 'NONE', #46524 ) ;
#14852 = LINE ( 'NONE', #30503, #27404 ) ;
#14853 = CARTESIAN_POINT ( 'NONE',  ( 183.0000000000000284, -174.9999999999999716, -111.0000000000001563 ) ) ;
#14854 = ADVANCED_FACE ( 'NONE', ( #23483 ), #11416, .T. ) ;
#14855 = FACE_BOUND ( 'NONE', #73, .T. ) ;
#14856 = CARTESIAN_POINT ( 'NONE',  ( 342.0000000000000000, 169.0000000000000000, 343.9999999999998863 ) ) ;
#14857 = CARTESIAN_POINT ( 'NONE',  ( 357.9999999999999432, 177.9999999999999432, -353.0000000000000568 ) ) ;
#14858 = CARTESIAN_POINT ( 'NONE',  ( 72.27890028733797578, -1.750000000000010214, 81.84341382277507648 ) ) ;
#14859 = CARTESIAN_POINT ( 'NONE',  ( 21.58778298521313843, -25.34222074689757065, 3.199614146704519602 ) ) ;
#14860 = LINE ( 'NONE', #18446, #10872 ) ;
#14861 = ADVANCED_FACE ( 'NONE', ( #22704, #7573 ), #38124, .T. ) ;
#14862 = EDGE_CURVE ( 'NONE', #5959, #46304, #3965, .T. ) ;
#14863 = ORIENTED_EDGE ( 'NONE', *, *, #44461, .T. ) ;
#14864 = CARTESIAN_POINT ( 'NONE',  ( -88.44597344681497475, 0.000000000000000000, 165.0000000000000000 ) ) ;
#14865 = B_SPLINE_CURVE_WITH_KNOTS ( 'NONE', 3,
 ( #33482, #45490, #6515, #22174 ),
 .UNSPECIFIED., .F., .F.,
 ( 4, 4 ),
 ( 0.000000000000000000, 2.804146970186931250E-05 ),
 .UNSPECIFIED. ) ;
#14866 = DIRECTION ( 'NONE',  ( 0.000000000000000000, -4.687818848539279227E-49, 1.000000000000000000 ) ) ;
#14867 = ADVANCED_FACE ( 'NONE', ( #47290 ), #9090, .F. ) ;
#14868 = EDGE_CURVE ( 'NONE', #13365, #14561, #44860, .T. ) ;
#14869 =( BOUNDED_CURVE ( )  B_SPLINE_CURVE ( 3, ( #48109, #36647, #45033, #13244 ),
 .UNSPECIFIED., .F., .F. ) 
 B_SPLINE_CURVE_WITH_KNOTS ( ( 4, 4 ),
 ( 1.570796326794896558, 3.141592653589793116 ),
 .UNSPECIFIED. ) 
 CURVE ( )  GEOMETRIC_REPRESENTATION_ITEM ( )  RATIONAL_B_SPLINE_CURVE ( ( 1.000000000000000000, 0.8047378541243649375, 0.8047378541243649375, 1.000000000000000000 ) ) 
 REPRESENTATION_ITEM ( '' )  );
#14870 = DIRECTION ( 'NONE',  ( 0.000000000000000000, 0.000000000000000000, 1.000000000000000000 ) ) ;
#14871 = VERTEX_POINT ( 'NONE', #48035 ) ;
#14872 = EDGE_CURVE ( 'NONE', #19026, #18177, #28582, .T. ) ;
#14873 = CARTESIAN_POINT ( 'NONE',  ( -12.16428377685542017, -11.73151505502925929, -9.008049429158100807 ) ) ;
#14874 = CARTESIAN_POINT ( 'NONE',  ( 210.0000000000000568, 0.000000000000000000, -159.1817124430720298 ) ) ;
#14875 = AXIS2_PLACEMENT_3D ( 'NONE', #14363, #21056, #21819 ) ;
#14876 = ADVANCED_FACE ( 'NONE', ( #19865 ), #22959, .T. ) ;
#14877 = CARTESIAN_POINT ( 'NONE',  ( 48.99656738986517723, -11.00747004110342431, 1.847720168420772691 ) ) ;
#14878 = CARTESIAN_POINT ( 'NONE',  ( -6.875132362119187768, 50.00000000000000711, 8.356839323120299312 ) ) ;
#14879 = DIRECTION ( 'NONE',  ( 1.000000000000000000, -0.000000000000000000, -0.000000000000000000 ) ) ;
#14880 = ORIENTED_EDGE ( 'NONE', *, *, #9799, .F. ) ;
#14881 = CARTESIAN_POINT ( 'NONE',  ( 73.30402655318508209, 0.000000000000000000, 165.0000000000000000 ) ) ;
#14882 = VERTEX_POINT ( 'NONE', #24241 ) ;
#14883 = CARTESIAN_POINT ( 'NONE',  ( 34.08355720199905647, -2.371364769369109116, 7.455576670931136185 ) ) ;
#14884 = ORIENTED_EDGE ( 'NONE', *, *, #33974, .T. ) ;
#14885 = CARTESIAN_POINT ( 'NONE',  ( -8.445973446814976526, 0.000000000000000000, 42.56828755692802702 ) ) ;
#14886 = VECTOR ( 'NONE', #34723, 1000.000000000000000 ) ;
#14887 = ORIENTED_EDGE ( 'NONE', *, *, #21786, .F. ) ;
#14888 = EDGE_CURVE ( 'NONE', #5210, #11165, #24750, .T. ) ;
#14889 = ORIENTED_EDGE ( 'NONE', *, *, #19941, .T. ) ;
#14890 = EDGE_CURVE ( 'NONE', #42480, #28309, #46198, .T. ) ;
#14891 = ADVANCED_FACE ( 'NONE', ( #39900 ), #25195, .T. ) ;
#14892 = VERTEX_POINT ( 'NONE', #47030 ) ;
#14893 = CARTESIAN_POINT ( 'NONE',  ( 214.9999999999999432, -172.9999999999999716, 232.0000000000000284 ) ) ;
#14894 = DIRECTION ( 'NONE',  ( -1.000000000000000000, 0.000000000000000000, 0.000000000000000000 ) ) ;
#14895 = EDGE_LOOP ( 'NONE', ( #20552, #17447, #3783, #43235, #21957, #19647, #26719, #4216, #32220, #47821, #20117, #44388, #2891, #3316 ) ) ;
#14896 = CARTESIAN_POINT ( 'NONE',  ( 0.000000000000000000, 0.000000000000000000, 15.00000000000000000 ) ) ;
#14897 = LINE ( 'NONE', #41589, #14407 ) ;
#14898 = CARTESIAN_POINT ( 'NONE',  ( 73.30402655318508209, 1.750000000000010658, 120.8182875569279702 ) ) ;
#14899 = VERTEX_POINT ( 'NONE', #16283 ) ;
#14900 = ORIENTED_EDGE ( 'NONE', *, *, #49125, .F. ) ;
#14901 = CARTESIAN_POINT ( 'NONE',  ( -49.67735855322972327, 8.912210285362091255, 8.356839323120299312 ) ) ;
#14902 = EDGE_CURVE ( 'NONE', #21347, #14373, #18019, .T. ) ;
#14903 = CARTESIAN_POINT ( 'NONE',  ( 5.551115123125782702E-14, -168.9999999999999432, 343.9999999999997726 ) ) ;
#14904 = ORIENTED_EDGE ( 'NONE', *, *, #6986, .T. ) ;
#14905 = DIRECTION ( 'NONE',  ( 1.000000000000000000, 0.000000000000000000, 0.000000000000000000 ) ) ;
#14906 = CARTESIAN_POINT ( 'NONE',  ( -6.695973446814940111, 1.750000000000024203, -79.18171244307201562 ) ) ;
#14907 = ORIENTED_EDGE ( 'NONE', *, *, #25258, .F. ) ;
#14908 = CARTESIAN_POINT ( 'NONE',  ( 340.0000000000000568, 165.0000000000000000, 343.9999999999997726 ) ) ;
#14909 = VECTOR ( 'NONE', #39738, 1000.000000000000000 ) ;
#14910 = CARTESIAN_POINT ( 'NONE',  ( 153.2026953830863647, -98.56198943095992604, -17.65743994998277699 ) ) ;
#14911 = ORIENTED_EDGE ( 'NONE', *, *, #10019, .F. ) ;
#14912 = ADVANCED_FACE ( 'NONE', ( #24492 ), #16537, .T. ) ;
#14913 = CARTESIAN_POINT ( 'NONE',  ( 210.0000000000000568, 0.000000000000000000, 120.8182875569279702 ) ) ;
#14914 = CARTESIAN_POINT ( 'NONE',  ( 1.011271242968677653, 0.7347315653656002477, 10.00000000000000000 ) ) ;
#14915 = CARTESIAN_POINT ( 'NONE',  ( 2.948105490344985480, 9.555557232197198658, 9.282506307616484875 ) ) ;
#14916 = CARTESIAN_POINT ( 'NONE',  ( 358.0000000000000000, -169.0000000000001137, -344.0000000000002842 ) ) ;
#14917 = VECTOR ( 'NONE', #46192, 1000.000000000000000 ) ;
#14918 = ORIENTED_EDGE ( 'NONE', *, *, #34426, .F. ) ;
#14919 = EDGE_CURVE ( 'NONE', #13193, #46082, #4730, .T. ) ;
#14920 = CARTESIAN_POINT ( 'NONE',  ( -1.011271242968688533, 0.7347315653655859258, 10.00000000000000000 ) ) ;
#14921 = CYLINDRICAL_SURFACE ( 'NONE', #37384, 2.000000000000001776 ) ;
#14922 = DIRECTION ( 'NONE',  ( -1.000000000000000000, 0.000000000000000000, 0.000000000000000000 ) ) ;
#14923 = ORIENTED_EDGE ( 'NONE', *, *, #5504, .T. ) ;
#14924 = ORIENTED_EDGE ( 'NONE', *, *, #1173, .F. ) ;
#14925 = CARTESIAN_POINT ( 'NONE',  ( -124.9459734468149321, -1.025126265847081664, 82.56828755692798438 ) ) ;
#14926 =( BOUNDED_CURVE ( )  B_SPLINE_CURVE ( 3, ( #25888, #26123, #30484, #37695 ),
 .UNSPECIFIED., .F., .F. ) 
 B_SPLINE_CURVE_WITH_KNOTS ( ( 4, 4 ),
 ( 0.000000000000000000, 1.570796326794896558 ),
 .UNSPECIFIED. ) 
 CURVE ( )  GEOMETRIC_REPRESENTATION_ITEM ( )  RATIONAL_B_SPLINE_CURVE ( ( 1.000000000000000000, 0.8047378541243649375, 0.8047378541243649375, 1.000000000000000000 ) ) 
 REPRESENTATION_ITEM ( '' )  );
#14927 = DIRECTION ( 'NONE',  ( -0.000000000000000000, -1.000000000000000000, 2.537652627714643577E-15 ) ) ;
#14928 = CARTESIAN_POINT ( 'NONE',  ( 24.39427009665984869, 44.07992421011656603, 8.807470649214879543 ) ) ;
#14929 = ADVANCED_FACE ( 'NONE', ( #47786 ), #31948, .F. ) ;
#14930 = ADVANCED_FACE ( 'NONE', ( #43718 ), #21902, .T. ) ;
#14931 = LINE ( 'NONE', #46189, #9428 ) ;
#14932 = CARTESIAN_POINT ( 'NONE',  ( 22.69295089195473736, 45.31600496604706052, 7.455576670931136185 ) ) ;
#14933 = ORIENTED_EDGE ( 'NONE', *, *, #36920, .T. ) ;
#14934 = EDGE_CURVE ( 'NONE', #20787, #19082, #44712, .T. ) ;
#14935 = CARTESIAN_POINT ( 'NONE',  ( 48.34672127938079456, -13.00749071703866555, 3.199614146704519602 ) ) ;
#14936 =( BOUNDED_CURVE ( )  B_SPLINE_CURVE ( 3, ( #5554, #16349, #21203, #36895 ),
 .UNSPECIFIED., .F., .F. ) 
 B_SPLINE_CURVE_WITH_KNOTS ( ( 4, 4 ),
 ( 0.000000000000000000, 1.570796326794896558 ),
 .UNSPECIFIED. ) 
 CURVE ( )  GEOMETRIC_REPRESENTATION_ITEM ( )  RATIONAL_B_SPLINE_CURVE ( ( 1.000000000000000000, 0.8047378541243649375, 0.8047378541243649375, 1.000000000000000000 ) ) 
 REPRESENTATION_ITEM ( '' )  );
#14937 = AXIS2_PLACEMENT_3D ( 'NONE', #31716, #32207, #4248 ) ;
#14938 = ADVANCED_FACE ( 'NONE', ( #41645 ), #13301, .T. ) ;
#14939 = CARTESIAN_POINT ( 'NONE',  ( 1.164014690938906416, -0.7287989552214911848, 9.946805383069625250 ) ) ;
#14940 = CARTESIAN_POINT ( 'NONE',  ( -0.06526599240255732959, 1.373921316405938065, 9.972175347158398040 ) ) ;
#14941 = ADVANCED_FACE ( 'NONE', ( #21635 ), #12569, .T. ) ;
#14942 = LINE ( 'NONE', #41884, #14092 ) ;
#14943 = ORIENTED_EDGE ( 'NONE', *, *, #29985, .T. ) ;
#14944 = DIRECTION ( 'NONE',  ( -1.000000000000000000, 0.000000000000000000, 0.000000000000000000 ) ) ;
#14945 = ORIENTED_EDGE ( 'NONE', *, *, #999, .F. ) ;
#14946 = CARTESIAN_POINT ( 'NONE',  ( 0.000000000000000000, 181.0000000000000284, -358.0000000000002274 ) ) ;
#14947 = VECTOR ( 'NONE', #2667, 1000.000000000000000 ) ;
#14948 = CARTESIAN_POINT ( 'NONE',  ( 341.6568542494921417, -185.0000000000001137, 360.0000000000002274 ) ) ;
#14949 = CARTESIAN_POINT ( 'NONE',  ( -5.000000000000000000, 175.0000000000000284, -350.0000000000002274 ) ) ;
#14950 = VERTEX_POINT ( 'NONE', #21380 ) ;
#14951=STYLED_ITEM('',(#50747),#38799);
#14952 = DIRECTION ( 'NONE',  ( -0.000000000000000000, -0.000000000000000000, -1.000000000000000000 ) ) ;
#14953 = B_SPLINE_CURVE_WITH_KNOTS ( 'NONE', 3,
 ( #13450, #17302, #45218, #33967 ),
 .UNSPECIFIED., .F., .F.,
 ( 4, 4 ),
 ( 0.000000000000000000, 0.2637263876330692147 ),
 .UNSPECIFIED. ) ;
#14954 = EDGE_CURVE ( 'NONE', #31678, #22771, #33707, .T. ) ;
#14955 = AXIS2_PLACEMENT_3D ( 'NONE', #14903, #25501, #18729 ) ;
#14956 = CARTESIAN_POINT ( 'NONE',  ( 75.05402655318509630, 2.143131898507880377E-16, 42.56828755692799859 ) ) ;
#14957 = ORIENTED_EDGE ( 'NONE', *, *, #40873, .T. ) ;
#14958 = CARTESIAN_POINT ( 'NONE',  ( -1.780619886013952602, -1.041246721325602920, 9.886433018048069954 ) ) ;
#14959 = CARTESIAN_POINT ( 'NONE',  ( -208.4459734468149463, 0.000000000000000000, -0.9317124430720247208 ) ) ;
#14960 = CARTESIAN_POINT ( 'NONE',  ( -4.945973446814938335, 0.000000000000000000, 162.5682875569279702 ) ) ;
#14961 = ORIENTED_EDGE ( 'NONE', *, *, #6719, .F. ) ;
#14962 = ORIENTED_EDGE ( 'NONE', *, *, #44762, .T. ) ;
#14963 = FACE_OUTER_BOUND ( 'NONE', #45504, .T. ) ;
#14964 = LINE ( 'NONE', #45971, #32069 ) ;
#14965 = ORIENTED_EDGE ( 'NONE', *, *, #34600, .F. ) ;
#14966 = VERTEX_POINT ( 'NONE', #9340 ) ;
#14967 = LINE ( 'NONE', #23165, #39717 ) ;
#14968 = CARTESIAN_POINT ( 'NONE',  ( 340.0000000000000000, -2.999999999999919176, 171.9999999999998295 ) ) ;
#14969 = ORIENTED_EDGE ( 'NONE', *, *, #23161, .F. ) ;
#14970 = DIRECTION ( 'NONE',  ( -0.000000000000000000, -0.000000000000000000, -1.000000000000000000 ) ) ;
#14971 = EDGE_LOOP ( 'NONE', ( #46730, #2668 ) ) ;
#14972 = AXIS2_PLACEMENT_3D ( 'NONE', #28035, #43422, #12625 ) ;
#14973 = CYLINDRICAL_SURFACE ( 'NONE', #3372, 4.000000000000003553 ) ;
#14974 = FACE_OUTER_BOUND ( 'NONE', #47122, .T. ) ;
#14975 = CARTESIAN_POINT ( 'NONE',  ( 1.249999999999999778, 0.000000000000000000, 3.333333333333333481 ) ) ;
#14976 = ORIENTED_EDGE ( 'NONE', *, *, #23465, .T. ) ;
#14977 = EDGE_LOOP ( 'NONE', ( #36134, #24812, #14805, #5316, #7727, #40850, #31124, #30943, #31752, #10415 ) ) ;
#14978 = AXIS2_PLACEMENT_3D ( 'NONE', #22184, #25780, #30133 ) ;
#14979 = VERTEX_POINT ( 'NONE', #37068 ) ;
#14980 = CARTESIAN_POINT ( 'NONE',  ( 0.000000000000000000, 169.0000000000000000, -342.0000000000001705 ) ) ;
#14981 = VECTOR ( 'NONE', #21295, 1000.000000000000000 ) ;
#14982 = DIRECTION ( 'NONE',  ( 0.000000000000000000, 0.000000000000000000, -1.000000000000000000 ) ) ;
#14983 = ORIENTED_EDGE ( 'NONE', *, *, #38823, .F. ) ;
#14984 = LINE ( 'NONE', #50592, #44445 ) ;
#14985 = ORIENTED_EDGE ( 'NONE', *, *, #49476, .T. ) ;
#14986=STYLED_ITEM('',(#50747),#39060);
#14987 = CARTESIAN_POINT ( 'NONE',  ( -166.6959734468149463, 1.750000000000010214, 40.81828755692798438 ) ) ;
#14988 = EDGE_LOOP ( 'NONE', ( #6893, #42984, #39579, #35556 ) ) ;
#14989 = PLANE ( 'NONE',  #22549 ) ;
#14990 = LINE ( 'NONE', #37363, #38259 ) ;
#14991 = CARTESIAN_POINT ( 'NONE',  ( -114.9999999999987779, 17.00000000000000000, 30.00000000000000000 ) ) ;
#14992 = CARTESIAN_POINT ( 'NONE',  ( 168.9999999999999716, -164.9999999999999432, -356.0000000000001705 ) ) ;
#14993 = EDGE_CURVE ( 'NONE', #18727, #13237, #24998, .T. ) ;
#14994 = ADVANCED_FACE ( 'NONE', ( #29095 ), #17288, .F. ) ;
#14995 = VECTOR ( 'NONE', #28062, 1000.000000000000000 ) ;
#14996 = LINE ( 'NONE', #45746, #13487 ) ;
#14997 = ORIENTED_EDGE ( 'NONE', *, *, #29891, .F. ) ;
#14998 = CARTESIAN_POINT ( 'NONE',  ( -5.670847180967843570, -1.750000000000023981, 79.79316129108087807 ) ) ;
#14999 = CARTESIAN_POINT ( 'NONE',  ( 32.27890028733795447, 1.750000000000009548, -160.2068387089191219 ) ) ;
#15000 = EDGE_CURVE ( 'NONE', #24319, #9357, #13432, .T. ) ;
#15001 = B_SPLINE_SURFACE_WITH_KNOTS ( 'NONE', 3, 3, ( 
 ( #49956, #10750, #11009, #15376 ),
 ( #22551, #46115, #38487, #6398 ),
 ( #18945, #14859, #49710, #42309 ),
 ( #14349, #30510, #34127, #22807 ) ),
 .UNSPECIFIED., .F., .F., .F.,
 ( 4, 4 ),
 ( 4, 4 ),
 ( 0.000000000000000000, 1.000000000000000000 ),
 ( 0.000000000000000000, 1.000000000000000000 ),
 .UNSPECIFIED. ) ;
#15002 = LINE ( 'NONE', #30660, #14620 ) ;
#15003 = CARTESIAN_POINT ( 'NONE',  ( -32.36066692128246558, 7.813306791043033606, 3.199614146704519602 ) ) ;
#15004 = EDGE_CURVE ( 'NONE', #45968, #43076, #33456, .T. ) ;
#15005 = EDGE_CURVE ( 'NONE', #9471, #17930, #5985, .T. ) ;
#15006 = CARTESIAN_POINT ( 'NONE',  ( -17.23491422248386584, 0.5912720620001978844, 8.727788335465566760 ) ) ;
#15007 = CARTESIAN_POINT ( 'NONE',  ( 350.0000000000001137, 165.0000000000000000, 355.9999999999997726 ) ) ;
#15008 = CARTESIAN_POINT ( 'NONE',  ( 9.999999999999998224, 8.486842105263161073, -18.34680996553532140 ) ) ;
#15009 = EDGE_CURVE ( 'NONE', #39423, #45968, #33951, .T. ) ;
#15010 = PLANE ( 'NONE',  #45950 ) ;
#15011 = VERTEX_POINT ( 'NONE', #7515 ) ;
#15012 = CARTESIAN_POINT ( 'NONE',  ( 20.40054609052976531, -26.26366202847973597, -3.760136334089591248 ) ) ;
#15013 = AXIS2_PLACEMENT_3D ( 'NONE', #37682, #26372, #49420 ) ;
#15014 = CARTESIAN_POINT ( 'NONE',  ( 5.551115123125782702E-14, -184.9999999999999716, 343.9999999999997726 ) ) ;
#15015 = CARTESIAN_POINT ( 'NONE',  ( -0.9015506157965548217, 0.9804419706251666922, 9.951893257059996500 ) ) ;
#15016 = AXIS2_PLACEMENT_3D ( 'NONE', #21940, #42184, #37607 ) ;
#15017 = VERTEX_POINT ( 'NONE', #7777 ) ;
#15018 = ORIENTED_EDGE ( 'NONE', *, *, #37508, .T. ) ;
#15019 = DIRECTION ( 'NONE',  ( 1.000000000000000000, -0.000000000000000000, -0.000000000000000000 ) ) ;
#15020 = VECTOR ( 'NONE', #47473, 1000.000000000000000 ) ;
#15021 = FACE_OUTER_BOUND ( 'NONE', #27255, .T. ) ;
#15022 = VERTEX_POINT ( 'NONE', #14956 ) ;
#15023 = AXIS2_PLACEMENT_3D ( 'NONE', #33129, #10010, #13603 ) ;
#15024 = ORIENTED_EDGE ( 'NONE', *, *, #26936, .T. ) ;
#15025 = CARTESIAN_POINT ( 'NONE',  ( 45.64490844644691236, 21.32281559348795952, 8.807470649214879543 ) ) ;
#15026 = CARTESIAN_POINT ( 'NONE',  ( 0.000000000000000000, 0.000000000000000000, 0.000000000000000000 ) ) ;
#15027 = CARTESIAN_POINT ( 'NONE',  ( -165.3973046169136012, -62.56198943095993315, -17.65743994998275213 ) ) ;
#15028 = ORIENTED_EDGE ( 'NONE', *, *, #11274, .F. ) ;
#15029 = EDGE_LOOP ( 'NONE', ( #28045, #20855, #37158, #29392 ) ) ;
#15030 = VERTEX_POINT ( 'NONE', #26498 ) ;
#15031 = EDGE_CURVE ( 'NONE', #49578, #41405, #34988, .T. ) ;
#15032 = CARTESIAN_POINT ( 'NONE',  ( 432.7825420346616170, -77.43746236555679729, -130.5992382549688671 ) ) ;
#15033 = DIRECTION ( 'NONE',  ( -1.000000000000000000, 0.000000000000000000, 0.000000000000000000 ) ) ;
#15034 = ORIENTED_EDGE ( 'NONE', *, *, #45364, .F. ) ;
#15035 = AXIS2_PLACEMENT_3D ( 'NONE', #1617, #36276, #13398 ) ;
#15036 = DIRECTION ( 'NONE',  ( 1.000000000000000000, 0.000000000000000000, 0.000000000000000000 ) ) ;
#15037 = CARTESIAN_POINT ( 'NONE',  ( 33.89193117067290473, 21.24469349090191983, 910.0000000000000000 ) ) ;
#15038 = CARTESIAN_POINT ( 'NONE',  ( -208.1473046169136580, -154.8119894309599260, 472.8425600500171981 ) ) ;
#15039 = ORIENTED_EDGE ( 'NONE', *, *, #37546, .F. ) ;
#15040 = ORIENTED_EDGE ( 'NONE', *, *, #6672, .F. ) ;
#15041 = CARTESIAN_POINT ( 'NONE',  ( 30.00000000000217781, 17.00000000000000000, 95.00000000000000000 ) ) ;
#15042 = CARTESIAN_POINT ( 'NONE',  ( -178.1763882397831082, 74.83106485270566566, -120.5992382549688955 ) ) ;
#15043 = CARTESIAN_POINT ( 'NONE',  ( -239.0000000000000853, -153.6999999999999602, 254.8599999999999852 ) ) ;
#15044 = EDGE_LOOP ( 'NONE', ( #29479, #22470, #7680, #23232, #10777, #9956 ) ) ;
#15045 = VERTEX_POINT ( 'NONE', #22391 ) ;
#15046 = CARTESIAN_POINT ( 'NONE',  ( 46.10908423965007330, 19.89422939639137766, 1.847720168420772691 ) ) ;
#15047 = DIRECTION ( 'NONE',  ( -0.000000000000000000, -0.000000000000000000, -1.000000000000000000 ) ) ;
#15048 = CARTESIAN_POINT ( 'NONE',  ( 166.9999999999999716, 6.000000000000060396, -340.0000000000001137 ) ) ;
#15049 = AXIS2_PLACEMENT_3D ( 'NONE', #1021, #16, #35932 ) ;
#15050 = CARTESIAN_POINT ( 'NONE',  ( -1.782521105131510186, 0.3635605703594341209, 9.903764339332088440 ) ) ;
#15051 = ORIENTED_EDGE ( 'NONE', *, *, #8629, .F. ) ;
#15052 = CARTESIAN_POINT ( 'NONE',  ( 11.73320209285708415, -11.96063479729170886, 9.403735324607438884 ) ) ;
#15053 = AXIS2_PLACEMENT_3D ( 'NONE', #14546, #26095, #46062 ) ;
#15054 = DIRECTION ( 'NONE',  ( -0.000000000000000000, -0.000000000000000000, -1.000000000000000000 ) ) ;
#15055 = CARTESIAN_POINT ( 'NONE',  ( 214.9999999999999432, 173.0000000000000000, 372.0000000000000000 ) ) ;
#15056 = DIRECTION ( 'NONE',  ( 6.765175596986471882E-16, -0.9749645535258953943, 0.2223603367690637489 ) ) ;
#15057 = AXIS2_PLACEMENT_3D ( 'NONE', #20237, #8191, #23840 ) ;
#15058 = LINE ( 'NONE', #39189, #16508 ) ;
#15059 = EDGE_CURVE ( 'NONE', #43076, #22294, #50558, .T. ) ;
#15060 = DIRECTION ( 'NONE',  ( 0.000000000000000000, 0.000000000000000000, 1.000000000000000000 ) ) ;
#15061 = ORIENTED_EDGE ( 'NONE', *, *, #10168, .T. ) ;
#15062 = EDGE_CURVE ( 'NONE', #40502, #46038, #13415, .T. ) ;
#15063 = CARTESIAN_POINT ( 'NONE',  ( 30.25247992116058526, -39.82368563463805344, -3.760136334089591248 ) ) ;
#15064 = DIRECTION ( 'NONE',  ( 1.000000000000000000, 0.000000000000000000, 1.612977847700450206E-50 ) ) ;
#15065 = B_SPLINE_CURVE_WITH_KNOTS ( 'NONE', 3,
 ( #45204, #44713, #10092, #13183 ),
 .UNSPECIFIED., .F., .F.,
 ( 4, 4 ),
 ( 0.9811748202683102660, 0.9878904167554123372 ),
 .UNSPECIFIED. ) ;
#15066 = DIRECTION ( 'NONE',  ( 0.000000000000000000, 6.123233995736766036E-17, -1.000000000000000000 ) ) ;
#15067 =( BOUNDED_CURVE ( )  B_SPLINE_CURVE ( 3, ( #38664, #49644, #6590, #3482 ),
 .UNSPECIFIED., .F., .F. ) 
 B_SPLINE_CURVE_WITH_KNOTS ( ( 4, 4 ),
 ( 1.570796326794890119, 3.141592653589794004 ),
 .UNSPECIFIED. ) 
 CURVE ( )  GEOMETRIC_REPRESENTATION_ITEM ( )  RATIONAL_B_SPLINE_CURVE ( ( 1.000000000000000000, 0.8047378541243632721, 0.8047378541243632721, 1.000000000000000000 ) ) 
 REPRESENTATION_ITEM ( '' )  );
#15068 = ORIENTED_EDGE ( 'NONE', *, *, #31474, .T. ) ;
#15069 = CARTESIAN_POINT ( 'NONE',  ( -568.6915979970481203, 57.49999999999996447, -173.6700166912652890 ) ) ;
#15070 = VECTOR ( 'NONE', #6343, 1000.000000000000000 ) ;
#15071 = CARTESIAN_POINT ( 'NONE',  ( 340.0000000000000568, 181.0000000000000853, 355.9999999999998295 ) ) ;
#15072 = VERTEX_POINT ( 'NONE', #30356 ) ;
#15073 = CARTESIAN_POINT ( 'NONE',  ( -0.3896797354171960270, 1.262193838292709147, 9.943883492372847854 ) ) ;
#15074 = DIRECTION ( 'NONE',  ( 0.000000000000000000, -0.2981428420003837121, -0.9545212652235329776 ) ) ;
#15075 = LINE ( 'NONE', #29714, #27324 ) ;
#15076 = CARTESIAN_POINT ( 'NONE',  ( -5.000000000000000000, 165.2000000000000171, 359.7999999999997840 ) ) ;
#15077 =( BOUNDED_CURVE ( )  B_SPLINE_CURVE ( 3, ( #33607, #49703, #34365, #9993 ),
 .UNSPECIFIED., .F., .F. ) 
 B_SPLINE_CURVE_WITH_KNOTS ( ( 4, 4 ),
 ( 3.141592653589793116, 4.712388980384689674 ),
 .UNSPECIFIED. ) 
 CURVE ( )  GEOMETRIC_REPRESENTATION_ITEM ( )  RATIONAL_B_SPLINE_CURVE ( ( 1.000000000000000000, 0.8047378541243649375, 0.8047378541243649375, 1.000000000000000000 ) ) 
 REPRESENTATION_ITEM ( '' )  );
#15078 = VERTEX_POINT ( 'NONE', #26258 ) ;
#15079 = LINE ( 'NONE', #27140, #20800 ) ;
#15080 = ORIENTED_EDGE ( 'NONE', *, *, #23419, .T. ) ;
#15081 = ORIENTED_EDGE ( 'NONE', *, *, #31353, .T. ) ;
#15082 = CYLINDRICAL_SURFACE ( 'NONE', #60, 1.750000000000001554 ) ;
#15083 = ORIENTED_EDGE ( 'NONE', *, *, #20969, .F. ) ;
#15084 = CARTESIAN_POINT ( 'NONE',  ( 153.2026953830863647, -97.66198943095992036, -17.48025818148969890 ) ) ;
#15085 = CARTESIAN_POINT ( 'NONE',  ( -50.11058929355266400, 7.578863168071933387, 7.455576670931136185 ) ) ;
#15086 = VECTOR ( 'NONE', #47354, 1000.000000000000000 ) ;
#15087 = CARTESIAN_POINT ( 'NONE',  ( 155.0540265531850537, 2.143131898507880377E-16, 165.0000000000000000 ) ) ;
#15088 = VECTOR ( 'NONE', #42330, 1000.000000000000000 ) ;
#15089 =( BOUNDED_CURVE ( )  B_SPLINE_CURVE ( 3, ( #7337, #38649, #19384, #12629 ),
 .UNSPECIFIED., .F., .F. ) 
 B_SPLINE_CURVE_WITH_KNOTS ( ( 4, 4 ),
 ( 1.570796326794896558, 3.141592653589793116 ),
 .UNSPECIFIED. ) 
 CURVE ( )  GEOMETRIC_REPRESENTATION_ITEM ( )  RATIONAL_B_SPLINE_CURVE ( ( 1.000000000000000000, 0.8047378541243649375, 0.8047378541243649375, 1.000000000000000000 ) ) 
 REPRESENTATION_ITEM ( '' )  );
#15090 = CARTESIAN_POINT ( 'NONE',  ( 339.9999999999998863, -164.9999999999999432, 343.9999999999997726 ) ) ;
#15091 = ORIENTED_EDGE ( 'NONE', *, *, #43970, .T. ) ;
#15092 = VECTOR ( 'NONE', #25365, 1000.000000000000000 ) ;
#15093 = EDGE_CURVE ( 'NONE', #12195, #25169, #12258, .T. ) ;
#15094 = CARTESIAN_POINT ( 'NONE',  ( -69.99999999999783995, 17.00000000000000000, 115.0000000000000142 ) ) ;
#15095 = CARTESIAN_POINT ( 'NONE',  ( 114.3291528190321173, -1.749999999999997113, -120.2068387089191219 ) ) ;
#15096 = VERTEX_POINT ( 'NONE', #27003 ) ;
#15097 = CARTESIAN_POINT ( 'NONE',  ( 153.3040265531850537, 1.750000000000010658, 120.8182875569279702 ) ) ;
#15098 = LINE ( 'NONE', #42534, #25330 ) ;
#15099 = ORIENTED_EDGE ( 'NONE', *, *, #30254, .F. ) ;
#15100 = ORIENTED_EDGE ( 'NONE', *, *, #9599, .T. ) ;
#15101 = ORIENTED_EDGE ( 'NONE', *, *, #1454, .F. ) ;
#15102 = CYLINDRICAL_SURFACE ( 'NONE', #26250, 1.750000000000001554 ) ;
#15103 = CARTESIAN_POINT ( 'NONE',  ( 340.0000000000000568, 181.0000000000000284, 339.9999999999997726 ) ) ;
#15104 = PRODUCT_DEFINITION_SHAPE ( 'NONE', 'NONE',  #50740 ) ;
#15105 = ORIENTED_EDGE ( 'NONE', *, *, #49889, .F. ) ;
#15106 = CARTESIAN_POINT ( 'NONE',  ( -0.4277546898749028381, -1.184419892831247711, 9.974012008644017158 ) ) ;
#15107 =( NAMED_UNIT ( * ) SI_UNIT ( $, .STERADIAN. ) SOLID_ANGLE_UNIT ( ) );
#15108 = FACE_BOUND ( 'NONE', #4684, .T. ) ;
#15109 = AXIS2_PLACEMENT_3D ( 'NONE', #18010, #37307, #17775 ) ;
#15110 = FACE_OUTER_BOUND ( 'NONE', #41997, .T. ) ;
#15111 = PLANE ( 'NONE',  #41066 ) ;
#15112 = DIRECTION ( 'NONE',  ( -0.000000000000000000, -1.000000000000000000, -0.000000000000000000 ) ) ;
#15113 = CARTESIAN_POINT ( 'NONE',  ( 113.3040265531850537, -1.749999999999997113, -39.18171244307202983 ) ) ;
#15114 = CARTESIAN_POINT ( 'NONE',  ( -124.9459734468149463, 2.143131898507847836E-16, 165.0000000000000000 ) ) ;
#15115 = FACE_OUTER_BOUND ( 'NONE', #47670, .T. ) ;
#15116 = CARTESIAN_POINT ( 'NONE',  ( -5.888214538810513154, -16.20866436362413410, 8.727788335465566760 ) ) ;
#15117 = ORIENTED_EDGE ( 'NONE', *, *, #3554, .T. ) ;
#15118 = PLANE ( 'NONE',  #12597 ) ;
#15119 = LINE ( 'NONE', #23061, #16767 ) ;
#15120 = LINE ( 'NONE', #18701, #32249 ) ;
#15121 = ORIENTED_EDGE ( 'NONE', *, *, #22998, .F. ) ;
#15122 = CARTESIAN_POINT ( 'NONE',  ( 1.057156451998911839, -0.7920882637786250680, 9.943883492372851407 ) ) ;
#15123 = EDGE_CURVE ( 'NONE', #10108, #43146, #42627, .T. ) ;
#15124 = LINE ( 'NONE', #3829, #22903 ) ;
#15125 = CARTESIAN_POINT ( 'NONE',  ( 16.69947034530964913, -2.312583065866261389, 2.590526750877053086 ) ) ;
#15126 = LINE ( 'NONE', #4092, #48720 ) ;
#15127 = CARTESIAN_POINT ( 'NONE',  ( -19.99999999999784706, 17.00000000000000000, 115.0000000000000142 ) ) ;
#15128 = ORIENTED_EDGE ( 'NONE', *, *, #17355, .T. ) ;
#15129 = CARTESIAN_POINT ( 'NONE',  ( -47.72109971266203132, -1.750000000000010214, 121.8434138227750623 ) ) ;
#15130 = ORIENTED_EDGE ( 'NONE', *, *, #11507, .T. ) ;
#15131 = CARTESIAN_POINT ( 'NONE',  ( 195.0540265531851105, -1.025126265847089435, 39.06828755692797728 ) ) ;
#15132 = VERTEX_POINT ( 'NONE', #38827 ) ;
#15133 = CARTESIAN_POINT ( 'NONE',  ( 341.6568542494922553, -185.0000000000001705, -360.0000000000003411 ) ) ;
#15135 = EDGE_CURVE ( 'NONE', #43286, #14525, #42135, .T. ) ;
#15134 = CARTESIAN_POINT ( 'NONE',  ( -124.9459734468149605, 0.000000000000000000, 162.5682875569279702 ) ) ;
#15136 = ADVANCED_FACE ( 'NONE', ( #10843 ), #22644, .F. ) ;
#15137 = ORIENTED_EDGE ( 'NONE', *, *, #26583, .F. ) ;
#15138 = SURFACE_STYLE_FILL_AREA ( #50229 ) ;
#15139 = VERTEX_POINT ( 'NONE', #34729 ) ;
#15140 = EDGE_CURVE ( 'NONE', #18077, #9162, #44553, .T. ) ;
#15141 = EDGE_CURVE ( 'NONE', #21498, #30616, #14445, .T. ) ;
#15142 = VECTOR ( 'NONE', #39884, 1000.000000000000000 ) ;
#15143 = VERTEX_POINT ( 'NONE', #19300 ) ;
#15144 = CARTESIAN_POINT ( 'NONE',  ( 193.3040265531851105, 1.750000000000010658, 80.81828755692798438 ) ) ;
#15145 = FACE_OUTER_BOUND ( 'NONE', #18684, .T. ) ;
#15146 = AXIS2_PLACEMENT_3D ( 'NONE', #16772, #1632, #32432 ) ;
#15147 = ORIENTED_EDGE ( 'NONE', *, *, #20337, .T. ) ;
#15148 = DIRECTION ( 'NONE',  ( 0.000000000000000000, 0.000000000000000000, 1.000000000000000000 ) ) ;
#15149 = CARTESIAN_POINT ( 'NONE',  ( -86.69597344681494633, -1.750000000000010658, -119.1817124430720440 ) ) ;
#15150 = CARTESIAN_POINT ( 'NONE',  ( -14.99999999999845812, 16.00000000000000000, 35.00000000000000000 ) ) ;
#15151 = ORIENTED_EDGE ( 'NONE', *, *, #31834, .F. ) ;
#15153 = ORIENTED_EDGE ( 'NONE', *, *, #9502, .T. ) ;
#15152 = ADVANCED_FACE ( 'NONE', ( #41894 ), #11615, .F. ) ;
#15154 = LINE ( 'NONE', #15411, #16085 ) ;
#15155 = EDGE_CURVE ( 'NONE', #19177, #34969, #32476, .T. ) ;
#15156 = FACE_OUTER_BOUND ( 'NONE', #48343, .T. ) ;
#15157 = EDGE_CURVE ( 'NONE', #2566, #15989, #27269, .T. ) ;
#15158 = EDGE_CURVE ( 'NONE', #14871, #19563, #4947, .T. ) ;
#15159 = ORIENTED_EDGE ( 'NONE', *, *, #113, .T. ) ;
#15160 = CARTESIAN_POINT ( 'NONE',  ( 210.0000000000000568, 0.000000000000000000, 40.81828755692798438 ) ) ;
#15161 = VECTOR ( 'NONE', #1643, 1000.000000000000000 ) ;
#15162 = CARTESIAN_POINT ( 'NONE',  ( -21.60170755165869849, 30.69732439037094807, -6.568693074176340296 ) ) ;
#15163 = ORIENTED_EDGE ( 'NONE', *, *, #46826, .T. ) ;
#15164 = CARTESIAN_POINT ( 'NONE',  ( 1.211050186583219279, 0.5544523570010763125, 9.951893257060014264 ) ) ;
#15165 = CARTESIAN_POINT ( 'NONE',  ( -6.695973446814940111, -1.750000000000024203, 80.81828755692798438 ) ) ;
#15166 = VERTEX_POINT ( 'NONE', #8278 ) ;
#15167 = AXIS2_PLACEMENT_3D ( 'NONE', #27357, #42993, #7872 ) ;
#15168 = DIRECTION ( 'NONE',  ( -0.000000000000000000, -0.000000000000000000, -1.000000000000000000 ) ) ;
#15169 = DIRECTION ( 'NONE',  ( -0.000000000000000000, -1.000000000000000000, -0.000000000000000000 ) ) ;
#15170 = DIRECTION ( 'NONE',  ( -0.000000000000000000, -0.000000000000000000, 1.000000000000000000 ) ) ;
#15171 = CARTESIAN_POINT ( 'NONE',  ( 5.551115123125782702E-14, -164.9999999999999432, 343.9999999999997726 ) ) ;
#15172 = ORIENTED_EDGE ( 'NONE', *, *, #43493, .F. ) ;
#15173 =( BOUNDED_CURVE ( )  B_SPLINE_CURVE ( 3, ( #30519, #45633, #34897, #35153 ),
 .UNSPECIFIED., .F., .F. ) 
 B_SPLINE_CURVE_WITH_KNOTS ( ( 4, 4 ),
 ( 3.141592653589793116, 4.712388980384689674 ),
 .UNSPECIFIED. ) 
 CURVE ( )  GEOMETRIC_REPRESENTATION_ITEM ( )  RATIONAL_B_SPLINE_CURVE ( ( 1.000000000000000000, 0.8047378541243649375, 0.8047378541243649375, 1.000000000000000000 ) ) 
 REPRESENTATION_ITEM ( '' )  );
#15174 = CARTESIAN_POINT ( 'NONE',  ( 5.551115123125782702E-14, -180.9999999999999716, 355.9999999999997726 ) ) ;
#15175 = DIRECTION ( 'NONE',  ( 1.132880637372608740E-16, 4.718402560806925739E-50, 1.000000000000000000 ) ) ;
#15176 = CARTESIAN_POINT ( 'NONE',  ( 1.011271242968677653, 0.7347315653656002477, 10.00000000000000000 ) ) ;
#15177 = VERTEX_POINT ( 'NONE', #11869 ) ;
#15178 = ADVANCED_FACE ( 'NONE', ( #21264 ), #23916, .T. ) ;
#15179 = ORIENTED_EDGE ( 'NONE', *, *, #767, .F. ) ;
#15180 = DIRECTION ( 'NONE',  ( 0.1896243834332324574, 1.304512053934558935E-14, 0.9818567070645116690 ) ) ;
#15181 = LINE ( 'NONE', #11330, #31903 ) ;
#15182 = CARTESIAN_POINT ( 'NONE',  ( 340.0000000000000000, -166.6568542494923406, 341.6568542494921985 ) ) ;
#15183 = VECTOR ( 'NONE', #24054, 1000.000000000000000 ) ;
#15184 = EDGE_CURVE ( 'NONE', #45555, #3395, #13554, .T. ) ;
#15185 = ADVANCED_FACE ( 'NONE', ( #33084 ), #47230, .F. ) ;
#15186 = CARTESIAN_POINT ( 'NONE',  ( 183.0000000000000000, -5.999999999999950262, -350.0000000000001705 ) ) ;
#15187 = CARTESIAN_POINT ( 'NONE',  ( -1.721971274562257515, -0.09408549481333014497, 9.928159647716187308 ) ) ;
#15188 = VECTOR ( 'NONE', #20421, 1000.000000000000000 ) ;
#15189 = CARTESIAN_POINT ( 'NONE',  ( -167.7210997126620384, -1.750000000000010214, -120.2068387089191219 ) ) ;
#15190 = ORIENTED_EDGE ( 'NONE', *, *, #31343, .T. ) ;
#15191 = CARTESIAN_POINT ( 'NONE',  ( 168.9999999999999716, -81.49999999999997158, -350.0000000000001705 ) ) ;
#15192 = EDGE_CURVE ( 'NONE', #30683, #36281, #8531, .T. ) ;
#15193 = AXIS2_PLACEMENT_3D ( 'NONE', #46442, #12334, #34962 ) ;
#15194 = LINE ( 'NONE', #50027, #21212 ) ;
#15195 = FACE_OUTER_BOUND ( 'NONE', #22326, .T. ) ;
#15196 = EDGE_CURVE ( 'NONE', #35891, #9839, #31886, .T. ) ;
#15197 = AXIS2_PLACEMENT_3D ( 'NONE', #44693, #21616, #40866 ) ;
#15198 = CARTESIAN_POINT ( 'NONE',  ( -167.7210997126620384, 1.750000000000009548, 81.84341382277507648 ) ) ;
#15199 = ORIENTED_EDGE ( 'NONE', *, *, #5224, .T. ) ;
#15200 = AXIS2_PLACEMENT_3D ( 'NONE', #39879, #24217, #1121 ) ;
#15201 = CYLINDRICAL_SURFACE ( 'NONE', #8949, 1.750000000000008438 ) ;
#15202 = AXIS2_PLACEMENT_3D ( 'NONE', #1544, #44111, #24644 ) ;
#15203 = CARTESIAN_POINT ( 'NONE',  ( 23.82716369509147825, 44.49195112876006419, 8.356839323120299312 ) ) ;
#15204 = ORIENTED_EDGE ( 'NONE', *, *, #44013, .F. ) ;
#15205 = CARTESIAN_POINT ( 'NONE',  ( -119.9999999999981668, 16.00000000000000000, 65.00000000000000000 ) ) ;
#15206 = PLANE ( 'NONE',  #27400 ) ;
#15207 = DIRECTION ( 'NONE',  ( 0.000000000000000000, 0.000000000000000000, 1.000000000000000000 ) ) ;
#15208 = CIRCLE ( 'NONE', #27481, 2.000000000000001776 ) ;
#15209 = VERTEX_POINT ( 'NONE', #31381 ) ;
#15210 = CARTESIAN_POINT ( 'NONE',  ( 153.3040265531850537, 0.000000000000000000, 165.0000000000000000 ) ) ;
#15211 = CARTESIAN_POINT ( 'NONE',  ( 35.05402655318504657, 2.143131898507880377E-16, -40.93171244307205825 ) ) ;
#15212 = ORIENTED_EDGE ( 'NONE', *, *, #14715, .F. ) ;
#15213 = CARTESIAN_POINT ( 'NONE',  ( 4.256388337216338691, -5.377297509087402005, 9.753789706659947711 ) ) ;
#15214 = EDGE_CURVE ( 'NONE', #26234, #325, #44837, .T. ) ;
#15215 = LINE ( 'NONE', #34468, #10638 ) ;
#15216 = UNCERTAINTY_MEASURE_WITH_UNIT (LENGTH_MEASURE( 1.000000000000000082E-05 ), #32165, 'distance_accuracy_value', 'NONE');
#15217 = CYLINDRICAL_SURFACE ( 'NONE', #26684, 3.749999999999975575 ) ;
#15218 = EDGE_LOOP ( 'NONE', ( #15081, #25236, #9057, #13053 ) ) ;
#15219 = ORIENTED_EDGE ( 'NONE', *, *, #43976, .T. ) ;
#15220 = ADVANCED_FACE ( 'NONE', ( #16224 ), #16480, .T. ) ;
#15221 = CARTESIAN_POINT ( 'NONE',  ( 0.000000000000000000, -164.9999999999999716, 0.000000000000000000 ) ) ;
#15222 = EDGE_CURVE ( 'NONE', #21391, #30988, #19806, .T. ) ;
#15223 = VECTOR ( 'NONE', #45712, 1000.000000000000000 ) ;
#15224 = EDGE_CURVE ( 'NONE', #20342, #41044, #8259, .T. ) ;
#15225 = ORIENTED_EDGE ( 'NONE', *, *, #5254, .T. ) ;
#15226 = EDGE_LOOP ( 'NONE', ( #47289, #47976, #4923, #24887 ) ) ;
#15227 = DIRECTION ( 'NONE',  ( -0.000000000000000000, -0.000000000000000000, -1.000000000000000000 ) ) ;
#15228 = DIRECTION ( 'NONE',  ( 0.000000000000000000, 0.000000000000000000, -1.000000000000000000 ) ) ;
#15229 = FACE_OUTER_BOUND ( 'NONE', #25610, .T. ) ;
#15230 = ORIENTED_EDGE ( 'NONE', *, *, #14270, .T. ) ;
#15231 = B_SPLINE_CURVE_WITH_KNOTS ( 'NONE', 3,
 ( #15904, #16398, #20253, #43337 ),
 .UNSPECIFIED., .F., .F.,
 ( 4, 4 ),
 ( 0.000000000000000000, 0.0001252128669263171171 ),
 .UNSPECIFIED. ) ;
#15232 = LINE ( 'NONE', #38082, #39907 ) ;
#15233 = EDGE_CURVE ( 'NONE', #32189, #33102, #47481, .T. ) ;
#15234 = ORIENTED_EDGE ( 'NONE', *, *, #38076, .T. ) ;
#15235 = EDGE_CURVE ( 'NONE', #13105, #31434, #48663, .T. ) ;
#15236 = VECTOR ( 'NONE', #18451, 1000.000000000000000 ) ;
#15237 = CARTESIAN_POINT ( 'NONE',  ( 0.000000000000000000, 183.0000000000000284, 355.9999999999997726 ) ) ;
#15238 = DIRECTION ( 'NONE',  ( -1.000000000000000000, 0.000000000000000000, 0.000000000000000000 ) ) ;
#15239 =( BOUNDED_CURVE ( )  B_SPLINE_CURVE ( 3, ( #7017, #31133, #30624, #22659 ),
 .UNSPECIFIED., .F., .F. ) 
 B_SPLINE_CURVE_WITH_KNOTS ( ( 4, 4 ),
 ( 4.712388980384676351, 6.283185307179586232 ),
 .UNSPECIFIED. ) 
 CURVE ( )  GEOMETRIC_REPRESENTATION_ITEM ( )  RATIONAL_B_SPLINE_CURVE ( ( 1.000000000000000000, 0.8047378541243618288, 0.8047378541243618288, 1.000000000000000000 ) ) 
 REPRESENTATION_ITEM ( '' )  );
#15241 = AXIS2_PLACEMENT_3D ( 'NONE', #11754, #49930, #47105 ) ;
#15240 = CARTESIAN_POINT ( 'NONE',  ( 339.9999999999999432, -180.9999999999999716, -340.0000000000001705 ) ) ;
#15242 = ORIENTED_EDGE ( 'NONE', *, *, #11243, .F. ) ;
#15243 = ORIENTED_EDGE ( 'NONE', *, *, #31140, .F. ) ;
#15244 = ORIENTED_EDGE ( 'NONE', *, *, #10175, .F. ) ;
#15245 = CARTESIAN_POINT ( 'NONE',  ( 1.011271242968683648, 0.7347315653655930312, 9.972675548442463622 ) ) ;
#15246 =( BOUNDED_CURVE ( )  B_SPLINE_CURVE ( 3, ( #30924, #46508, #27313, #23467 ),
 .UNSPECIFIED., .F., .F. ) 
 B_SPLINE_CURVE_WITH_KNOTS ( ( 4, 4 ),
 ( 0.000000000000000000, 1.570796326794896558 ),
 .UNSPECIFIED. ) 
 CURVE ( )  GEOMETRIC_REPRESENTATION_ITEM ( )  RATIONAL_B_SPLINE_CURVE ( ( 1.000000000000000000, 0.8047378541243649375, 0.8047378541243649375, 1.000000000000000000 ) ) 
 REPRESENTATION_ITEM ( '' )  );
#15247 = CARTESIAN_POINT ( 'NONE',  ( -164.9459734468149463, 2.143131898507880377E-16, -40.93171244307202983 ) ) ;
#15248 = ORIENTED_EDGE ( 'NONE', *, *, #13997, .F. ) ;
#15249 = CARTESIAN_POINT ( 'NONE',  ( 35.05402655318504657, 1.025126265847089879, 122.5682875569280128 ) ) ;
#15250 = EDGE_LOOP ( 'NONE', ( #27785, #49305, #6558, #29210 ) ) ;
#15251 = VECTOR ( 'NONE', #43787, 1000.000000000000000 ) ;
#15252 = CYLINDRICAL_SURFACE ( 'NONE', #38956, 1.750000000000015543 ) ;
#15253 = ORIENTED_EDGE ( 'NONE', *, *, #25881, .T. ) ;
#15254 = SHAPE_REPRESENTATION_RELATIONSHIP ( 'NONE' , 'NONE' ,  #15926, #24018 ) ;
#15255 = CARTESIAN_POINT ( 'NONE',  ( 360.0000000000000000, 183.3431457505076310, -358.3431457505078015 ) ) ;
#15256 = CARTESIAN_POINT ( 'NONE',  ( -48.99656738986512039, 11.00747004110376182, 1.847720168420772691 ) ) ;
#15257 = CARTESIAN_POINT ( 'NONE',  ( -42.99990394833793061, 47.95759300784327905, 5.000000000000000000 ) ) ;
#15258 = EDGE_CURVE ( 'NONE', #24669, #39173, #35305, .T. ) ;
#15259 = DIRECTION ( 'NONE',  ( 0.000000000000000000, -2.969158215481698263E-48, 1.000000000000000000 ) ) ;
#15260 = ORIENTED_EDGE ( 'NONE', *, *, #26518, .F. ) ;
#15261 = EDGE_LOOP ( 'NONE', ( #28116, #7187, #706, #8824 ) ) ;
#15262 = CARTESIAN_POINT ( 'NONE',  ( -31.44259251615275019, -38.95901822126145220, -9.367992836599951190 ) ) ;
#15263 = LINE ( 'NONE', #9006, #49398 ) ;
#15264 = LINE ( 'NONE', #15754, #22826 ) ;
#15265 = DIRECTION ( 'NONE',  ( 1.000000000000000000, 0.000000000000000000, 0.000000000000000000 ) ) ;
#15266 = B_SPLINE_CURVE_WITH_KNOTS ( 'NONE', 3,
 ( #49740, #22592, #14639, #38274 ),
 .UNSPECIFIED., .F., .F.,
 ( 4, 4 ),
 ( 0.002800684175189303935, 0.008939195511151335274 ),
 .UNSPECIFIED. ) ;
#15267 = VECTOR ( 'NONE', #19114, 1000.000000000000000 ) ;
#15268 = FACE_OUTER_BOUND ( 'NONE', #32284, .T. ) ;
#15269 = VECTOR ( 'NONE', #40040, 1000.000000000000000 ) ;
#15270 = DIRECTION ( 'NONE',  ( 0.000000000000000000, -2.969158215481698263E-48, 1.000000000000000000 ) ) ;
#15271 = ORIENTED_EDGE ( 'NONE', *, *, #4927, .T. ) ;
#15272 = EDGE_CURVE ( 'NONE', #8483, #41468, #25260, .T. ) ;
#15273 = LINE ( 'NONE', #34260, #20484 ) ;
#15274 = DIRECTION ( 'NONE',  ( -0.8637789008984334549, 0.000000000000000000, 0.5038710255240862468 ) ) ;
#15275 = ORIENTED_EDGE ( 'NONE', *, *, #30006, .T. ) ;
#15276 = AXIS2_PLACEMENT_3D ( 'NONE', #40107, #35322, #155 ) ;
#15277 = CARTESIAN_POINT ( 'NONE',  ( -164.9459734468149463, -1.025126265847089213, 42.56828755692799149 ) ) ;
#15278 = EDGE_CURVE ( 'NONE', #16638, #11677, #40084, .T. ) ;
#15279 = CARTESIAN_POINT ( 'NONE',  ( -8.831420117243776957, -14.12636088103186260, -3.546734833711462365 ) ) ;
#15280 = LINE ( 'NONE', #11176, #14328 ) ;
#15281 = ORIENTED_EDGE ( 'NONE', *, *, #2030, .T. ) ;
#15282 = B_SPLINE_CURVE_WITH_KNOTS ( 'NONE', 3,
 ( #9745, #45377, #2302, #30268 ),
 .UNSPECIFIED., .F., .F.,
 ( 4, 4 ),
 ( 0.000000000000000000, 0.0002520763768916076618 ),
 .UNSPECIFIED. ) ;
#15283 = ORIENTED_EDGE ( 'NONE', *, *, #50324, .F. ) ;
#15284 = DIRECTION ( 'NONE',  ( 0.000000000000000000, 0.000000000000000000, 1.000000000000000000 ) ) ;
#15285 = VECTOR ( 'NONE', #23430, 1000.000000000000000 ) ;
#15286 = CARTESIAN_POINT ( 'NONE',  ( 6.875132362119187768, -50.00000000000000711, 8.356839323120299312 ) ) ;
#15287 = EDGE_CURVE ( 'NONE', #26090, #35055, #7893, .T. ) ;
#15288 = EDGE_CURVE ( 'NONE', #21333, #42541, #2496, .T. ) ;
#15289 = EDGE_LOOP ( 'NONE', ( #29180, #22535, #12868, #18541 ) ) ;
#15290 = ORIENTED_EDGE ( 'NONE', *, *, #19615, .F. ) ;
#15291 = CARTESIAN_POINT ( 'NONE',  ( 29.39982726364966581, 16.78152490921169360, 8.356839323120299312 ) ) ;
#15292 = DIRECTION ( 'NONE',  ( 1.586032892321652482E-16, 0.000000000000000000, 1.000000000000000000 ) ) ;
#15293 = CARTESIAN_POINT ( 'NONE',  ( 0.4166666666666669072, 0.000000000000000000, 10.00000000000000000 ) ) ;
#15294 = ORIENTED_EDGE ( 'NONE', *, *, #17702, .T. ) ;
#15295 = ORIENTED_EDGE ( 'NONE', *, *, #19588, .T. ) ;
#15296 = ORIENTED_EDGE ( 'NONE', *, *, #39850, .F. ) ;
#15297 = EDGE_CURVE ( 'NONE', #30636, #20701, #834, .T. ) ;
#15298 = ADVANCED_FACE ( 'NONE', ( #5865 ), #25878, .F. ) ;
#15299 = LINE ( 'NONE', #11193, #7018 ) ;
#15300 = EDGE_CURVE ( 'NONE', #9732, #29784, #20368, .T. ) ;
#15301 = CARTESIAN_POINT ( 'NONE',  ( -10.00000000000000355, -34.54492135858216528, 0.000000000000000000 ) ) ;
#15302 = ORIENTED_EDGE ( 'NONE', *, *, #47892, .T. ) ;
#15303 = FACE_BOUND ( 'NONE', #38855, .T. ) ;
#15304 = AXIS2_PLACEMENT_3D ( 'NONE', #21973, #29671, #22228 ) ;
#15305 = CARTESIAN_POINT ( 'NONE',  ( 0.000000000000000000, 17.00000000000000000, 0.000000000000000000 ) ) ;
#15306 = CARTESIAN_POINT ( 'NONE',  ( 0.000000000000000000, -164.9999999999999432, -356.0000000000002274 ) ) ;
#15307 = EDGE_LOOP ( 'NONE', ( #36680, #18248, #24798, #49353 ) ) ;
#15308=STYLED_ITEM('',(#50747),#21149);
#15309 = ORIENTED_EDGE ( 'NONE', *, *, #29481, .F. ) ;
#15310 = DIRECTION ( 'NONE',  ( -1.586032892321652236E-16, -1.000000000000000000, -2.288264760618012091E-48 ) ) ;
#15311 = LINE ( 'NONE', #16063, #30878 ) ;
#15312 = EDGE_CURVE ( 'NONE', #8581, #5103, #37716, .T. ) ;
#15313 = CARTESIAN_POINT ( 'NONE',  ( -6.695973446814940111, -1.750000000000024203, 120.8182875569279702 ) ) ;
#15314 = ORIENTED_EDGE ( 'NONE', *, *, #3941, .T. ) ;
#15315 = ORIENTED_EDGE ( 'NONE', *, *, #172, .F. ) ;
#15316 = CARTESIAN_POINT ( 'NONE',  ( 28.96803024440893992, 18.11533787072037072, 7.455576670931136185 ) ) ;
#15317 =( LENGTH_UNIT ( ) NAMED_UNIT ( * ) SI_UNIT ( .MILLI., .METRE. ) );
#15318 = CARTESIAN_POINT ( 'NONE',  ( 115.0540265531850395, 1.025126265847081886, 39.06828755692799149 ) ) ;
#15319 = CARTESIAN_POINT ( 'NONE',  ( 14.49999999999999822, -46.51315789473684248, -6.315789473684215949 ) ) ;
#15320 = CARTESIAN_POINT ( 'NONE',  ( 183.0000000000000284, -9.999999999999953815, -111.0000000000001563 ) ) ;
#15321 = CARTESIAN_POINT ( 'NONE',  ( 151.5540265531850537, 0.000000000000000000, -40.93171244307202983 ) ) ;
#15322 = VERTEX_POINT ( 'NONE', #49919 ) ;
#15323 = LINE ( 'NONE', #27814, #29117 ) ;
#15324 = CARTESIAN_POINT ( 'NONE',  ( 2.097937730060976946, -0.2450639578954889597, 9.884520316594379352 ) ) ;
#15325 = DIRECTION ( 'NONE',  ( 0.000000000000000000, 1.000000000000000000, 0.000000000000000000 ) ) ;
#15326 = LINE ( 'NONE', #19146, #11334 ) ;
#15327 = AXIS2_PLACEMENT_3D ( 'NONE', #22661, #3409, #41914 ) ;
#15328 = CARTESIAN_POINT ( 'NONE',  ( 48.55374341718673747, 12.37034209168268006, -8.917361510505369182 ) ) ;
#15329 = ORIENTED_EDGE ( 'NONE', *, *, #5278, .F. ) ;
#15330 = DIRECTION ( 'NONE',  ( -1.000000000000000000, 0.000000000000000000, 0.000000000000000000 ) ) ;
#15331 = LINE ( 'NONE', #30986, #9464 ) ;
#15332 = CARTESIAN_POINT ( 'NONE',  ( 152.2789002873379900, 1.750000000000009548, 39.79316129108089228 ) ) ;
#15333 = EDGE_CURVE ( 'NONE', #43762, #33571, #2915, .T. ) ;
#15334 = ORIENTED_EDGE ( 'NONE', *, *, #27169, .T. ) ;
#15335 =( LENGTH_UNIT ( ) NAMED_UNIT ( * ) SI_UNIT ( .MILLI., .METRE. ) );
#15336 = CARTESIAN_POINT ( 'NONE',  ( 155.0540265531850537, 2.143131898507880377E-16, -37.43171244307205825 ) ) ;
#15337 = EDGE_LOOP ( 'NONE', ( #8830, #6810, #28998, #7152 ) ) ;
#15338 = DIRECTION ( 'NONE',  ( 0.000000000000000000, 0.000000000000000000, 1.000000000000000000 ) ) ;
#15339 = LINE ( 'NONE', #8837, #29568 ) ;
#15340 = DIRECTION ( 'NONE',  ( -1.000000000000000000, -0.000000000000000000, -0.000000000000000000 ) ) ;
#15341 = CARTESIAN_POINT ( 'NONE',  ( -0.9602803029231570253, 0.8490247040095960651, 9.976582533991679824 ) ) ;
#15342 = EDGE_LOOP ( 'NONE', ( #7217, #33937, #31956, #32975 ) ) ;
#15343 = DIRECTION ( 'NONE',  ( -1.000000000000000000, -0.000000000000000000, -0.000000000000000000 ) ) ;
#15344 = VERTEX_POINT ( 'NONE', #18663 ) ;
#15345 = VERTEX_POINT ( 'NONE', #37947 ) ;
#15346 = CARTESIAN_POINT ( 'NONE',  ( -87.72109971266203843, -1.750000000000009548, -40.20683870891912193 ) ) ;
#15347 = ADVANCED_FACE ( 'NONE', ( #14057 ), #10224, .T. ) ;
#15348 = EDGE_CURVE ( 'NONE', #34745, #41862, #9710, .T. ) ;
#15349 = ORIENTED_EDGE ( 'NONE', *, *, #31088, .T. ) ;
#15350 = CARTESIAN_POINT ( 'NONE',  ( 14.49999999999999822, -46.01315789473684248, 5.916985404131816395 ) ) ;
#15351 = LINE ( 'NONE', #19174, #36826 ) ;
#15352 = CARTESIAN_POINT ( 'NONE',  ( -64.99999999999971578, 17.00000000000000000, -60.00000000000000000 ) ) ;
#15353 = ORIENTED_EDGE ( 'NONE', *, *, #6051, .T. ) ;
#15355 = ADVANCED_FACE ( 'NONE', ( #38205 ), #45088, .T. ) ;
#15354 = CARTESIAN_POINT ( 'NONE',  ( -126.6959734468149321, -1.749999999999996891, -159.1817124430720298 ) ) ;
#15356 = DIRECTION ( 'NONE',  ( 0.000000000000000000, 1.000000000000000000, 0.000000000000000000 ) ) ;
#15357 = ADVANCED_FACE ( 'NONE', ( #21769, #14824 ), #13799, .F. ) ;
#15358 = CARTESIAN_POINT ( 'NONE',  ( 115.0540265531850395, 1.025126265847081664, 159.0682875569279418 ) ) ;
#15359 = ORIENTED_EDGE ( 'NONE', *, *, #33357, .T. ) ;
#15360 = FACE_OUTER_BOUND ( 'NONE', #44646, .T. ) ;
#15361 = CARTESIAN_POINT ( 'NONE',  ( 166.9999999999999716, -256.4999999999999432, -339.9999999999998863 ) ) ;
#15362 = ORIENTED_EDGE ( 'NONE', *, *, #12222, .F. ) ;
#15363 = ORIENTED_EDGE ( 'NONE', *, *, #14240, .T. ) ;
#15364 = EDGE_LOOP ( 'NONE', ( #33220, #46533, #44468, #45318, #42478 ) ) ;
#15365 = DIRECTION ( 'NONE',  ( -0.000000000000000000, -0.000000000000000000, -1.000000000000000000 ) ) ;
#15366 = EDGE_CURVE ( 'NONE', #22529, #16567, #3014, .T. ) ;
#15367 = DIRECTION ( 'NONE',  ( -1.000000000000000000, 0.000000000000000000, 0.000000000000000000 ) ) ;
#15368 = ORIENTED_EDGE ( 'NONE', *, *, #24684, .F. ) ;
#15369 = DIRECTION ( 'NONE',  ( 0.2599384441937727663, -0.8000082703740916124, 0.5407575913134972101 ) ) ;
#15370 = DIRECTION ( 'NONE',  ( -1.000000000000000000, 0.000000000000000000, 0.000000000000000000 ) ) ;
#15371 = SPHERICAL_SURFACE ( 'NONE', #18599, 0.5000000000000000000 ) ;
#15372 = CARTESIAN_POINT ( 'NONE',  ( 0.7769635690559215657, 0.3027738231833606020, 9.985671796968913938 ) ) ;
#15373 = VECTOR ( 'NONE', #41169, 1000.000000000000000 ) ;
#15374 = CARTESIAN_POINT ( 'NONE',  ( 9.999999999999998224, 1.843143693225357538E-15, 8.340239149798797769 ) ) ;
#15375 = CARTESIAN_POINT ( 'NONE',  ( -208.4459734468148611, 1.025126265847089435, 39.06828755692797728 ) ) ;
#15376 = CARTESIAN_POINT ( 'NONE',  ( -1.011271242968677875, -0.7347315653656004697, -10.00000000000000000 ) ) ;
#15377 = CARTESIAN_POINT ( 'NONE',  ( 33.30402655318503946, -1.750000000000009992, -159.1817124430720298 ) ) ;
#15378 = DIRECTION ( 'NONE',  ( 1.000000000000000000, 0.000000000000000000, 0.000000000000000000 ) ) ;
#15379 = ORIENTED_EDGE ( 'NONE', *, *, #40435, .F. ) ;
#15380 = DIRECTION ( 'NONE',  ( 0.000000000000000000, -0.000000000000000000, 1.000000000000000000 ) ) ;
#15381 =( BOUNDED_CURVE ( )  B_SPLINE_CURVE ( 3, ( #33591, #14069, #41528, #22022 ),
 .UNSPECIFIED., .F., .F. ) 
 B_SPLINE_CURVE_WITH_KNOTS ( ( 4, 4 ),
 ( 3.141592653589793560, 4.712388980384745629 ),
 .UNSPECIFIED. ) 
 CURVE ( )  GEOMETRIC_REPRESENTATION_ITEM ( )  RATIONAL_B_SPLINE_CURVE ( ( 1.000000000000000000, 0.8047378541243519479, 0.8047378541243519479, 1.000000000000000000 ) ) 
 REPRESENTATION_ITEM ( '' )  );
#15382 = CARTESIAN_POINT ( 'NONE',  ( -1.642172164747307761, 0.000000000000000000, 0.000000000000000000 ) ) ;
#15383 = DIRECTION ( 'NONE',  ( 0.000000000000000000, -1.000000000000000000, -3.186989995019654210E-49 ) ) ;
#15384 = LINE ( 'NONE', #27688, #10082 ) ;
#15385 = ORIENTED_EDGE ( 'NONE', *, *, #7571, .T. ) ;
#15386 = CARTESIAN_POINT ( 'NONE',  ( -177.4999999999999716, -72.50000000000001421, -9.999999999999973355 ) ) ;
#15387 = CARTESIAN_POINT ( 'NONE',  ( -165.0000000000000284, 16.00000000000000000, 115.0000000000000142 ) ) ;
#15388 =( BOUNDED_CURVE ( )  B_SPLINE_CURVE ( 3, ( #5579, #36411, #28445, #20992 ),
 .UNSPECIFIED., .F., .F. ) 
 B_SPLINE_CURVE_WITH_KNOTS ( ( 4, 4 ),
 ( 3.141592653589793116, 4.712388980384689674 ),
 .UNSPECIFIED. ) 
 CURVE ( )  GEOMETRIC_REPRESENTATION_ITEM ( )  RATIONAL_B_SPLINE_CURVE ( ( 1.000000000000000000, 0.8047378541243649375, 0.8047378541243649375, 1.000000000000000000 ) ) 
 REPRESENTATION_ITEM ( '' )  );
#15389 = CARTESIAN_POINT ( 'NONE',  ( -0.1287570809895632329, 0.3962735484563137400, 10.00000000000000000 ) ) ;
#15390 = CARTESIAN_POINT ( 'NONE',  ( 195.0540265531851105, -1.025126265847089657, -120.9317124430720440 ) ) ;
#15391 = CARTESIAN_POINT ( 'NONE',  ( 32.43949840348898306, 7.871562655726499713, -9.367992836599954742 ) ) ;
#15392 = EDGE_CURVE ( 'NONE', #22621, #15132, #30478, .T. ) ;
#15393 = ORIENTED_EDGE ( 'NONE', *, *, #15466, .T. ) ;
#15394 = ORIENTED_EDGE ( 'NONE', *, *, #19352, .T. ) ;
#15395 = CARTESIAN_POINT ( 'NONE',  ( 135.0000000000006253, 16.00000000000000000, -54.99999999999999289 ) ) ;
#15396 = ORIENTED_EDGE ( 'NONE', *, *, #3261, .T. ) ;
#15397 = DIRECTION ( 'NONE',  ( 0.000000000000000000, 1.000000000000000000, -1.822804496942679766E-16 ) ) ;
#15398 =( BOUNDED_CURVE ( )  B_SPLINE_CURVE ( 3, ( #21456, #37642, #49124, #6574 ),
 .UNSPECIFIED., .F., .F. ) 
 B_SPLINE_CURVE_WITH_KNOTS ( ( 4, 4 ),
 ( 1.570796326794896558, 3.141592653589793116 ),
 .UNSPECIFIED. ) 
 CURVE ( )  GEOMETRIC_REPRESENTATION_ITEM ( )  RATIONAL_B_SPLINE_CURVE ( ( 1.000000000000000000, 0.8047378541243649375, 0.8047378541243649375, 1.000000000000000000 ) ) 
 REPRESENTATION_ITEM ( '' )  );
#15399 = VERTEX_POINT ( 'NONE', #25369 ) ;
#15400 = FILL_AREA_STYLE ('',( #30290 ) ) ;
#15401 = ORIENTED_EDGE ( 'NONE', *, *, #15626, .T. ) ;
#15402 = VECTOR ( 'NONE', #41497, 1000.000000000000000 ) ;
#15403 = ORIENTED_EDGE ( 'NONE', *, *, #12863, .F. ) ;
#15404 = LINE ( 'NONE', #35931, #6519 ) ;
#15405 = CARTESIAN_POINT ( 'NONE',  ( -6.695973446814940111, 1.750000000000023759, 40.81828755692798438 ) ) ;
#15406 = EDGE_LOOP ( 'NONE', ( #6135, #41283, #3959, #37596 ) ) ;
#15407 = CARTESIAN_POINT ( 'NONE',  ( 168.9999999999999716, -174.9999999999999716, -340.0000000000001137 ) ) ;
#15408 = LINE ( 'NONE', #31064, #40646 ) ;
#15409 = CARTESIAN_POINT ( 'NONE',  ( 210.0000000000000568, 0.000000000000000000, -159.1817124430720298 ) ) ;
#15410 = ORIENTED_EDGE ( 'NONE', *, *, #1218, .T. ) ;
#15411 = CARTESIAN_POINT ( 'NONE',  ( 210.0000000000000568, 2.143131898507881856E-16, -120.9317124430720582 ) ) ;
#15412 = LINE ( 'NONE', #35184, #5085 ) ;
#15413 = EDGE_LOOP ( 'NONE', ( #25067, #42925, #13394, #2651 ) ) ;
#15414 = DIRECTION ( 'NONE',  ( 0.000000000000000000, 0.000000000000000000, 1.000000000000000000 ) ) ;
#15415 = LINE ( 'NONE', #42595, #23985 ) ;
#15416 = ORIENTED_EDGE ( 'NONE', *, *, #8060, .T. ) ;
#15417 = DIRECTION ( 'NONE',  ( 1.000000000000000000, 0.000000000000000000, 0.000000000000000000 ) ) ;
#15418 = EDGE_CURVE ( 'NONE', #20304, #28229, #50079, .T. ) ;
#15419 = CARTESIAN_POINT ( 'NONE',  ( 0.000000000000000000, 181.0000000000000284, -342.0000000000001705 ) ) ;
#15420 = B_SPLINE_SURFACE_WITH_KNOTS ( 'NONE', 3, 3, ( 
 ( #40439, #47833, #12721, #4769 ),
 ( #28885, #44010, #17331, #39691 ),
 ( #16328, #20416, #31991, #6793 ),
 ( #25283, #25792, #26046, #9880 ) ),
 .UNSPECIFIED., .F., .F., .F.,
 ( 4, 4 ),
 ( 4, 4 ),
 ( 0.000000000000000000, 1.000000000000000000 ),
 ( 0.000000000000000000, 1.000000000000000000 ),
 .UNSPECIFIED. ) ;
#15421 = ORIENTED_EDGE ( 'NONE', *, *, #35913, .T. ) ;
#15422 = CYLINDRICAL_SURFACE ( 'NONE', #16104, 37.50000000000000000 ) ;
#15423 = CARTESIAN_POINT ( 'NONE',  ( 130.0000000000021032, 16.00000000000000000, 95.00000000000000000 ) ) ;
#15424 = CARTESIAN_POINT ( 'NONE',  ( 154.3291528190321458, -1.750000000000009548, -118.1565861772249519 ) ) ;
#15425 = FACE_OUTER_BOUND ( 'NONE', #35001, .T. ) ;
#15426 = VERTEX_POINT ( 'NONE', #37689 ) ;
#15427 = CARTESIAN_POINT ( 'NONE',  ( 15.62858259096121216, -5.755205073598614440, -9.683996418299976483 ) ) ;
#15428 = LINE ( 'NONE', #26973, #4583 ) ;
#15429 = CARTESIAN_POINT ( 'NONE',  ( 0.000000000000000000, 0.000000000000000000, 790.0000000000000000 ) ) ;
#15430 = ORIENTED_EDGE ( 'NONE', *, *, #11496, .T. ) ;
#15431 = ORIENTED_EDGE ( 'NONE', *, *, #50537, .T. ) ;
#15432 =( LENGTH_UNIT ( ) NAMED_UNIT ( * ) SI_UNIT ( .MILLI., .METRE. ) );
#15433 = CARTESIAN_POINT ( 'NONE',  ( -126.6959734468149321, -1.749999999999997335, 80.81828755692798438 ) ) ;
#15434 = DIRECTION ( 'NONE',  ( 0.000000000000000000, -1.000000000000000000, 0.000000000000000000 ) ) ;
#15435 = CIRCLE ( 'NONE', #23640, 0.5000000000000004441 ) ;
#15436 = DIRECTION ( 'NONE',  ( -1.000000000000000000, -0.000000000000000000, -0.000000000000000000 ) ) ;
#15437 = LINE ( 'NONE', #38556, #15996 ) ;
#15438 = LINE ( 'NONE', #22370, #5132 ) ;
#15439 = ORIENTED_EDGE ( 'NONE', *, *, #29601, .T. ) ;
#15440 = CARTESIAN_POINT ( 'NONE',  ( 50.11058929355269953, -7.578863168071589662, 7.455576670931136185 ) ) ;
#15441 = CARTESIAN_POINT ( 'NONE',  ( 153.3040265531850537, 0.000000000000000000, 165.0000000000000000 ) ) ;
#15442 = CARTESIAN_POINT ( 'NONE',  ( 42.99990394833793061, 47.95759300784327905, 5.000000000000000000 ) ) ;
#15443 = CARTESIAN_POINT ( 'NONE',  ( -204.9459734468148895, 1.025126265847089879, -117.4317124430720156 ) ) ;
#15444 = ORIENTED_EDGE ( 'NONE', *, *, #24699, .F. ) ;
#15445 = CARTESIAN_POINT ( 'NONE',  ( 115.0540265531850395, 1.025126265847081442, -160.9317124430720014 ) ) ;
#15446 = DIRECTION ( 'NONE',  ( 0.000000000000000000, -0.4027858274925600890, -0.9152942571496521795 ) ) ;
#15447 = ORIENTED_EDGE ( 'NONE', *, *, #34201, .T. ) ;
#15448 = CARTESIAN_POINT ( 'NONE',  ( -6.508636631827791064, -15.75743548351446854, 8.953103998512858652 ) ) ;
#15449 = CARTESIAN_POINT ( 'NONE',  ( 80.00000000000122213, 17.00000000000000000, 5.000000000000004441 ) ) ;
#15450 = DIRECTION ( 'NONE',  ( -1.000000000000000000, -0.000000000000000000, 4.625929269271687073E-16 ) ) ;
#15451 = VERTEX_POINT ( 'NONE', #10473 ) ;
#15452 = FACE_OUTER_BOUND ( 'NONE', #31590, .T. ) ;
#15453 = DIRECTION ( 'NONE',  ( 1.000000000000000000, 0.000000000000000000, 0.000000000000000000 ) ) ;
#15454 = ORIENTED_EDGE ( 'NONE', *, *, #9944, .T. ) ;
#15455 = CARTESIAN_POINT ( 'NONE',  ( 341.9999999999999432, -180.9999999999999716, 355.9999999999998295 ) ) ;
#15456 = DIRECTION ( 'NONE',  ( -1.000000000000000000, 0.000000000000000000, -0.000000000000000000 ) ) ;
#15457 = DIRECTION ( 'NONE',  ( 1.000000000000000000, -4.105366553918459587E-48, -1.586032880504786307E-16 ) ) ;
#15458 = B_SPLINE_CURVE_WITH_KNOTS ( 'NONE', 3,
 ( #14156, #26232, #45942, #14673 ),
 .UNSPECIFIED., .F., .F.,
 ( 4, 4 ),
 ( 1.093182292142470417E-15, 0.0004154657329505190787 ),
 .UNSPECIFIED. ) ;
#15459 = ORIENTED_EDGE ( 'NONE', *, *, #46335, .T. ) ;
#15460 = ORIENTED_EDGE ( 'NONE', *, *, #39739, .F. ) ;
#15461 = FACE_OUTER_BOUND ( 'NONE', #14311, .T. ) ;
#15462 = CARTESIAN_POINT ( 'NONE',  ( 111.5540265531850679, 0.000000000000000000, -77.43171244307204404 ) ) ;
#15463 = VECTOR ( 'NONE', #29132, 1000.000000000000000 ) ;
#15464 = VECTOR ( 'NONE', #42321, 1000.000000000000000 ) ;
#15465 = EDGE_LOOP ( 'NONE', ( #43240, #45285, #30741, #20708 ) ) ;
#15466 = EDGE_CURVE ( 'NONE', #21643, #8176, #18647, .T. ) ;
#15467 = ORIENTED_EDGE ( 'NONE', *, *, #44632, .F. ) ;
#15468 = CYLINDRICAL_SURFACE ( 'NONE', #381, 1.750000000000015543 ) ;
#15469 = LINE ( 'NONE', #10606, #3788 ) ;
#15470 = CARTESIAN_POINT ( 'NONE',  ( 191.5540265531851105, 0.000000000000000000, 2.568287556927978166 ) ) ;
#15471 = ORIENTED_EDGE ( 'NONE', *, *, #18325, .F. ) ;
#15472 = CARTESIAN_POINT ( 'NONE',  ( 135.0000000000012790, 17.00000000000000000, 5.000000000000004441 ) ) ;
#15473 = ADVANCED_FACE ( 'NONE', ( #22521 ), #33840, .F. ) ;
#15474 = ORIENTED_EDGE ( 'NONE', *, *, #25946, .F. ) ;
#15475 = CARTESIAN_POINT ( 'NONE',  ( -16.02661358026017879, -4.530191650547607196, -9.683996418299976483 ) ) ;
#15476 = CLOSED_SHELL ( 'NONE', ( #28589, #25174, #20477, #19016, #22186, #7367, #36643, #4697, #20824, #23737, #23148, #43681, #50178, #13592, #4561, #8844, #38261, #16211 ) ) ;
#15477 = ADVANCED_FACE ( 'NONE', ( #11999 ), #7645, .T. ) ;
#15478 = DIRECTION ( 'NONE',  ( -0.000000000000000000, -0.000000000000000000, -1.000000000000000000 ) ) ;
#15479 = ADVANCED_FACE ( 'NONE', ( #47096 ), #15082, .T. ) ;
#15480 = AXIS2_PLACEMENT_3D ( 'NONE', #2524, #5612, #13308 ) ;
#15481 = LINE ( 'NONE', #41918, #13222 ) ;
#15482 = ORIENTED_EDGE ( 'NONE', *, *, #2655, .T. ) ;
#15483 = VERTEX_POINT ( 'NONE', #46349 ) ;
#15484 = ORIENTED_EDGE ( 'NONE', *, *, #21100, .F. ) ;
#15485 = CARTESIAN_POINT ( 'NONE',  ( 115.0540265531850679, 0.000000000000000000, 162.5682875569279702 ) ) ;
#15486 = CARTESIAN_POINT ( 'NONE',  ( -40.86389006639098653, -8.513139889764316237, -8.080361901872240793 ) ) ;
#15487 = CARTESIAN_POINT ( 'NONE',  ( 30.00000000000029132, 16.00000000000000000, -84.99999999999998579 ) ) ;
#15488 = VERTEX_POINT ( 'NONE', #43285 ) ;
#15489 = CARTESIAN_POINT ( 'NONE',  ( -1.468446590252919348, -0.3226319952343834063, 9.953784399990620813 ) ) ;
#15490 = ORIENTED_EDGE ( 'NONE', *, *, #21486, .T. ) ;
#15491 = CYLINDRICAL_SURFACE ( 'NONE', #21752, 10.00000000000000000 ) ;
#15492 = VERTEX_POINT ( 'NONE', #35373 ) ;
#15493 = CARTESIAN_POINT ( 'NONE',  ( 165.0000000000000284, 165.0000000000000000, 355.9999999999998863 ) ) ;
#15494 = CARTESIAN_POINT ( 'NONE',  ( -84.94597344681494633, 2.143131898507880377E-16, 159.0682875569279702 ) ) ;
#15495 = LINE ( 'NONE', #27306, #1284 ) ;
#15496 = LINE ( 'NONE', #38615, #11039 ) ;
#15497 = ORIENTED_EDGE ( 'NONE', *, *, #43098, .T. ) ;
#15498 = ORIENTED_EDGE ( 'NONE', *, *, #26868, .T. ) ;
#15499 = CARTESIAN_POINT ( 'NONE',  ( -128.4459734468149179, 0.000000000000000000, 165.0000000000000000 ) ) ;
#15500 = CARTESIAN_POINT ( 'NONE',  ( 73.30402655318508209, -1.750000000000010658, -119.1817124430720440 ) ) ;
#15501 = CARTESIAN_POINT ( 'NONE',  ( -33.08717642956897009, -5.870837526464928402, -8.016098858316199838 ) ) ;
#15502 = ADVANCED_FACE ( 'NONE', ( #31004 ), #34858, .F. ) ;
#15503 = EDGE_CURVE ( 'NONE', #5556, #28357, #9892, .T. ) ;
#15504 = AXIS2_PLACEMENT_3D ( 'NONE', #35980, #822, #43901 ) ;
#15505 = EDGE_CURVE ( 'NONE', #21893, #13072, #5094, .T. ) ;
#15506 = EDGE_CURVE ( 'NONE', #25636, #36281, #11244, .T. ) ;
#15507 = VECTOR ( 'NONE', #29263, 1000.000000000000000 ) ;
#15508 = DIRECTION ( 'NONE',  ( -3.172065784643302499E-16, -1.000000000000000000, 2.537652627714642000E-15 ) ) ;
#15509 = VECTOR ( 'NONE', #8486, 1000.000000000000000 ) ;
#15510 = EDGE_CURVE ( 'NONE', #31874, #15492, #19693, .T. ) ;
#15511 = ORIENTED_EDGE ( 'NONE', *, *, #27869, .T. ) ;
#15512 = CIRCLE ( 'NONE', #36866, 37.50000000000000000 ) ;
#15513 = LINE ( 'NONE', #12175, #28652 ) ;
#15514 = EDGE_CURVE ( 'NONE', #13717, #21643, #2617, .T. ) ;
#15515 = FACE_OUTER_BOUND ( 'NONE', #20747, .T. ) ;
#15516 = ORIENTED_EDGE ( 'NONE', *, *, #27935, .F. ) ;
#15517 = VECTOR ( 'NONE', #6554, 1000.000000000000000 ) ;
#15518 = PLANE ( 'NONE',  #47519 ) ;
#15519 = CARTESIAN_POINT ( 'NONE',  ( 15.00000000000000000, -46.01315789473684248, 5.916985404131814619 ) ) ;
#15520 = FACE_OUTER_BOUND ( 'NONE', #3996, .T. ) ;
#15521 = ORIENTED_EDGE ( 'NONE', *, *, #4280, .F. ) ;
#15522 = PRODUCT_DEFINITION_SHAPE ( 'NONE', 'NONE',  #50734 ) ;
#15523 = EDGE_LOOP ( 'NONE', ( #46864, #40825, #39064, #2113, #34554, #37085 ) ) ;
#15524 = ADVANCED_FACE ( 'NONE', ( #39209 ), #11490, .T. ) ;
#15525 = CYLINDRICAL_SURFACE ( 'NONE', #21798, 1.750000000000001554 ) ;
#15526 = ADVANCED_FACE ( 'NONE', ( #15845 ), #42516, .T. ) ;
#15527 = CARTESIAN_POINT ( 'NONE',  ( 2.462075149652696027, -16.57295996686994499, 9.403735324607438884 ) ) ;
#15528 =( BOUNDED_CURVE ( )  B_SPLINE_CURVE ( 3, ( #27304, #47522, #15255, #31415 ),
 .UNSPECIFIED., .F., .F. ) 
 B_SPLINE_CURVE_WITH_KNOTS ( ( 4, 4 ),
 ( 4.710277376051313914E-16, 1.570796326794896780 ),
 .UNSPECIFIED. ) 
 CURVE ( )  GEOMETRIC_REPRESENTATION_ITEM ( )  RATIONAL_B_SPLINE_CURVE ( ( 1.000000000000000000, 0.8047378541243650485, 0.8047378541243650485, 1.000000000000000000 ) ) 
 REPRESENTATION_ITEM ( '' )  );
#15529 = EDGE_CURVE ( 'NONE', #32098, #36777, #42934, .T. ) ;
#15530 = ORIENTED_EDGE ( 'NONE', *, *, #6120, .T. ) ;
#15531 = ADVANCED_FACE ( 'NONE', ( #22776 ), #15593, .T. ) ;
#15532 = ORIENTED_EDGE ( 'NONE', *, *, #34334, .T. ) ;
#15533 = LINE ( 'NONE', #35558, #27235 ) ;
#15534 = CARTESIAN_POINT ( 'NONE',  ( 112.2789002873379758, -1.749999999999996669, 39.79316129108089228 ) ) ;
#15535 = ORIENTED_EDGE ( 'NONE', *, *, #22070, .F. ) ;
#15536 = ORIENTED_EDGE ( 'NONE', *, *, #35291, .T. ) ;
#15537 = ORIENTED_EDGE ( 'NONE', *, *, #26805, .F. ) ;
#15538 =( BOUNDED_CURVE ( )  B_SPLINE_CURVE ( 3, ( #37903, #6832, #18362, #18615 ),
 .UNSPECIFIED., .F., .F. ) 
 B_SPLINE_CURVE_WITH_KNOTS ( ( 4, 4 ),
 ( 1.570796326794896558, 3.141592653589793116 ),
 .UNSPECIFIED. ) 
 CURVE ( )  GEOMETRIC_REPRESENTATION_ITEM ( )  RATIONAL_B_SPLINE_CURVE ( ( 1.000000000000000000, 0.8047378541243649375, 0.8047378541243649375, 1.000000000000000000 ) ) 
 REPRESENTATION_ITEM ( '' )  );
#15539 = CIRCLE ( 'NONE', #828, 2.000000000000001776 ) ;
#15540 = EDGE_CURVE ( 'NONE', #19505, #17731, #26882, .T. ) ;
#15541 = CARTESIAN_POINT ( 'NONE',  ( -16.52264463346130796, 2.779753662172870232, 9.403735324607438884 ) ) ;
#15542 = VECTOR ( 'NONE', #11031, 1000.000000000000000 ) ;
#15543 = CARTESIAN_POINT ( 'NONE',  ( -37.90972275097263378, -14.83505920947805734, 901.8832493327278144 ) ) ;
#15544 = EDGE_LOOP ( 'NONE', ( #31972, #30060, #50586, #7176, #43121 ) ) ;
#15545 = AXIS2_PLACEMENT_3D ( 'NONE', #9443, #18582, #37869 ) ;
#15546 = CARTESIAN_POINT ( 'NONE',  ( 6.174150299305392053, -33.14591993373988998, 8.807470649214879543 ) ) ;
#15547 = DIRECTION ( 'NONE',  ( -0.000000000000000000, -0.000000000000000000, -1.000000000000000000 ) ) ;
#15548 = CARTESIAN_POINT ( 'NONE',  ( -64.99999999999846523, 17.00000000000000000, 60.00000000000000000 ) ) ;
#15549 = ORIENTED_EDGE ( 'NONE', *, *, #8900, .F. ) ;
#15550 = VERTEX_POINT ( 'NONE', #457 ) ;
#15551 = CARTESIAN_POINT ( 'NONE',  ( -8.445973446814976526, 0.000000000000000000, -0.9317124430720524764 ) ) ;
#15552 = EDGE_CURVE ( 'NONE', #19482, #6876, #48443, .T. ) ;
#15553 = CARTESIAN_POINT ( 'NONE',  ( -114.9999999999987779, 16.00000000000000000, 5.000000000000004441 ) ) ;
#15554 = VERTEX_POINT ( 'NONE', #16099 ) ;
#15555 = ORIENTED_EDGE ( 'NONE', *, *, #20462, .F. ) ;
#15556 = FACE_OUTER_BOUND ( 'NONE', #23597, .T. ) ;
#15557 = LINE ( 'NONE', #24280, #30509 ) ;
#15558 = VERTEX_POINT ( 'NONE', #39965 ) ;
#15559 = VECTOR ( 'NONE', #44515, 1000.000000000000000 ) ;
#15560 = CARTESIAN_POINT ( 'NONE',  ( -126.6959734468149321, 0.000000000000000000, 165.0000000000000000 ) ) ;
#15561 = DIRECTION ( 'NONE',  ( 0.000000000000000000, 0.000000000000000000, 1.000000000000000000 ) ) ;
#15562 = LINE ( 'NONE', #31984, #34333 ) ;
#15563 = EDGE_CURVE ( 'NONE', #37586, #46541, #30819, .T. ) ;
#15564 = CARTESIAN_POINT ( 'NONE',  ( 35.00000000000152767, 17.00000000000000000, 35.00000000000000000 ) ) ;
#15565 = ORIENTED_EDGE ( 'NONE', *, *, #21501, .F. ) ;
#15566 = DIRECTION ( 'NONE',  ( 0.000000000000000000, 0.000000000000000000, -1.000000000000000000 ) ) ;
#15567 = LINE ( 'NONE', #4277, #32624 ) ;
#15568 = CARTESIAN_POINT ( 'NONE',  ( -86.69597344681496054, 0.000000000000000000, 165.0000000000000000 ) ) ;
#15569 = EDGE_CURVE ( 'NONE', #46042, #31660, #25561, .T. ) ;
#15570 = ADVANCED_FACE ( 'NONE', ( #24317 ), #962, .T. ) ;
#15571 = ORIENTED_EDGE ( 'NONE', *, *, #42860, .F. ) ;
#15572 = DIRECTION ( 'NONE',  ( 0.000000000000000000, -0.2223603367690656640, -0.9749645535258950613 ) ) ;
#15573 = ADVANCED_FACE ( 'NONE', ( #24554 ), #21200, .T. ) ;
#15574 = CARTESIAN_POINT ( 'NONE',  ( -0.3862712429686809279, -1.188820645368943163, 10.00000000000000000 ) ) ;
#15575 = VECTOR ( 'NONE', #44786, 1000.000000000000000 ) ;
#15576 = LINE ( 'NONE', #46831, #37804 ) ;
#15577 = EDGE_CURVE ( 'NONE', #49298, #27092, #47858, .T. ) ;
#15578 = VECTOR ( 'NONE', #37124, 1000.000000000000114 ) ;
#15579 = ORIENTED_EDGE ( 'NONE', *, *, #43730, .F. ) ;
#15580 = DIRECTION ( 'NONE',  ( 2.220446049250312588E-16, 0.7071067811865475727, -0.7071067811865474617 ) ) ;
#15581 = AXIS2_PLACEMENT_3D ( 'NONE', #33007, #17839, #10142 ) ;
#15582 = ORIENTED_EDGE ( 'NONE', *, *, #19728, .T. ) ;
#15583 = CARTESIAN_POINT ( 'NONE',  ( 153.3040265531850537, -1.750000000000010214, -39.18171244307202983 ) ) ;
#15584 = CARTESIAN_POINT ( 'NONE',  ( 71.55402655318505367, 1.025126265847089435, 39.06828755692797728 ) ) ;
#15585 = DIRECTION ( 'NONE',  ( -4.758098676964956461E-16, 0.000000000000000000, -1.000000000000000000 ) ) ;
#15586 = AXIS2_PLACEMENT_3D ( 'NONE', #12769, #40483, #24575 ) ;
#15587 = CARTESIAN_POINT ( 'NONE',  ( 210.0000000000000568, 0.000000000000000000, -37.43171244307202272 ) ) ;
#15588 = EDGE_CURVE ( 'NONE', #45408, #34855, #13115, .T. ) ;
#15589 = EDGE_LOOP ( 'NONE', ( #29356, #36432, #18559, #13887 ) ) ;
#15590 = VERTEX_POINT ( 'NONE', #20436 ) ;
#15591 = VERTEX_POINT ( 'NONE', #12487 ) ;
#15592 = DIRECTION ( 'NONE',  ( -0.000000000000000000, -0.000000000000000000, 1.000000000000000000 ) ) ;
#15593 = CYLINDRICAL_SURFACE ( 'NONE', #13156, 1.749999999999987566 ) ;
#15594 = AXIS2_PLACEMENT_3D ( 'NONE', #4174, #35490, #50561 ) ;
#15595 = EDGE_LOOP ( 'NONE', ( #26883, #1599, #15244 ) ) ;
#15596 = ADVANCED_FACE ( 'NONE', ( #12749 ), #44524, .F. ) ;
#15597 = LINE ( 'NONE', #27655, #41789 ) ;
#15598 = CYLINDRICAL_SURFACE ( 'NONE', #16734, 1.749999999999973799 ) ;
#15599 = CARTESIAN_POINT ( 'NONE',  ( 0.000000000000000000, 0.000000000000000000, 0.000000000000000000 ) ) ;
#15600 = ORIENTED_EDGE ( 'NONE', *, *, #12661, .T. ) ;
#15601 = CARTESIAN_POINT ( 'NONE',  ( -205.6708471809678827, 1.750000000000010214, 119.7931612910808781 ) ) ;
#15602 = CARTESIAN_POINT ( 'NONE',  ( -208.1473046169136296, -154.8119894309598976, 472.8425600500173118 ) ) ;
#15603 =( NAMED_UNIT ( * ) SI_UNIT ( $, .STERADIAN. ) SOLID_ANGLE_UNIT ( ) );
#15604 = VERTEX_POINT ( 'NONE', #28157 ) ;
#15605 = DIRECTION ( 'NONE',  ( -1.000000000000000000, -0.000000000000000000, -0.000000000000000000 ) ) ;
#15606 = CARTESIAN_POINT ( 'NONE',  ( -85.67084718096784002, 1.750000000000009548, 1.843413822775065825 ) ) ;
#15607 = ORIENTED_EDGE ( 'NONE', *, *, #23316, .F. ) ;
#15608 = VERTEX_POINT ( 'NONE', #43788 ) ;
#15609 = ORIENTED_EDGE ( 'NONE', *, *, #27826, .F. ) ;
#15610 = DIRECTION ( 'NONE',  ( 0.000000000000000000, 0.000000000000000000, 1.000000000000000000 ) ) ;
#15611 = ORIENTED_EDGE ( 'NONE', *, *, #15854, .F. ) ;
#15612 = VECTOR ( 'NONE', #9967, 1000.000000000000000 ) ;
#15613 = CARTESIAN_POINT ( 'NONE',  ( -2.961022939495062900, 16.59676755884084187, 2.590526750877053086 ) ) ;
#15614 = LINE ( 'NONE', #4070, #9036 ) ;
#15615 = CARTESIAN_POINT ( 'NONE',  ( -0.3862712429686895876, 1.188820645368940720, 10.00000000000000000 ) ) ;
#15616 = CARTESIAN_POINT ( 'NONE',  ( -14.49999999999999822, -46.01315789473684248, 5.916985404131813731 ) ) ;
#15617 = LINE ( 'NONE', #43058, #34034 ) ;
#15618 = PLANE ( 'NONE',  #26569 ) ;
#15619 = CARTESIAN_POINT ( 'NONE',  ( 1.862232582514315338, 0.9302239440314843399, 9.888808121373909188 ) ) ;
#15620 = CARTESIAN_POINT ( 'NONE',  ( 181.0000000000000284, -174.9999999999999716, -115.0000000000001563 ) ) ;
#15621 = VECTOR ( 'NONE', #19256, 1000.000000000000000 ) ;
#15622 = CARTESIAN_POINT ( 'NONE',  ( -166.6959734468149463, -1.750000000000010658, 120.8182875569279702 ) ) ;
#15623 = PRESENTATION_LAYER_ASSIGNMENT (  '', '', ( #22971 ) ) ;
#15624 = ORIENTED_EDGE ( 'NONE', *, *, #19903, .T. ) ;
#15625 = CARTESIAN_POINT ( 'NONE',  ( 35.00000000000028422, 17.00000000000000000, -84.99999999999998579 ) ) ;
#15626 = EDGE_CURVE ( 'NONE', #23844, #5437, #683, .T. ) ;
#15627 = EDGE_CURVE ( 'NONE', #42197, #27344, #44032, .T. ) ;
#15628 = CARTESIAN_POINT ( 'NONE',  ( -64.99999999999846523, 17.00000000000000000, 35.00000000000000000 ) ) ;
#15629 = CARTESIAN_POINT ( 'NONE',  ( 168.9999999999999716, 6.000000000000060396, -350.0000000000001705 ) ) ;
#15630 = ORIENTED_EDGE ( 'NONE', *, *, #16810, .F. ) ;
#15631 = DIRECTION ( 'NONE',  ( 1.000000000000000000, 0.000000000000000000, 0.000000000000000000 ) ) ;
#15632 = EDGE_CURVE ( 'NONE', #14566, #34169, #40713, .T. ) ;
#15633 = CARTESIAN_POINT ( 'NONE',  ( -165.3973046169136012, -98.56198943095992604, 22.84256005001721945 ) ) ;
#15634 = CARTESIAN_POINT ( 'NONE',  ( 85.00000000000029843, 17.00000000000000000, -84.99999999999998579 ) ) ;
#15635 = DIRECTION ( 'NONE',  ( 1.000000000000000000, 0.000000000000000000, 0.000000000000000000 ) ) ;
#15636 = EDGE_CURVE ( 'NONE', #7012, #38661, #49182, .T. ) ;
#15637 = EDGE_CURVE ( 'NONE', #13383, #16751, #21657, .T. ) ;
#15638 = VERTEX_POINT ( 'NONE', #8409 ) ;
#15639 = SURFACE_SIDE_STYLE ('',( #31564 ) ) ;
#15640 = ORIENTED_EDGE ( 'NONE', *, *, #22992, .T. ) ;
#15641 = SPHERICAL_SURFACE ( 'NONE', #5718, 0.5000000000000000000 ) ;
#15642 = EDGE_LOOP ( 'NONE', ( #40302, #33952 ) ) ;
#15643 = LINE ( 'NONE', #39261, #13948 ) ;
#15644 = CARTESIAN_POINT ( 'NONE',  ( -124.9459734468149321, 1.025126265847082108, -77.43171244307201562 ) ) ;
#15645 = ADVANCED_FACE ( 'NONE', ( #20700 ), #36376, .T. ) ;
#15646 = VERTEX_POINT ( 'NONE', #29166 ) ;
#15647 = CARTESIAN_POINT ( 'NONE',  ( 0.000000000000000000, 23.48684210526316107, -5.000000000000000000 ) ) ;
#15648 = ORIENTED_EDGE ( 'NONE', *, *, #35405, .T. ) ;
#15649 = VECTOR ( 'NONE', #23736, 1000.000000000000000 ) ;
#15650 = CIRCLE ( 'NONE', #40131, 4.000000000000003553 ) ;
#15651 = ORIENTED_EDGE ( 'NONE', *, *, #21458, .T. ) ;
#15652 = CYLINDRICAL_SURFACE ( 'NONE', #17189, 0.5000000000000004441 ) ;
#15653 = CARTESIAN_POINT ( 'NONE',  ( 30.00000000000218492, 17.00000000000000000, 115.0000000000000142 ) ) ;
#15654 = ORIENTED_EDGE ( 'NONE', *, *, #38408, .F. ) ;
#15655 = DIRECTION ( 'NONE',  ( 1.000000000000000000, 0.000000000000000000, 0.000000000000000000 ) ) ;
#15656 = DIRECTION ( 'NONE',  ( 0.000000000000000000, -1.000000000000000000, 0.000000000000000000 ) ) ;
#15657 = EDGE_LOOP ( 'NONE', ( #20614, #4539, #26329, #40733 ) ) ;
#15658 = CIRCLE ( 'NONE', #23004, 10.00000000000000000 ) ;
#15659 = LINE ( 'NONE', #15918, #30048 ) ;
#15660 = PLANE ( 'NONE',  #46849 ) ;
#15661 = ORIENTED_EDGE ( 'NONE', *, *, #26939, .F. ) ;
#15662 = CARTESIAN_POINT ( 'NONE',  ( -1.250000000000000222, 0.000000000000000000, -10.00000000000000000 ) ) ;
#15663 = DIRECTION ( 'NONE',  ( 0.000000000000000000, -1.000000000000000000, 1.822804496942680012E-16 ) ) ;
#15664 = ORIENTED_EDGE ( 'NONE', *, *, #26431, .F. ) ;
#15665 = DIRECTION ( 'NONE',  ( -0.4374820812098839107, 0.3178493372392718896, -0.8411784753765542133 ) ) ;
#15666 = DIRECTION ( 'NONE',  ( 0.000000000000000000, -1.000000000000000000, 1.822804496942679766E-16 ) ) ;
#15667 = VERTEX_POINT ( 'NONE', #6813 ) ;
#15668 = ADVANCED_FACE ( 'NONE', ( #37634 ), #40961, .F. ) ;
#15669 = DIRECTION ( 'NONE',  ( 0.000000000000000000, -3.186989995019654210E-49, -1.000000000000000000 ) ) ;
#15670 = CARTESIAN_POINT ( 'NONE',  ( 181.0000000000000284, 2.775557561562891351E-14, -99.00000000000014211 ) ) ;
#15671 = CARTESIAN_POINT ( 'NONE',  ( 151.5540265531850537, 0.000000000000000000, 162.5682875569279702 ) ) ;
#15672 =( BOUNDED_CURVE ( )  B_SPLINE_CURVE ( 3, ( #27012, #43661, #4178, #15719 ),
 .UNSPECIFIED., .F., .F. ) 
 B_SPLINE_CURVE_WITH_KNOTS ( ( 4, 4 ),
 ( 1.570796326794896558, 3.141592653589793116 ),
 .UNSPECIFIED. ) 
 CURVE ( )  GEOMETRIC_REPRESENTATION_ITEM ( )  RATIONAL_B_SPLINE_CURVE ( ( 1.000000000000000000, 0.8047378541243649375, 0.8047378541243649375, 1.000000000000000000 ) ) 
 REPRESENTATION_ITEM ( '' )  );
#15673 = PLANE ( 'NONE',  #35411 ) ;
#15674 = ORIENTED_EDGE ( 'NONE', *, *, #43183, .T. ) ;
#15675 = CARTESIAN_POINT ( 'NONE',  ( -24.39427009666018265, -44.07992421011638129, 8.807470649214879543 ) ) ;
#15676 = CARTESIAN_POINT ( 'NONE',  ( 45.42829307628542779, 21.98948915213303579, 8.356839323120299312 ) ) ;
#15677 =( BOUNDED_CURVE ( )  B_SPLINE_CURVE ( 3, ( #6608, #22261, #19155, #26618 ),
 .UNSPECIFIED., .F., .F. ) 
 B_SPLINE_CURVE_WITH_KNOTS ( ( 4, 4 ),
 ( 3.141592653589793116, 4.712388980384689674 ),
 .UNSPECIFIED. ) 
 CURVE ( )  GEOMETRIC_REPRESENTATION_ITEM ( )  RATIONAL_B_SPLINE_CURVE ( ( 1.000000000000000000, 0.8047378541243649375, 0.8047378541243649375, 1.000000000000000000 ) ) 
 REPRESENTATION_ITEM ( '' )  );
#15678 = CARTESIAN_POINT ( 'NONE',  ( -34.95136153415531766, 36.40974830873496870, 8.356839323120299312 ) ) ;
#15679 = EDGE_LOOP ( 'NONE', ( #850, #27293, #36659, #23019, #4968, #12330, #15430, #12892 ) ) ;
#15681 = ORIENTED_EDGE ( 'NONE', *, *, #7478, .T. ) ;
#15680 = AXIS2_PLACEMENT_3D ( 'NONE', #23309, #38725, #46382 ) ;
#15682 = CARTESIAN_POINT ( 'NONE',  ( 867.4995338190004759, 1338.153237050701819, 1561.986414963432253 ) ) ;
#15683 = CARTESIAN_POINT ( 'NONE',  ( 210.0000000000000568, 0.000000000000000000, -159.1817124430720298 ) ) ;
#15684 = CARTESIAN_POINT ( 'NONE',  ( -1.211301556933465751, -0.1727733738854601298, 9.993783931180535873 ) ) ;
#15685 = PLANE ( 'NONE',  #28311 ) ;
#15686 = CARTESIAN_POINT ( 'NONE',  ( 1.057156451998911839, -0.7920882637786250680, 9.943883492372851407 ) ) ;
#15687 = DIRECTION ( 'NONE',  ( 0.000000000000000000, -1.000000000000000000, 0.000000000000000000 ) ) ;
#15688 = VERTEX_POINT ( 'NONE', #2214 ) ;
#15689 = CARTESIAN_POINT ( 'NONE',  ( 155.0540265531850537, 1.025126265847089435, 39.06828755692797728 ) ) ;
#15690 =( BOUNDED_CURVE ( )  B_SPLINE_CURVE ( 3, ( #24267, #39920, #4999, #16056 ),
 .UNSPECIFIED., .F., .F. ) 
 B_SPLINE_CURVE_WITH_KNOTS ( ( 4, 4 ),
 ( 1.570796326794896558, 3.141592653589793116 ),
 .UNSPECIFIED. ) 
 CURVE ( )  GEOMETRIC_REPRESENTATION_ITEM ( )  RATIONAL_B_SPLINE_CURVE ( ( 1.000000000000000000, 0.8047378541243649375, 0.8047378541243649375, 1.000000000000000000 ) ) 
 REPRESENTATION_ITEM ( '' )  );
#15692 = VECTOR ( 'NONE', #40079, 1000.000000000000000 ) ;
#15691 = CARTESIAN_POINT ( 'NONE',  ( -34.08355720199904226, 2.371364769369340042, 7.455576670931136185 ) ) ;
#15693 = CARTESIAN_POINT ( 'NONE',  ( 2.097926912204255867, -0.2448757052703989245, 9.890170120223999106 ) ) ;
#15694 = DIRECTION ( 'NONE',  ( 0.000000000000000000, -1.000000000000000000, 2.537652627714643577E-15 ) ) ;
#15695 = ORIENTED_EDGE ( 'NONE', *, *, #25940, .T. ) ;
#15696 = DIRECTION ( 'NONE',  ( 0.000000000000000000, -0.3846153846153845812, -0.9230769230769231282 ) ) ;
#15697 = ORIENTED_EDGE ( 'NONE', *, *, #45308, .F. ) ;
#15698 = LINE ( 'NONE', #3378, #36852 ) ;
#15699 = CARTESIAN_POINT ( 'NONE',  ( -14.49999999999999822, 13.48684210526315930, -20.00000000000000000 ) ) ;
#15700 = ORIENTED_EDGE ( 'NONE', *, *, #17778, .T. ) ;
#15701 = EDGE_CURVE ( 'NONE', #7036, #30495, #14764, .T. ) ;
#15702 = CARTESIAN_POINT ( 'NONE',  ( -33.89193117067290473, 0.000000000000000000, 910.0000000000000000 ) ) ;
#15703 = PLANE ( 'NONE',  #18369 ) ;
#15704 = B_SPLINE_CURVE_WITH_KNOTS ( 'NONE', 3,
 ( #35974, #27506, #20558, #818 ),
 .UNSPECIFIED., .F., .F.,
 ( 4, 4 ),
 ( 0.01012863361515566052, 0.01015667504234235748 ),
 .UNSPECIFIED. ) ;
#15705 = SURFACE_STYLE_FILL_AREA ( #33764 ) ;
#15706 = DIRECTION ( 'NONE',  ( -1.000000000000000000, 0.000000000000000000, 0.000000000000000000 ) ) ;
#15707 = ORIENTED_EDGE ( 'NONE', *, *, #22940, .F. ) ;
#15708 = LINE ( 'NONE', #42642, #10564 ) ;
#15709 = DIRECTION ( 'NONE',  ( -1.000000000000000000, -0.000000000000000000, -0.000000000000000000 ) ) ;
#15710 = ORIENTED_EDGE ( 'NONE', *, *, #37506, .F. ) ;
#15711 = CARTESIAN_POINT ( 'NONE',  ( -0.8285222815141961572, -1.889008401827320771, 9.886433018048073507 ) ) ;
#15712 = CARTESIAN_POINT ( 'NONE',  ( -6.695973446814940111, 1.750000000000023315, -159.1817124430720298 ) ) ;
#15713 = CARTESIAN_POINT ( 'NONE',  ( 155.0540265531850537, 2.143131898507880377E-16, -77.43171244307204404 ) ) ;
#15714 = CARTESIAN_POINT ( 'NONE',  ( 85.00000000000152056, 17.00000000000000000, 35.00000000000000000 ) ) ;
#15715 = AXIS2_PLACEMENT_3D ( 'NONE', #12574, #41, #28244 ) ;
#15716 = ORIENTED_EDGE ( 'NONE', *, *, #5062, .T. ) ;
#15717 = B_SPLINE_CURVE_WITH_KNOTS ( 'NONE', 3,
 ( #3375, #25992, #41630, #6476 ),
 .UNSPECIFIED., .F., .F.,
 ( 4, 4 ),
 ( 0.002354859187796704348, 0.002825807655362034231 ),
 .UNSPECIFIED. ) ;
#15718 = ORIENTED_EDGE ( 'NONE', *, *, #13798, .F. ) ;
#15719 = CARTESIAN_POINT ( 'NONE',  ( 111.5540265531850679, 0.000000000000000000, -117.4317124430720725 ) ) ;
#15720 = VERTEX_POINT ( 'NONE', #14508 ) ;
#15721 = AXIS2_PLACEMENT_3D ( 'NONE', #20359, #36294, #43456 ) ;
#15722 = CARTESIAN_POINT ( 'NONE',  ( 1.019713130072856355, 3.848720492505100843, 4.370690007832189750E-16 ) ) ;
#15723 = CARTESIAN_POINT ( 'NONE',  ( -166.6959734468149463, -1.750000000000010214, 40.81828755692798438 ) ) ;
#15724 = DIRECTION ( 'NONE',  ( -0.000000000000000000, -1.000000000000000000, -0.000000000000000000 ) ) ;
#15725 = ORIENTED_EDGE ( 'NONE', *, *, #49974, .F. ) ;
#15726 = CARTESIAN_POINT ( 'NONE',  ( -5.888214538810513154, -16.20866436362413410, 8.727788335465566760 ) ) ;
#15727 = ORIENTED_EDGE ( 'NONE', *, *, #21188, .T. ) ;
#15728 = DIRECTION ( 'NONE',  ( -1.000000000000000000, -0.000000000000000000, -0.000000000000000000 ) ) ;
#15729 = EDGE_CURVE ( 'NONE', #31600, #23031, #23914, .T. ) ;
#15730 = CARTESIAN_POINT ( 'NONE',  ( 191.5540265531851105, 0.000000000000000000, 165.0000000000000000 ) ) ;
#15731 = DIRECTION ( 'NONE',  ( -0.000000000000000000, -0.000000000000000000, -1.000000000000000000 ) ) ;
#15732 = VERTEX_POINT ( 'NONE', #48860 ) ;
#15733 = ORIENTED_EDGE ( 'NONE', *, *, #22240, .T. ) ;
#15734 = ORIENTED_EDGE ( 'NONE', *, *, #34471, .F. ) ;
#15735 = CARTESIAN_POINT ( 'NONE',  ( 341.9999999999999432, -169.0000000000001137, -344.0000000000002842 ) ) ;
#15736 = B_SPLINE_CURVE_WITH_KNOTS ( 'NONE', 3,
 ( #25335, #5573, #1985, #1491 ),
 .UNSPECIFIED., .F., .F.,
 ( 4, 4 ),
 ( 0.0002936521407522070222, 0.0006663369986142620403 ),
 .UNSPECIFIED. ) ;
#15737 = PLANE ( 'NONE',  #25096 ) ;
#15738 = CARTESIAN_POINT ( 'NONE',  ( -166.6959734468149463, 1.750000000000010214, -39.18171244307202983 ) ) ;
#15739 = ORIENTED_EDGE ( 'NONE', *, *, #36078, .F. ) ;
#15740 = DIRECTION ( 'NONE',  ( -1.586032892321652236E-16, -1.000000000000000000, -2.288264760618012091E-48 ) ) ;
#15741 = VERTEX_POINT ( 'NONE', #48608 ) ;
#15742 = LINE ( 'NONE', #35268, #43025 ) ;
#15743 = ORIENTED_EDGE ( 'NONE', *, *, #9661, .T. ) ;
#15744 = SHAPE_REPRESENTATION_RELATIONSHIP ( 'NONE' , 'NONE' ,  #13952, #38746 ) ;
#15745 = LINE ( 'NONE', #619, #49752 ) ;
#15746 = CARTESIAN_POINT ( 'NONE',  ( 23.82716369509147825, 44.49195112876006419, 8.356839323120299312 ) ) ;
#15747 = CARTESIAN_POINT ( 'NONE',  ( 35.05402655318503946, 0.000000000000000000, 162.5682875569279702 ) ) ;
#15748 = CARTESIAN_POINT ( 'NONE',  ( 1.249999999999999778, -0.000000000000000000, -10.00000000000000000 ) ) ;
#15749 = CARTESIAN_POINT ( 'NONE',  ( -26.25702031264333058, 26.77347351953860155, 8.914903342594559632 ) ) ;
#15750 = ORIENTED_EDGE ( 'NONE', *, *, #46471, .F. ) ;
#15751 = ORIENTED_EDGE ( 'NONE', *, *, #8932, .F. ) ;
#15752 = CARTESIAN_POINT ( 'NONE',  ( -4.945973446814916130, -1.025126265847097429, 79.06828755692792754 ) ) ;
#15753 = AXIS2_PLACEMENT_3D ( 'NONE', #11893, #43187, #15995 ) ;
#15754 = CARTESIAN_POINT ( 'NONE',  ( -376.8544389702902890, 164.9999999999999716, 219.8317560660027539 ) ) ;
#15755 = CYLINDRICAL_SURFACE ( 'NONE', #12653, 1.750000000000001554 ) ;
#15756 = MECHANICAL_DESIGN_GEOMETRIC_PRESENTATION_REPRESENTATION (  '', ( #11662 ), #46070 ) ;
#15757 = CARTESIAN_POINT ( 'NONE',  ( -34.08355720199904226, 2.371364769369340042, 7.455576670931136185 ) ) ;
#15758 = VECTOR ( 'NONE', #17300, 1000.000000000000000 ) ;
#15759 = PLANE ( 'NONE',  #49864 ) ;
#15760 = ORIENTED_EDGE ( 'NONE', *, *, #46234, .F. ) ;
#15761 = EDGE_CURVE ( 'NONE', #2864, #46936, #21445, .T. ) ;
#15762 = DIRECTION ( 'NONE',  ( -0.000000000000000000, -1.000000000000000000, -0.000000000000000000 ) ) ;
#15763 = DIRECTION ( 'NONE',  ( -1.586032892321652236E-16, -1.000000000000000000, -2.288264760618012091E-48 ) ) ;
#15764 = ORIENTED_EDGE ( 'NONE', *, *, #18881, .T. ) ;
#15765 = DIRECTION ( 'NONE',  ( -1.000000000000000000, 0.000000000000000000, -0.000000000000000000 ) ) ;
#15766 = CARTESIAN_POINT ( 'NONE',  ( -21.61731705588949737, -25.43568671410585935, -9.367992836599954742 ) ) ;
#15767 = CARTESIAN_POINT ( 'NONE',  ( 9.696760411815720460, 2.443938934556958653, 0.000000000000000000 ) ) ;
#15768 = EDGE_CURVE ( 'NONE', #9775, #22165, #44258, .T. ) ;
#15769 = VECTOR ( 'NONE', #36065, 1000.000000000000000 ) ;
#15770 = EDGE_CURVE ( 'NONE', #24618, #4113, #18056, .T. ) ;
#15771 = ORIENTED_EDGE ( 'NONE', *, *, #50404, .T. ) ;
#15772 = ORIENTED_EDGE ( 'NONE', *, *, #6467, .T. ) ;
#15773 = CARTESIAN_POINT ( 'NONE',  ( 1.080000014128428498, 0.7606467978644730898, 9.943883492372853183 ) ) ;
#15774 = FACE_OUTER_BOUND ( 'NONE', #10674, .T. ) ;
#15775 = EDGE_CURVE ( 'NONE', #16324, #48417, #5808, .T. ) ;
#15776 = ORIENTED_EDGE ( 'NONE', *, *, #27154, .T. ) ;
#15777 = VERTEX_POINT ( 'NONE', #29404 ) ;
#15778 = LINE ( 'NONE', #31447, #23974 ) ;
#15779 = LINE ( 'NONE', #23220, #23278 ) ;
#15780 = FACE_OUTER_BOUND ( 'NONE', #42463, .T. ) ;
#15781 = DIRECTION ( 'NONE',  ( 1.000000000000000000, 0.000000000000000000, 0.000000000000000000 ) ) ;
#15782 = COLOUR_RGB ( '',0.7921568627450980005, 0.8196078431372548767, 0.9333333333333333481 ) ;
#15783 = ORIENTED_EDGE ( 'NONE', *, *, #32528, .F. ) ;
#15784 = ORIENTED_EDGE ( 'NONE', *, *, #19583, .T. ) ;
#15785 = VECTOR ( 'NONE', #14207, 1000.000000000000000 ) ;
#15786 = ORIENTED_EDGE ( 'NONE', *, *, #39968, .T. ) ;
#15787 = EDGE_CURVE ( 'NONE', #35621, #16704, #45027, .T. ) ;
#15788 = EDGE_CURVE ( 'NONE', #27142, #47198, #6055, .T. ) ;
#15789 = AXIS2_PLACEMENT_3D ( 'NONE', #27949, #39004, #12800 ) ;
#15790 = CARTESIAN_POINT ( 'NONE',  ( -5.670847180967843570, -1.750000000000023315, 41.84341382277508359 ) ) ;
#15791 = DIRECTION ( 'NONE',  ( -1.000000000000000000, -0.000000000000000000, -0.000000000000000000 ) ) ;
#15792 = EDGE_CURVE ( 'NONE', #47066, #4803, #48142, .T. ) ;
#15793 = VERTEX_POINT ( 'NONE', #49612 ) ;
#15794 = EDGE_CURVE ( 'NONE', #30045, #26155, #44204, .T. ) ;
#15795 = CARTESIAN_POINT ( 'NONE',  ( 1.337801958641917199, 1.088266084286984015, 9.928159647716135794 ) ) ;
#15796 = AXIS2_PLACEMENT_3D ( 'NONE', #5369, #28481, #32844 ) ;
#15797 = CARTESIAN_POINT ( 'NONE',  ( 358.0000000000001137, 169.0000000000000000, 343.9999999999998295 ) ) ;
#15798 = CYLINDRICAL_SURFACE ( 'NONE', #35318, 1.750000000000036193 ) ;
#15799 = EDGE_LOOP ( 'NONE', ( #16885, #16989, #26136, #16240 ) ) ;
#15800 = ORIENTED_EDGE ( 'NONE', *, *, #42123, .F. ) ;
#15801 = CARTESIAN_POINT ( 'NONE',  ( 35.00000000000216716, 17.00000000000000000, 95.00000000000000000 ) ) ;
#15802 = CARTESIAN_POINT ( 'NONE',  ( -44.94597344681493922, 1.025126265847089435, -40.93171244307204404 ) ) ;
#15803 = ADVANCED_FACE ( 'NONE', ( #6318 ), #1960, .T. ) ;
#15804 = CARTESIAN_POINT ( 'NONE',  ( 151.5540265531850537, 0.000000000000000000, 165.0000000000000000 ) ) ;
#15805 = UNCERTAINTY_MEASURE_WITH_UNIT (LENGTH_MEASURE( 1.000000000000000082E-05 ), #47360, 'distance_accuracy_value', 'NONE');
#15806 = EDGE_LOOP ( 'NONE', ( #20910, #47554, #29756, #26789 ) ) ;
#15807 = ORIENTED_EDGE ( 'NONE', *, *, #9302, .F. ) ;
#15808 = DIRECTION ( 'NONE',  ( 0.000000000000000000, 0.000000000000000000, 1.000000000000000000 ) ) ;
#15809 = VERTEX_POINT ( 'NONE', #45533 ) ;
#15810 = CARTESIAN_POINT ( 'NONE',  ( 155.0540265531850537, 2.143131898507880377E-16, 165.0000000000000000 ) ) ;
#15811 = FACE_OUTER_BOUND ( 'NONE', #30201, .T. ) ;
#15812 = CARTESIAN_POINT ( 'NONE',  ( 195.9526953830863079, -154.8119894309599260, 23.74256005001722158 ) ) ;
#15813 = CARTESIAN_POINT ( 'NONE',  ( -1.011271242968683426, -0.7347315653655928092, 10.00000000000000000 ) ) ;
#15814 = VERTEX_POINT ( 'NONE', #10413 ) ;
#15815 = CARTESIAN_POINT ( 'NONE',  ( 181.0000000000000000, 175.0000000000000284, -344.0000000000001137 ) ) ;
#15816 = CARTESIAN_POINT ( 'NONE',  ( 7.499999999999948486, -194.9999999999999716, -240.0000000000000000 ) ) ;
#15817 = LINE ( 'NONE', #23527, #26893 ) ;
#15818 = EDGE_CURVE ( 'NONE', #36401, #26375, #26064, .T. ) ;
#15819 = CARTESIAN_POINT ( 'NONE',  ( 130.0000000000008811, 16.00000000000000000, -24.99999999999999289 ) ) ;
#15820 = EDGE_CURVE ( 'NONE', #33697, #43357, #36141, .T. ) ;
#15821 = EDGE_CURVE ( 'NONE', #5037, #45423, #42664, .T. ) ;
#15822 = VECTOR ( 'NONE', #39768, 1000.000000000000000 ) ;
#15823 = ORIENTED_EDGE ( 'NONE', *, *, #22781, .F. ) ;
#15824 = FACE_OUTER_BOUND ( 'NONE', #35065, .T. ) ;
#15825 = EDGE_CURVE ( 'NONE', #26083, #16304, #8093, .T. ) ;
#15826 = CARTESIAN_POINT ( 'NONE',  ( -0.1287570809895602630, -0.3962735484563142396, 10.00000000000000000 ) ) ;
#15827 = CARTESIAN_POINT ( 'NONE',  ( 8.294258456918035094, 5.607426633512224257, 6.185594734181536936 ) ) ;
#15828 = VECTOR ( 'NONE', #18649, 1000.000000000000000 ) ;
#15829 = ADVANCED_FACE ( 'NONE', ( #15774 ), #27312, .T. ) ;
#15830 = VERTEX_POINT ( 'NONE', #7845 ) ;
#15831 = SURFACE_STYLE_USAGE ( .BOTH. , #23261 ) ;
#15832 = AXIS2_PLACEMENT_3D ( 'NONE', #34379, #33878, #49965 ) ;
#15833 = DIRECTION ( 'NONE',  ( 0.000000000000000000, -2.537652627714643577E-15, -1.000000000000000000 ) ) ;
#15834 = ORIENTED_EDGE ( 'NONE', *, *, #9244, .T. ) ;
#15835 = DIRECTION ( 'NONE',  ( -1.000000000000000000, 0.000000000000000000, -0.000000000000000000 ) ) ;
#15836 = FACE_BOUND ( 'NONE', #41434, .T. ) ;
#15837 = CARTESIAN_POINT ( 'NONE',  ( -167.4999999999999432, 102.5000000000000142, 10.00000000000000000 ) ) ;
#15838 =( BOUNDED_CURVE ( )  B_SPLINE_CURVE ( 3, ( #42141, #49794, #7004, #22649 ),
 .UNSPECIFIED., .F., .F. ) 
 B_SPLINE_CURVE_WITH_KNOTS ( ( 4, 4 ),
 ( 1.570796326794896558, 3.141592653589793116 ),
 .UNSPECIFIED. ) 
 CURVE ( )  GEOMETRIC_REPRESENTATION_ITEM ( )  RATIONAL_B_SPLINE_CURVE ( ( 1.000000000000000000, 0.8047378541243649375, 0.8047378541243649375, 1.000000000000000000 ) ) 
 REPRESENTATION_ITEM ( '' )  );
#15839 = ORIENTED_EDGE ( 'NONE', *, *, #42843, .T. ) ;
#15840 = DIRECTION ( 'NONE',  ( -2.958228394578794708E-31, 0.000000000000000000, 1.000000000000000000 ) ) ;
#15841 = B_SPLINE_SURFACE_WITH_KNOTS ( 'NONE', 3, 3, ( 
 ( #40497, #1746, #5581, #21236 ),
 ( #43822, #993, #36926, #47891 ),
 ( #9691, #736, #5336, #48640 ),
 ( #13531, #16380, #32049, #28192 ) ),
 .UNSPECIFIED., .F., .F., .F.,
 ( 4, 4 ),
 ( 4, 4 ),
 ( 0.000000000000000000, 1.000000000000000000 ),
 ( 0.000000000000000000, 1.000000000000000000 ),
 .UNSPECIFIED. ) ;
#15842 = ORIENTED_EDGE ( 'NONE', *, *, #1865, .F. ) ;
#15843 = VERTEX_POINT ( 'NONE', #34530 ) ;
#15844 = DIRECTION ( 'NONE',  ( 3.469446951953611231E-16, -0.000000000000000000, -1.000000000000000000 ) ) ;
#15845 = FACE_OUTER_BOUND ( 'NONE', #41627, .T. ) ;
#15846 = ORIENTED_EDGE ( 'NONE', *, *, #26779, .T. ) ;
#15847 = DIRECTION ( 'NONE',  ( -0.6805276818820436002, 0.4944323023722021482, 0.5407575913134970991 ) ) ;
#15848 = CARTESIAN_POINT ( 'NONE',  ( -45.35314062630780541, 8.244242869019066333, 8.807470649214881320 ) ) ;
#15849 = EDGE_CURVE ( 'NONE', #22918, #3086, #23491, .T. ) ;
#15850 = CARTESIAN_POINT ( 'NONE',  ( 0.5349929392774247505, 3.214704144639360717, 9.799351690761062272 ) ) ;
#15851 = ORIENTED_EDGE ( 'NONE', *, *, #42158, .T. ) ;
#15852 = LINE ( 'NONE', #11254, #42255 ) ;
#15853 = CARTESIAN_POINT ( 'NONE',  ( 9.999999999999994671, -1.084202172485504187E-16, 9.303249460322209785 ) ) ;
#15854 = EDGE_CURVE ( 'NONE', #8731, #14966, #30136, .T. ) ;
#15855 = ORIENTED_EDGE ( 'NONE', *, *, #49656, .T. ) ;
#15856 = EDGE_CURVE ( 'NONE', #750, #32832, #2529, .T. ) ;
#15857 = CARTESIAN_POINT ( 'NONE',  ( 343.9999999999999432, -185.0000000000001421, -360.0000000000003411 ) ) ;
#15858 = CARTESIAN_POINT ( 'NONE',  ( 183.0000000000000000, -268.4999999999999432, -339.9999999999998863 ) ) ;
#15859 = CIRCLE ( 'NONE', #26514, 2.000000000000001776 ) ;
#15860 = ORIENTED_EDGE ( 'NONE', *, *, #35999, .F. ) ;
#15861 = ORIENTED_EDGE ( 'NONE', *, *, #7758, .T. ) ;
#15862 = VERTEX_POINT ( 'NONE', #50628 ) ;
#15863 = LINE ( 'NONE', #46613, #43457 ) ;
#15864 = EDGE_CURVE ( 'NONE', #49857, #44495, #2326, .T. ) ;
#15865 = VECTOR ( 'NONE', #38873, 1000.000000000000000 ) ;
#15866 = ADVANCED_FACE ( 'NONE', ( #144 ), #31444, .T. ) ;
#15867 = DIRECTION ( 'NONE',  ( 0.000000000000000000, -0.000000000000000000, 1.000000000000000000 ) ) ;
#15868 = VERTEX_POINT ( 'NONE', #22713 ) ;
#15869 = VECTOR ( 'NONE', #10526, 1000.000000000000000 ) ;
#15870 = ADVANCED_FACE ( 'NONE', ( #15021 ), #694, .T. ) ;
#15871 = LINE ( 'NONE', #35141, #29092 ) ;
#15872 = LINE ( 'NONE', #19961, #24600 ) ;
#15873 = CARTESIAN_POINT ( 'NONE',  ( -45.64490844644706868, -21.32281559348764333, 8.807470649214879543 ) ) ;
#15874 = CARTESIAN_POINT ( 'NONE',  ( 339.9999999999998863, -174.9999999999999432, 355.9999999999998295 ) ) ;
#15875 = DIRECTION ( 'NONE',  ( 0.000000000000000000, 0.000000000000000000, 1.000000000000000000 ) ) ;
#15876 = CARTESIAN_POINT ( 'NONE',  ( 8.277096487746778308, -50.00000000000000711, 7.455576670931136185 ) ) ;
#15877 = CARTESIAN_POINT ( 'NONE',  ( -1.151763129092706617, 0.4096856258255360261, 9.987567862361069970 ) ) ;
#15878 = CARTESIAN_POINT ( 'NONE',  ( 155.0540265531850537, 2.143131898507880377E-16, -117.4317124430720725 ) ) ;
#15879 = CARTESIAN_POINT ( 'NONE',  ( -0.08756411783990718234, 1.703854692066548937, 9.912102921405034905 ) ) ;
#15880 = CARTESIAN_POINT ( 'NONE',  ( -86.69597344681496054, 0.000000000000000000, 165.0000000000000000 ) ) ;
#15881 = DIRECTION ( 'NONE',  ( -1.000000000000000000, 0.000000000000000000, -0.000000000000000000 ) ) ;
#15882 = CARTESIAN_POINT ( 'NONE',  ( 10.00000000000000178, -46.01315789473684248, -5.916985404131818171 ) ) ;
#15883 = LINE ( 'NONE', #11277, #43091 ) ;
#15884 = VECTOR ( 'NONE', #12151, 1000.000000000000000 ) ;
#15885 = EDGE_CURVE ( 'NONE', #43863, #37343, #18346, .T. ) ;
#15886 = PLANE ( 'NONE',  #12591 ) ;
#15887 = CARTESIAN_POINT ( 'NONE',  ( 339.9999999999998863, -185.0000000000001421, -344.0000000000001705 ) ) ;
#15888 = EDGE_LOOP ( 'NONE', ( #10766, #32418, #5704, #13816 ) ) ;
#15889 = DIRECTION ( 'NONE',  ( 1.000000000000000000, 0.000000000000000000, 0.000000000000000000 ) ) ;
#15890 = CARTESIAN_POINT ( 'NONE',  ( 85.00000000000029843, 17.00000000000000000, -60.00000000000000000 ) ) ;
#15891 = CARTESIAN_POINT ( 'NONE',  ( -0.9494396179258391966, 9.954826186926261755, 9.646707543097345905 ) ) ;
#15892 = PRODUCT_RELATED_PRODUCT_CATEGORY ( 'part', '', ( #9324 ) ) ;
#15893 = PLANE ( 'NONE',  #41844 ) ;
#15894 = B_SPLINE_CURVE_WITH_KNOTS ( 'NONE', 3,
 ( #46663, #11562, #32075, #27465 ),
 .UNSPECIFIED., .F., .F.,
 ( 4, 4 ),
 ( 0.000000000000000000, 0.0002520763768916294543 ),
 .UNSPECIFIED. ) ;
#15895 = ORIENTED_EDGE ( 'NONE', *, *, #33399, .F. ) ;
#15896 = FILL_AREA_STYLE ('',( #47903 ) ) ;
#15897 = EDGE_LOOP ( 'NONE', ( #13847, #3473, #48075 ) ) ;
#15898 = VECTOR ( 'NONE', #9217, 1000.000000000000000 ) ;
#15899 = CARTESIAN_POINT ( 'NONE',  ( 16.76006782980217125, -2.050259795448531541, 9.178419661560148768 ) ) ;
#15900 = AXIS2_PLACEMENT_3D ( 'NONE', #3270, #18917, #18665 ) ;
#15901 = ORIENTED_EDGE ( 'NONE', *, *, #50683, .T. ) ;
#15902 = DIRECTION ( 'NONE',  ( -1.000000000000000000, 1.331116318405244905E-23, 4.759647537211363479E-16 ) ) ;
#15903 = AXIS2_PLACEMENT_3D ( 'NONE', #19731, #5074, #28196 ) ;
#15905 = EDGE_CURVE ( 'NONE', #11040, #31210, #17044, .T. ) ;
#15904 = CARTESIAN_POINT ( 'NONE',  ( -1.249999999999999778, 0.000000000000000000, 9.972675548442463622 ) ) ;
#15906 = ORIENTED_EDGE ( 'NONE', *, *, #37617, .T. ) ;
#15907 = DIRECTION ( 'NONE',  ( -1.000000000000000000, 0.000000000000000000, -7.793956916774525800E-48 ) ) ;
#15908 = ORIENTED_EDGE ( 'NONE', *, *, #5481, .F. ) ;
#15909 = VECTOR ( 'NONE', #43848, 1000.000000000000000 ) ;
#15910 = ORIENTED_EDGE ( 'NONE', *, *, #28156, .T. ) ;
#15911 = DIRECTION ( 'NONE',  ( -0.000000000000000000, -1.000000000000000000, -0.000000000000000000 ) ) ;
#15912 = DIRECTION ( 'NONE',  ( -1.000000000000000000, 0.000000000000000000, 0.000000000000000000 ) ) ;
#15913 = ORIENTED_EDGE ( 'NONE', *, *, #28619, .F. ) ;
#15914 = CARTESIAN_POINT ( 'NONE',  ( 0.9342145181057528447, 1.950058884269514126, 9.882709995651168811 ) ) ;
#15915 = DIRECTION ( 'NONE',  ( -1.000000000000000000, 0.000000000000000000, 0.000000000000000000 ) ) ;
#15916 = CARTESIAN_POINT ( 'NONE',  ( 164.9999999999999716, 16.00000000000000000, -54.99999999999999289 ) ) ;
#15917 = ORIENTED_EDGE ( 'NONE', *, *, #42536, .T. ) ;
#15918 = CARTESIAN_POINT ( 'NONE',  ( -42.99990394833793061, 47.95759300784327905, 5.000000000000000000 ) ) ;
#15919 = CARTESIAN_POINT ( 'NONE',  ( 85.00000000000029843, 16.00000000000000000, -60.00000000000000000 ) ) ;
#15920 = ADVANCED_FACE ( 'NONE', ( #4985 ), #13190, .T. ) ;
#15921 = CIRCLE ( 'NONE', #35609, 2.000000000000001776 ) ;
#15922 = VERTEX_POINT ( 'NONE', #1155 ) ;
#15923 = ADVANCED_FACE ( 'NONE', ( #44470 ), #12929, .F. ) ;
#15924 = DIRECTION ( 'NONE',  ( 0.000000000000000000, 0.000000000000000000, -1.000000000000000000 ) ) ;
#15925 = CARTESIAN_POINT ( 'NONE',  ( 153.3040265531850537, -1.750000000000010214, 40.81828755692798438 ) ) ;
#15926 = SHAPE_REPRESENTATION ( 'hopper', ( #45486 ), #11091 ) ;
#15927 = ORIENTED_EDGE ( 'NONE', *, *, #33702, .T. ) ;
#15928 = CARTESIAN_POINT ( 'NONE',  ( 181.0000000000000284, 2.775557561562891351E-14, -115.0000000000001563 ) ) ;
#15929 = EDGE_CURVE ( 'NONE', #35915, #8390, #7580, .T. ) ;
#15930 = DIRECTION ( 'NONE',  ( 0.000000000000000000, 1.000000000000000000, -2.969158215481698263E-48 ) ) ;
#15931 = ORIENTED_EDGE ( 'NONE', *, *, #25258, .T. ) ;
#15932 = CARTESIAN_POINT ( 'NONE',  ( 34.08406891383362591, -15.63733501198463038, -8.192531242611266862 ) ) ;
#15933 = EDGE_CURVE ( 'NONE', #13539, #44183, #47840, .T. ) ;
#15934 = DIRECTION ( 'NONE',  ( 0.000000000000000000, -1.000000000000000000, 0.000000000000000000 ) ) ;
#15935 = CARTESIAN_POINT ( 'NONE',  ( -4.945973446814903696, 2.143131898507912917E-16, -117.4317124430720156 ) ) ;
#15936 = ADVANCED_FACE ( 'NONE', ( #642 ), #4783, .T. ) ;
#15937 = CARTESIAN_POINT ( 'NONE',  ( -5.670847180967843570, 1.750000000000023315, 39.79316129108089228 ) ) ;
#15938 = ORIENTED_EDGE ( 'NONE', *, *, #32856, .F. ) ;
#15939 = VECTOR ( 'NONE', #42151, 1000.000000000000000 ) ;
#15940 = CARTESIAN_POINT ( 'NONE',  ( -84.94597344681494633, 2.143131898507880377E-16, -160.9317124430720014 ) ) ;
#15941 = CARTESIAN_POINT ( 'NONE',  ( 44.99506233596247995, 23.32283626942318833, 7.455576670931136185 ) ) ;
#15942 = VECTOR ( 'NONE', #35425, 1000.000000000000000 ) ;
#15943 = ADVANCED_FACE ( 'NONE', ( #39647 ), #35111, .T. ) ;
#15944 = FACE_OUTER_BOUND ( 'NONE', #120, .T. ) ;
#15945 = ORIENTED_EDGE ( 'NONE', *, *, #26236, .F. ) ;
#15946 = VECTOR ( 'NONE', #9054, 1000.000000000000000 ) ;
#15947 = EDGE_LOOP ( 'NONE', ( #28953, #14070, #34398, #18174 ) ) ;
#15948 = DIRECTION ( 'NONE',  ( 0.000000000000000000, 0.000000000000000000, 1.000000000000000000 ) ) ;
#15949 = DIRECTION ( 'NONE',  ( 0.000000000000000000, 0.000000000000000000, -1.000000000000000000 ) ) ;
#15950 = CARTESIAN_POINT ( 'NONE',  ( 30.00000000000092726, 17.00000000000000000, -24.99999999999999289 ) ) ;
#15951 = CARTESIAN_POINT ( 'NONE',  ( -204.9459734468148895, 1.025126265847089435, -40.93171244307204404 ) ) ;
#15952 = CARTESIAN_POINT ( 'NONE',  ( 1.104609456715839766, 0.6504863887005235545, 9.948547179989622791 ) ) ;
#15953 = ORIENTED_EDGE ( 'NONE', *, *, #6106, .F. ) ;
#15954 = CARTESIAN_POINT ( 'NONE',  ( 339.9999999999999432, -180.9999999999999432, 355.9999999999998295 ) ) ;
#15955 = CARTESIAN_POINT ( 'NONE',  ( 6.010192544690008631, -37.05120237258827132, 4.835783797351798974 ) ) ;
#15956 = SURFACE_STYLE_USAGE ( .BOTH. , #11604 ) ;
#15957 = ORIENTED_EDGE ( 'NONE', *, *, #30989, .T. ) ;
#15958 = VECTOR ( 'NONE', #39304, 1000.000000000000000 ) ;
#15959 = FACE_OUTER_BOUND ( 'NONE', #33853, .T. ) ;
#15960 = VERTEX_POINT ( 'NONE', #10098 ) ;
#15961 = AXIS2_PLACEMENT_3D ( 'NONE', #30094, #45951, #11087 ) ;
#15962 = B_SPLINE_CURVE_WITH_KNOTS ( 'NONE', 3,
 ( #7619, #24031, #39940, #3760 ),
 .UNSPECIFIED., .F., .F.,
 ( 4, 4 ),
 ( 5.776111876705087994E-18, 0.0004301978946275169255 ),
 .UNSPECIFIED. ) ;
#15963 = EDGE_LOOP ( 'NONE', ( #32903, #50244, #15739, #27600 ) ) ;
#15964 = CARTESIAN_POINT ( 'NONE',  ( -1.011271242968688533, 0.7347315653655859258, 10.00000000000000000 ) ) ;
#15965 = CARTESIAN_POINT ( 'NONE',  ( 343.9999999999999432, -183.0000000000001421, -358.0000000000003411 ) ) ;
#15966 = CARTESIAN_POINT ( 'NONE',  ( 349.9999999999999432, -168.9999999999999432, 355.9999999999997726 ) ) ;
#15967 = LINE ( 'NONE', #31634, #21431 ) ;
#15968 = ORIENTED_EDGE ( 'NONE', *, *, #42607, .T. ) ;
#15969 = EDGE_CURVE ( 'NONE', #26234, #43085, #2645, .T. ) ;
#15970 = PLANE ( 'NONE',  #47412 ) ;
#15971 = DIRECTION ( 'NONE',  ( 0.000000000000000000, 0.000000000000000000, -1.000000000000000000 ) ) ;
#15972 = VERTEX_POINT ( 'NONE', #37075 ) ;
#15973 = CARTESIAN_POINT ( 'NONE',  ( -5.000000000000000000, 184.8000000000000114, -340.2000000000001592 ) ) ;
#15974 = VECTOR ( 'NONE', #34598, 1000.000000000000000 ) ;
#15975 = CARTESIAN_POINT ( 'NONE',  ( 224.9999999999999432, -175.0000000000000000, 32.29650858650035161 ) ) ;
#15976 = CYLINDRICAL_SURFACE ( 'NONE', #31981, 1.750000000000008438 ) ;
#15977 = ORIENTED_EDGE ( 'NONE', *, *, #40688, .F. ) ;
#15978 = ORIENTED_EDGE ( 'NONE', *, *, #5106, .T. ) ;
#15979 = LINE ( 'NONE', #31650, #18524 ) ;
#15980 = CIRCLE ( 'NONE', #18414, 1.750000000000008438 ) ;
#15981 =( BOUNDED_CURVE ( )  B_SPLINE_CURVE ( 3, ( #3384, #30604, #19036, #46205 ),
 .UNSPECIFIED., .F., .F. ) 
 B_SPLINE_CURVE_WITH_KNOTS ( ( 4, 4 ),
 ( 1.570796326794896558, 3.141592653589793116 ),
 .UNSPECIFIED. ) 
 CURVE ( )  GEOMETRIC_REPRESENTATION_ITEM ( )  RATIONAL_B_SPLINE_CURVE ( ( 1.000000000000000000, 0.8047378541243649375, 0.8047378541243649375, 1.000000000000000000 ) ) 
 REPRESENTATION_ITEM ( '' )  );
#15982 = ORIENTED_EDGE ( 'NONE', *, *, #31550, .T. ) ;
#15983 = ADVANCED_FACE ( 'NONE', ( #30111 ), #5740, .F. ) ;
#15984 = DIRECTION ( 'NONE',  ( -0.000000000000000000, -1.000000000000000000, -0.000000000000000000 ) ) ;
#15985 = CARTESIAN_POINT ( 'NONE',  ( 195.0540265531851105, 2.143131898507880377E-16, -0.9317124430720247208 ) ) ;
#15986 = DIRECTION ( 'NONE',  ( -1.000000000000000000, -0.000000000000000000, -0.000000000000000000 ) ) ;
#15987 = ORIENTED_EDGE ( 'NONE', *, *, #2761, .T. ) ;
#15988 = CARTESIAN_POINT ( 'NONE',  ( 0.1425549192113746144, -1.238581250503543618, 9.981352469109934233 ) ) ;
#15989 = VERTEX_POINT ( 'NONE', #18041 ) ;
#15990 =( BOUNDED_CURVE ( )  B_SPLINE_CURVE ( 3, ( #21320, #14114, #29277, #41328 ),
 .UNSPECIFIED., .F., .F. ) 
 B_SPLINE_CURVE_WITH_KNOTS ( ( 4, 4 ),
 ( 0.000000000000000000, 1.570796326794896558 ),
 .UNSPECIFIED. ) 
 CURVE ( )  GEOMETRIC_REPRESENTATION_ITEM ( )  RATIONAL_B_SPLINE_CURVE ( ( 1.000000000000000000, 0.8047378541243649375, 0.8047378541243649375, 1.000000000000000000 ) ) 
 REPRESENTATION_ITEM ( '' )  );
#15991 = ORIENTED_EDGE ( 'NONE', *, *, #19352, .F. ) ;
#15992 = DIRECTION ( 'NONE',  ( -1.000000000000000000, -0.000000000000000000, -0.000000000000000000 ) ) ;
#15993 = EDGE_CURVE ( 'NONE', #19838, #38709, #13445, .T. ) ;
#15994 = EDGE_CURVE ( 'NONE', #37254, #4263, #41142, .T. ) ;
#15995 = DIRECTION ( 'NONE',  ( 3.614007241618348278E-16, 1.000000000000000000, 0.000000000000000000 ) ) ;
#15996 = VECTOR ( 'NONE', #50278, 1000.000000000000000 ) ;
#15997 = ORIENTED_EDGE ( 'NONE', *, *, #32162, .F. ) ;
#15998 = ORIENTED_EDGE ( 'NONE', *, *, #9516, .T. ) ;
#15999 = ORIENTED_EDGE ( 'NONE', *, *, #47287, .F. ) ;
#16000 = VECTOR ( 'NONE', #33063, 1000.000000000000000 ) ;
#16001 = CARTESIAN_POINT ( 'NONE',  ( 210.0000000000000568, 2.143131898507881116E-16, -40.93171244307203693 ) ) ;
#16002 = EDGE_CURVE ( 'NONE', #14561, #31607, #11184, .T. ) ;
#16003 = LINE ( 'NONE', #9060, #26700 ) ;
#16004 =( BOUNDED_CURVE ( )  B_SPLINE_CURVE ( 3, ( #29177, #18114, #33787, #44792 ),
 .UNSPECIFIED., .F., .F. ) 
 B_SPLINE_CURVE_WITH_KNOTS ( ( 4, 4 ),
 ( 4.712388980384689674, 6.283185307179586232 ),
 .UNSPECIFIED. ) 
 CURVE ( )  GEOMETRIC_REPRESENTATION_ITEM ( )  RATIONAL_B_SPLINE_CURVE ( ( 1.000000000000000000, 0.8047378541243649375, 0.8047378541243649375, 1.000000000000000000 ) ) 
 REPRESENTATION_ITEM ( '' )  );
#16005 = PRODUCT_DEFINITION_CONTEXT ( 'detailed design', #35511, 'design' ) ;
#16006 = VERTEX_POINT ( 'NONE', #29857 ) ;
#16007 = CARTESIAN_POINT ( 'NONE',  ( -128.4459734468149179, 0.000000000000000000, 165.0000000000000000 ) ) ;
#16008 = EDGE_LOOP ( 'NONE', ( #22004, #11307, #32065, #12636 ) ) ;
#16009 = CARTESIAN_POINT ( 'NONE',  ( 9.386495789655688426, 3.489743738556303487, 6.429802539306412434 ) ) ;
#16010 = VERTEX_POINT ( 'NONE', #49049 ) ;
#16011 = CARTESIAN_POINT ( 'NONE',  ( 340.0000000000000568, 169.0000000000000000, 349.9999999999998295 ) ) ;
#16012 = DIRECTION ( 'NONE',  ( -1.000000000000000000, -0.000000000000000000, -0.000000000000000000 ) ) ;
#16013 = AXIS2_PLACEMENT_3D ( 'NONE', #25472, #10071, #37306 ) ;
#16014 = CARTESIAN_POINT ( 'NONE',  ( 33.30402655318503946, 1.750000000000009992, 160.8182875569279702 ) ) ;
#16015 = CARTESIAN_POINT ( 'NONE',  ( 224.9999999999999716, -164.9999999999999716, 474.9999999999998863 ) ) ;
#16016 = DIRECTION ( 'NONE',  ( -1.000000000000000000, 0.000000000000000000, 0.000000000000000000 ) ) ;
#16017 = CIRCLE ( 'NONE', #24223, 2.000000000000001776 ) ;
#16018 = CARTESIAN_POINT ( 'NONE',  ( 1.158497635116737312, -16.61944452314319420, -3.546734833711462365 ) ) ;
#16019 = VERTEX_POINT ( 'NONE', #18283 ) ;
#16020 = ORIENTED_EDGE ( 'NONE', *, *, #14872, .F. ) ;
#16021 = CARTESIAN_POINT ( 'NONE',  ( 191.5540265531851105, 0.000000000000000000, 165.0000000000000000 ) ) ;
#16022 = AXIS2_PLACEMENT_3D ( 'NONE', #3624, #19270, #27744 ) ;
#16023 = FACE_OUTER_BOUND ( 'NONE', #16245, .T. ) ;
#16024 = CYLINDRICAL_SURFACE ( 'NONE', #47962, 1.750000000000001554 ) ;
#16025 = VECTOR ( 'NONE', #13529, 1000.000000000000000 ) ;
#16026 = CARTESIAN_POINT ( 'NONE',  ( 177.5000000000000284, 112.5000000000000000, -10.00000000000000000 ) ) ;
#16027 = LINE ( 'NONE', #42440, #46630 ) ;
#16028 = VERTEX_POINT ( 'NONE', #21911 ) ;
#16029 = DIRECTION ( 'NONE',  ( -1.000000000000000000, -6.344131455081961406E-16, 4.759647537211363479E-16 ) ) ;
#16030 = DIRECTION ( 'NONE',  ( -1.000000000000000000, -0.000000000000000000, -0.000000000000000000 ) ) ;
#16031 = ADVANCED_FACE ( 'NONE', ( #21646 ), #47347, .T. ) ;
#16032 = VERTEX_POINT ( 'NONE', #1654 ) ;
#16033 = VECTOR ( 'NONE', #36817, 1000.000000000000000 ) ;
#16034 = CARTESIAN_POINT ( 'NONE',  ( 4.672045878990125800, -33.19353511768168374, 1.847720168420772691 ) ) ;
#16035 = VECTOR ( 'NONE', #13702, 1000.000000000000000 ) ;
#16036 = DIRECTION ( 'NONE',  ( 0.000000000000000000, -3.186989995019654210E-49, -1.000000000000000000 ) ) ;
#16037 = CARTESIAN_POINT ( 'NONE',  ( 356.0000000000000000, -164.9999999999999432, 339.9999999999998295 ) ) ;
#16038 = AXIS2_PLACEMENT_3D ( 'NONE', #41117, #12651, #1124 ) ;
#16039 = EDGE_LOOP ( 'NONE', ( #3029, #1541, #38943, #21564 ) ) ;
#16040 = EDGE_LOOP ( 'NONE', ( #42923, #23853, #38692 ) ) ;
#16041 = LINE ( 'NONE', #31953, #499 ) ;
#16042 = CARTESIAN_POINT ( 'NONE',  ( 6.508636631827673824, 15.75743548351451295, 8.953103998512858652 ) ) ;
#16043 = VECTOR ( 'NONE', #35383, 1000.000000000000000 ) ;
#16044 = VERTEX_POINT ( 'NONE', #9598 ) ;
#16045 = ORIENTED_EDGE ( 'NONE', *, *, #46519, .T. ) ;
#16046 = DIRECTION ( 'NONE',  ( 1.000000000000000000, 0.000000000000000000, 0.000000000000000000 ) ) ;
#16047 = CARTESIAN_POINT ( 'NONE',  ( 12.35406723005396046, -11.51001571518080624, 9.178419661560148768 ) ) ;
#16048 = CARTESIAN_POINT ( 'NONE',  ( 151.5540265531850537, 0.000000000000000000, 79.06828755692797017 ) ) ;
#16049 = DIRECTION ( 'NONE',  ( -1.586032880504786307E-16, 1.654361225106055350E-24, -1.000000000000000000 ) ) ;
#16050 = AXIS2_PLACEMENT_3D ( 'NONE', #27296, #38092, #23181 ) ;
#16051 = VERTEX_POINT ( 'NONE', #10363 ) ;
#16052 = VERTEX_POINT ( 'NONE', #48549 ) ;
#16053 = ORIENTED_EDGE ( 'NONE', *, *, #27884, .T. ) ;
#16054 = CIRCLE ( 'NONE', #17692, 1.750000000000001554 ) ;
#16055 = VECTOR ( 'NONE', #41713, 1000.000000000000000 ) ;
#16056 = CARTESIAN_POINT ( 'NONE',  ( 71.55402655318505367, 0.000000000000000000, 42.56828755692799859 ) ) ;
#16057 = VERTEX_POINT ( 'NONE', #33222 ) ;
#16058 = LINE ( 'NONE', #47054, #6604 ) ;
#16059 = ORIENTED_EDGE ( 'NONE', *, *, #17486, .F. ) ;
#16060 = ORIENTED_EDGE ( 'NONE', *, *, #3608, .F. ) ;
#16061 = CARTESIAN_POINT ( 'NONE',  ( -8.445973446814976526, 0.000000000000000000, 82.56828755692801280 ) ) ;
#16062 = EDGE_CURVE ( 'NONE', #30045, #3402, #22204, .T. ) ;
#16063 = CARTESIAN_POINT ( 'NONE',  ( -239.0000000000000853, -165.6999999999999602, 254.8599999999999852 ) ) ;
#16064 = CARTESIAN_POINT ( 'NONE',  ( 339.9999999999999432, -180.9999999999999716, -342.0000000000001705 ) ) ;
#16065 = VERTEX_POINT ( 'NONE', #14184 ) ;
#16066 = ORIENTED_EDGE ( 'NONE', *, *, #26219, .T. ) ;
#16067 = CARTESIAN_POINT ( 'NONE',  ( -0.1287570809895576818, -0.3962735484563154609, 10.00000000000000000 ) ) ;
#16068 = ORIENTED_EDGE ( 'NONE', *, *, #25027, .F. ) ;
#16069 = FACE_OUTER_BOUND ( 'NONE', #2535, .T. ) ;
#16070 = CARTESIAN_POINT ( 'NONE',  ( 0.000000000000000000, 0.000000000000000000, -5.000000000000000000 ) ) ;
#16071 = CARTESIAN_POINT ( 'NONE',  ( 166.9999999999999716, -93.49999999999997158, -115.0000000000001563 ) ) ;
#16072 = LINE ( 'NONE', #15564, #6907 ) ;
#16073 = VECTOR ( 'NONE', #14466, 1000.000000000000000 ) ;
#16074 = ORIENTED_EDGE ( 'NONE', *, *, #24934, .T. ) ;
#16075 = LINE ( 'NONE', #4016, #25859 ) ;
#16076 = DIRECTION ( 'NONE',  ( 4.759647537211363479E-16, -5.772796816983493182E-42, 1.000000000000000000 ) ) ;
#16077 = LINE ( 'NONE', #22994, #49771 ) ;
#16078 = DIRECTION ( 'NONE',  ( 1.000000000000000000, 0.000000000000000000, 0.000000000000000000 ) ) ;
#16079 = CIRCLE ( 'NONE', #27552, 2.000000000000001776 ) ;
#16080 = VECTOR ( 'NONE', #20539, 1000.000000000000000 ) ;
#16081 = FACE_OUTER_BOUND ( 'NONE', #29186, .T. ) ;
#16082 = CARTESIAN_POINT ( 'NONE',  ( -6.174150299305392053, 50.00000000000000711, 8.807470649214879543 ) ) ;
#16083 = EDGE_CURVE ( 'NONE', #46160, #11740, #33465, .T. ) ;
#16084 = CARTESIAN_POINT ( 'NONE',  ( 195.0540265531851105, 2.143131898507880377E-16, -160.9317124430720014 ) ) ;
#16085 = VECTOR ( 'NONE', #30816, 1000.000000000000000 ) ;
#16086 = ORIENTED_EDGE ( 'NONE', *, *, #33873, .T. ) ;
#16087 = FACE_OUTER_BOUND ( 'NONE', #40191, .T. ) ;
#16088 = CARTESIAN_POINT ( 'NONE',  ( 195.0540265531851105, 2.143131898507880377E-16, 162.5682875569279702 ) ) ;
#16089 = VERTEX_POINT ( 'NONE', #21388 ) ;
#16090 = LINE ( 'NONE', #43780, #14068 ) ;
#16091 = CARTESIAN_POINT ( 'NONE',  ( -5.647304616913629616, 53.53801056904005407, 22.84256005001721945 ) ) ;
#16092 = DIRECTION ( 'NONE',  ( -1.000000000000000000, 0.000000000000000000, 1.860490536778032451E-50 ) ) ;
#16093 = VERTEX_POINT ( 'NONE', #17550 ) ;
#16094 = DIRECTION ( 'NONE',  ( 0.000000000000000000, 1.000000000000000000, 0.000000000000000000 ) ) ;
#16095 = ORIENTED_EDGE ( 'NONE', *, *, #5158, .T. ) ;
#16096 = ORIENTED_EDGE ( 'NONE', *, *, #3239, .F. ) ;
#16097 = CARTESIAN_POINT ( 'NONE',  ( 47.87295225382209907, 14.46560184742433641, -2.408242355805840784 ) ) ;
#16098 = B_SPLINE_CURVE_WITH_KNOTS ( 'NONE', 3,
 ( #20924, #13216, #39934, #12460 ),
 .UNSPECIFIED., .F., .F.,
 ( 4, 4 ),
 ( 0.001937412222931639196, 0.003978261222106111578 ),
 .UNSPECIFIED. ) ;
#16099 = CARTESIAN_POINT ( 'NONE',  ( 195.0540265531851105, 2.143131898507880377E-16, -80.93171244307201562 ) ) ;
#16100 = AXIS2_PLACEMENT_3D ( 'NONE', #24947, #9779, #44658 ) ;
#16101 = ORIENTED_EDGE ( 'NONE', *, *, #2771, .T. ) ;
#16102 = DIRECTION ( 'NONE',  ( -0.000000000000000000, -0.000000000000000000, -1.000000000000000000 ) ) ;
#16103 = LINE ( 'NONE', #27912, #8545 ) ;
#16104 = AXIS2_PLACEMENT_3D ( 'NONE', #6703, #15168, #18240 ) ;
#16105 = ORIENTED_EDGE ( 'NONE', *, *, #24275, .F. ) ;
#16106 = CARTESIAN_POINT ( 'NONE',  ( 1.780432407520001536, 1.041450996408479046, 9.894754715216729224 ) ) ;
#16107 = ORIENTED_EDGE ( 'NONE', *, *, #24683, .F. ) ;
#16108 = CARTESIAN_POINT ( 'NONE',  ( 210.0000000000000568, 0.000000000000000000, -79.18171244307201562 ) ) ;
#16109 = CARTESIAN_POINT ( 'NONE',  ( 115.0540265531850395, 2.143131898507847836E-16, 122.5682875569279560 ) ) ;
#16110 = LINE ( 'NONE', #31775, #44690 ) ;
#16111 = AXIS2_PLACEMENT_3D ( 'NONE', #43616, #43871, #39542 ) ;
#16112 = EDGE_CURVE ( 'NONE', #953, #47880, #29597, .T. ) ;
#16113 = VERTEX_POINT ( 'NONE', #48806 ) ;
#16114 = EDGE_CURVE ( 'NONE', #33352, #20660, #6499, .T. ) ;
#16115 = FACE_OUTER_BOUND ( 'NONE', #27253, .T. ) ;
#16116 = CARTESIAN_POINT ( 'NONE',  ( 358.3431457505075741, -185.0000000000001137, 360.0000000000000000 ) ) ;
#16117 = ORIENTED_EDGE ( 'NONE', *, *, #5224, .F. ) ;
#16118 = VERTEX_POINT ( 'NONE', #11625 ) ;
#16119 = ORIENTED_EDGE ( 'NONE', *, *, #50555, .T. ) ;
#16120 = FACE_OUTER_BOUND ( 'NONE', #5353, .T. ) ;
#16121 = EDGE_CURVE ( 'NONE', #24878, #23700, #30365, .T. ) ;
#16122 = CARTESIAN_POINT ( 'NONE',  ( 0.000000000000000000, -389.0218519071287346, 192.5658166940287970 ) ) ;
#16123 = ORIENTED_EDGE ( 'NONE', *, *, #15505, .F. ) ;
#16124 = EDGE_CURVE ( 'NONE', #44732, #37243, #37789, .T. ) ;
#16125 = AXIS2_PLACEMENT_3D ( 'NONE', #24135, #12309, #39782 ) ;
#16126 = DIRECTION ( 'NONE',  ( 0.000000000000000000, -1.000000000000000000, 1.822804496942679766E-16 ) ) ;
#16127 = CARTESIAN_POINT ( 'NONE',  ( 168.9999999999999716, -272.5000000000000000, -98.99999999999990052 ) ) ;
#16128 = CARTESIAN_POINT ( 'NONE',  ( -0.1287570809895632329, 0.3962735484563137400, 10.00000000000000000 ) ) ;
#16129 = EDGE_CURVE ( 'NONE', #18208, #14529, #96, .T. ) ;
#16130 = FACE_OUTER_BOUND ( 'NONE', #27477, .T. ) ;
#16131 = CARTESIAN_POINT ( 'NONE',  ( -168.4459734468149747, -1.025126265847089435, -157.4317124430720582 ) ) ;
#16132 = DIRECTION ( 'NONE',  ( -0.000000000000000000, -0.000000000000000000, -1.000000000000000000 ) ) ;
#16133 = CARTESIAN_POINT ( 'NONE',  ( -204.9459734468148895, 1.025126265847089657, -80.93171244307201562 ) ) ;
#16134 = CARTESIAN_POINT ( 'NONE',  ( -25.79500241909648395, 0.000000000000000000, 0.000000000000000000 ) ) ;
#16135 = DIRECTION ( 'NONE',  ( -1.000000000000000000, 0.000000000000000000, 0.000000000000000000 ) ) ;
#16136 = LINE ( 'NONE', #45686, #4771 ) ;
#16137 = LINE ( 'NONE', #43823, #43727 ) ;
#16138 = DIRECTION ( 'NONE',  ( 0.000000000000000000, 2.969158215481698263E-48, -1.000000000000000000 ) ) ;
#16140 = B_SPLINE_CURVE_WITH_KNOTS ( 'NONE', 3,
 ( #3346, #33910, #14398, #45668 ),
 .UNSPECIFIED., .F., .F.,
 ( 4, 4 ),
 ( 0.9688112071879405596, 0.9724175925769215079 ),
 .UNSPECIFIED. ) ;
#16139 = AXIS2_PLACEMENT_3D ( 'NONE', #34544, #49865, #46039 ) ;
#16141 = LINE ( 'NONE', #47385, #10913 ) ;
#16142 = VERTEX_POINT ( 'NONE', #18544 ) ;
#16143 = DIRECTION ( 'NONE',  ( -0.000000000000000000, -0.000000000000000000, -1.000000000000000000 ) ) ;
#16144 =( BOUNDED_CURVE ( )  B_SPLINE_CURVE ( 3, ( #37514, #21075, #44898, #36760 ),
 .UNSPECIFIED., .F., .F. ) 
 B_SPLINE_CURVE_WITH_KNOTS ( ( 4, 4 ),
 ( 0.000000000000000000, 1.570796326794896558 ),
 .UNSPECIFIED. ) 
 CURVE ( )  GEOMETRIC_REPRESENTATION_ITEM ( )  RATIONAL_B_SPLINE_CURVE ( ( 1.000000000000000000, 0.8047378541243649375, 0.8047378541243649375, 1.000000000000000000 ) ) 
 REPRESENTATION_ITEM ( '' )  );
#16145 = FACE_OUTER_BOUND ( 'NONE', #632, .T. ) ;
#16146 = DIRECTION ( 'NONE',  ( 8.673617379884028076E-17, -1.000000000000000000, 0.000000000000000000 ) ) ;
#16147 = EDGE_CURVE ( 'NONE', #11134, #11547, #32567, .T. ) ;
#16148 = EDGE_CURVE ( 'NONE', #29772, #8852, #14964, .T. ) ;
#16149 = CARTESIAN_POINT ( 'NONE',  ( -49.89397392339119364, 8.245536726717011433, 7.906207997025717304 ) ) ;
#16151 = EDGE_LOOP ( 'NONE', ( #34822, #50305, #38321, #15302 ) ) ;
#16150 = EDGE_CURVE ( 'NONE', #11655, #28510, #46726, .T. ) ;
#16152 = CARTESIAN_POINT ( 'NONE',  ( -0.7601424845489993531, 1.297311920617006065, 9.927319414211224213 ) ) ;
#16153 = EDGE_CURVE ( 'NONE', #16517, #15399, #10852, .T. ) ;
#16154 = ORIENTED_EDGE ( 'NONE', *, *, #30709, .F. ) ;
#16155 = DIRECTION ( 'NONE',  ( 0.000000000000000000, 5.664403186863042467E-17, 1.000000000000000000 ) ) ;
#16156 = ORIENTED_EDGE ( 'NONE', *, *, #42903, .F. ) ;
#16157 = ADVANCED_FACE ( 'NONE', ( #3662 ), #30618, .T. ) ;
#16158 = CARTESIAN_POINT ( 'NONE',  ( -164.9459734468149463, 2.143131898507880377E-16, -77.43171244307204404 ) ) ;
#16159 = CARTESIAN_POINT ( 'NONE',  ( 0.7601424845489945792, -1.297311920616997627, 9.927319414211225990 ) ) ;
#16160 = DIRECTION ( 'NONE',  ( -0.000000000000000000, -1.000000000000000000, 2.537652627714643577E-15 ) ) ;
#16161 = EDGE_CURVE ( 'NONE', #34526, #16183, #41721, .T. ) ;
#16162 = ORIENTED_EDGE ( 'NONE', *, *, #15820, .T. ) ;
#16163 = CARTESIAN_POINT ( 'NONE',  ( 31.55402655318503236, 0.000000000000000000, 165.0000000000000000 ) ) ;
#16164 = ORIENTED_EDGE ( 'NONE', *, *, #12224, .T. ) ;
#16165 = CIRCLE ( 'NONE', #9597, 4.000000000000003553 ) ;
#16166 = VERTEX_POINT ( 'NONE', #19052 ) ;
#16167 = LINE ( 'NONE', #43343, #18813 ) ;
#16168 = CARTESIAN_POINT ( 'NONE',  ( -64.99999999999971578, 17.00000000000000000, -60.00000000000000000 ) ) ;
#16169 =( REPRESENTATION_RELATIONSHIP ('NONE','NONE', #45699, #50327 ) REPRESENTATION_RELATIONSHIP_WITH_TRANSFORMATION ( #37728 )SHAPE_REPRESENTATION_RELATIONSHIP( ) );
#16170 = VERTEX_POINT ( 'NONE', #22654 ) ;
#16171 = PLANE ( 'NONE',  #18031 ) ;
#16172 = DIRECTION ( 'NONE',  ( -1.000000000000000000, 0.000000000000000000, 0.000000000000000000 ) ) ;
#16173 = PLANE ( 'NONE',  #46171 ) ;
#16174 = PLANE ( 'NONE',  #16125 ) ;
#16175 = EDGE_CURVE ( 'NONE', #31056, #12217, #20916, .T. ) ;
#16176 = DIRECTION ( 'NONE',  ( 1.000000000000000000, 0.000000000000000000, -4.758098676964956461E-16 ) ) ;
#16177 = EDGE_CURVE ( 'NONE', #10936, #13504, #9928, .T. ) ;
#16178 = EDGE_LOOP ( 'NONE', ( #8104, #24748, #39333, #44182 ) ) ;
#16179 = AXIS2_PLACEMENT_3D ( 'NONE', #31027, #11266, #4328 ) ;
#16180 = EDGE_CURVE ( 'NONE', #9118, #20525, #49779, .T. ) ;
#16181 = CARTESIAN_POINT ( 'NONE',  ( -0.3862712429686895876, 1.188820645368940720, 10.00000000000000000 ) ) ;
#16182 = CARTESIAN_POINT ( 'NONE',  ( 185.0000000000000000, -272.4999999999999432, -356.0000000000001705 ) ) ;
#16183 = VERTEX_POINT ( 'NONE', #31127 ) ;
#16184 = DIRECTION ( 'NONE',  ( 0.000000000000000000, 0.000000000000000000, -1.000000000000000000 ) ) ;
#16185 = DIRECTION ( 'NONE',  ( -1.000000000000000000, 0.000000000000000000, 0.000000000000000000 ) ) ;
#16186 = ORIENTED_EDGE ( 'NONE', *, *, #19252, .F. ) ;
#16187 = CARTESIAN_POINT ( 'NONE',  ( 151.5540265531850537, 0.000000000000000000, 165.0000000000000000 ) ) ;
#16188 = CYLINDRICAL_SURFACE ( 'NONE', #42954, 4.000000000000003553 ) ;
#16189 = FACE_OUTER_BOUND ( 'NONE', #18757, .T. ) ;
#16190 = CARTESIAN_POINT ( 'NONE',  ( 71.55402655318505367, -1.025126265847089657, -120.9317124430720440 ) ) ;
#16191 = ORIENTED_EDGE ( 'NONE', *, *, #43724, .F. ) ;
#16192 = DIRECTION ( 'NONE',  ( 1.000000000000000000, 0.000000000000000000, -0.000000000000000000 ) ) ;
#16193 = CARTESIAN_POINT ( 'NONE',  ( 15.00099850811936264, 7.462898891544210933, 9.403735324607438884 ) ) ;
#16194 = EDGE_CURVE ( 'NONE', #566, #44892, #1737, .T. ) ;
#16195 = CARTESIAN_POINT ( 'NONE',  ( 7.241383964640743187, 3.469446951953614189E-15, -5.000000000000000000 ) ) ;
#16196 = ORIENTED_EDGE ( 'NONE', *, *, #39084, .T. ) ;
#16197 = VERTEX_POINT ( 'NONE', #27278 ) ;
#16198 = DIRECTION ( 'NONE',  ( -1.604966159973741924E-14, 0.1191452206184306778, -0.9928768384869218755 ) ) ;
#16199 = DIRECTION ( 'NONE',  ( 1.000000000000000000, 0.000000000000000000, 0.000000000000000000 ) ) ;
#16200 = CARTESIAN_POINT ( 'NONE',  ( -9.260964247899874380, 13.84230907185616744, -9.683996418299976483 ) ) ;
#16201 = EDGE_CURVE ( 'NONE', #4028, #921, #22907, .T. ) ;
#16202 = CARTESIAN_POINT ( 'NONE',  ( 28.52604530808654815, 41.07801380285680892, -3.760136334089591248 ) ) ;
#16203 = ORIENTED_EDGE ( 'NONE', *, *, #9155, .T. ) ;
#16204 = LINE ( 'NONE', #43635, #14060 ) ;
#16205 = B_SPLINE_CURVE_WITH_KNOTS ( 'NONE', 3,
 ( #43818, #19461, #27678, #38189 ),
 .UNSPECIFIED., .F., .F.,
 ( 4, 4 ),
 ( 1.734723475976807094E-18, 2.647279941188286807E-05 ),
 .UNSPECIFIED. ) ;
#16206 = DIRECTION ( 'NONE',  ( 0.000000000000000000, -1.000000000000000000, 0.000000000000000000 ) ) ;
#16207 = SURFACE_STYLE_FILL_AREA ( #46700 ) ;
#16209 = ORIENTED_EDGE ( 'NONE', *, *, #39464, .T. ) ;
#16208 = EDGE_CURVE ( 'NONE', #14871, #1515, #43191, .T. ) ;
#16210 = PLANE ( 'NONE',  #34628 ) ;
#16211 = ADVANCED_FACE ( 'NONE', ( #46741, #27798 ), #47254, .T. ) ;
#16213 = ORIENTED_EDGE ( 'NONE', *, *, #34334, .F. ) ;
#16212 = VECTOR ( 'NONE', #20857, 1000.000000000000000 ) ;
#16214 = CARTESIAN_POINT ( 'NONE',  ( 183.0000000000000000, 6.000000000000060396, -350.0000000000001705 ) ) ;
#16215 = ORIENTED_EDGE ( 'NONE', *, *, #44055, .T. ) ;
#16216 = CARTESIAN_POINT ( 'NONE',  ( -4.945973446814903696, 2.143131898507912917E-16, 42.56828755692802702 ) ) ;
#16217 = LINE ( 'NONE', #8024, #8549 ) ;
#16218 = EDGE_CURVE ( 'NONE', #42092, #35238, #4447, .T. ) ;
#16219 = CARTESIAN_POINT ( 'NONE',  ( 341.6568542494923690, -165.0000000000001421, 339.9999999999999432 ) ) ;
#16220 = ORIENTED_EDGE ( 'NONE', *, *, #3976, .T. ) ;
#16221 = EDGE_CURVE ( 'NONE', #38683, #30983, #23945, .T. ) ;
#16222 = EDGE_CURVE ( 'NONE', #24145, #33295, #30505, .T. ) ;
#16223 = DIRECTION ( 'NONE',  ( 0.000000000000000000, 0.000000000000000000, -1.000000000000000000 ) ) ;
#16224 = FACE_OUTER_BOUND ( 'NONE', #28362, .T. ) ;
#16225 = ORIENTED_EDGE ( 'NONE', *, *, #15849, .T. ) ;
#16226 = CARTESIAN_POINT ( 'NONE',  ( 342.8284271247458150, -182.9999999999996589, 357.9999999999995453 ) ) ;
#16227 = CARTESIAN_POINT ( 'NONE',  ( 113.3040265531850537, 1.749999999999996891, 0.8182875569279768335 ) ) ;
#16228 =( BOUNDED_CURVE ( )  B_SPLINE_CURVE ( 3, ( #45541, #6573, #22223, #10421 ),
 .UNSPECIFIED., .F., .F. ) 
 B_SPLINE_CURVE_WITH_KNOTS ( ( 4, 4 ),
 ( 1.570796326794896558, 3.141592653589793116 ),
 .UNSPECIFIED. ) 
 CURVE ( )  GEOMETRIC_REPRESENTATION_ITEM ( )  RATIONAL_B_SPLINE_CURVE ( ( 1.000000000000000000, 0.8047378541243649375, 0.8047378541243649375, 1.000000000000000000 ) ) 
 REPRESENTATION_ITEM ( '' )  );
#16229 = CARTESIAN_POINT ( 'NONE',  ( 16.99749102614301677, -1.320765928724307425, 8.953103998512858652 ) ) ;
#16230 = FACE_OUTER_BOUND ( 'NONE', #6724, .T. ) ;
#16231 = CIRCLE ( 'NONE', #12131, 4.000000000000003553 ) ;
#16232 = EDGE_CURVE ( 'NONE', #42729, #9188, #38856, .T. ) ;
#16233 = ORIENTED_EDGE ( 'NONE', *, *, #50584, .F. ) ;
#16234 = ORIENTED_EDGE ( 'NONE', *, *, #21826, .T. ) ;
#16235 = DIRECTION ( 'NONE',  ( 0.000000000000000000, 0.000000000000000000, 1.000000000000000000 ) ) ;
#16236 = ORIENTED_EDGE ( 'NONE', *, *, #33386, .T. ) ;
#16237 = CARTESIAN_POINT ( 'NONE',  ( 0.000000000000000000, 0.000000000000000000, 0.000000000000000000 ) ) ;
#16238 = CARTESIAN_POINT ( 'NONE',  ( 15.00000000000000000, -46.51315789473684248, 6.315789473684215949 ) ) ;
#16239 = CARTESIAN_POINT ( 'NONE',  ( 5.551115123125782702E-14, -164.9999999999999432, 355.9999999999997726 ) ) ;
#16240 = ORIENTED_EDGE ( 'NONE', *, *, #44751, .T. ) ;
#16241 = LINE ( 'NONE', #39349, #47248 ) ;
#16242 = VERTEX_POINT ( 'NONE', #39360 ) ;
#16243 = LINE ( 'NONE', #15730, #37407 ) ;
#16244 = FACE_OUTER_BOUND ( 'NONE', #7088, .T. ) ;
#16245 = EDGE_LOOP ( 'NONE', ( #35119, #4262, #3166, #34236 ) ) ;
#16246 = AXIS2_PLACEMENT_3D ( 'NONE', #29320, #13404, #13160 ) ;
#16247 = VERTEX_POINT ( 'NONE', #19068 ) ;
#16248 = EDGE_LOOP ( 'NONE', ( #31136, #22010, #26108, #11855, #1393, #1167 ) ) ;
#16249 = CARTESIAN_POINT ( 'NONE',  ( -208.4459734468148611, 1.025126265847089657, 119.0682875569279560 ) ) ;
#16250 = CARTESIAN_POINT ( 'NONE',  ( 80.00000000000122213, 17.00000000000000000, 5.000000000000004441 ) ) ;
#16251 = LINE ( 'NONE', #5203, #331 ) ;
#16252 = EDGE_LOOP ( 'NONE', ( #40136, #31145, #35512, #3071, #2679 ) ) ;
#16253 = DIRECTION ( 'NONE',  ( 0.000000000000000000, -1.000000000000000000, 0.000000000000000000 ) ) ;
#16254 = ORIENTED_EDGE ( 'NONE', *, *, #6677, .T. ) ;
#16255 = ADVANCED_FACE ( 'NONE', ( #3678 ), #11642, .T. ) ;
#16256 = CARTESIAN_POINT ( 'NONE',  ( 0.3862712429686894766, -1.188820645368940276, 3.333333333333333481 ) ) ;
#16257 = EDGE_LOOP ( 'NONE', ( #29104, #1077, #37645, #9555, #14052, #48487 ) ) ;
#16258 = CARTESIAN_POINT ( 'NONE',  ( -47.72109971266203132, -1.750000000000010214, 81.84341382277507648 ) ) ;
#16259 = DIRECTION ( 'NONE',  ( 0.000000000000000000, 0.000000000000000000, 1.000000000000000000 ) ) ;
#16260 = DIRECTION ( 'NONE',  ( -0.000000000000000000, 0.000000000000000000, 1.000000000000000000 ) ) ;
#16261 = CARTESIAN_POINT ( 'NONE',  ( -48.44597344681496054, 1.025126265847089435, 82.56828755692798438 ) ) ;
#16262 = PLANE ( 'NONE',  #5287 ) ;
#16263 = CARTESIAN_POINT ( 'NONE',  ( 168.9999999999999716, -272.5000000000000000, -110.9999999999999005 ) ) ;
#16264 = VERTEX_POINT ( 'NONE', #15485 ) ;
#16265 = ORIENTED_EDGE ( 'NONE', *, *, #21826, .F. ) ;
#16266 = DIRECTION ( 'NONE',  ( 0.000000000000000000, -0.000000000000000000, -1.000000000000000000 ) ) ;
#16267 = B_SPLINE_SURFACE_WITH_KNOTS ( 'NONE', 3, 3, ( 
 ( #12947, #28604, #8858, #36080 ),
 ( #12704, #16563, #28365, #35578 ),
 ( #32222, #47315, #31729, #43995 ),
 ( #414, #27867, #20912, #36334 ) ),
 .UNSPECIFIED., .F., .F., .F.,
 ( 4, 4 ),
 ( 4, 4 ),
 ( 0.000000000000000000, 1.000000000000000000 ),
 ( 0.000000000000000000, 1.000000000000000000 ),
 .UNSPECIFIED. ) ;
#16268 = DIRECTION ( 'NONE',  ( -1.000000000000000000, 0.000000000000000000, 0.000000000000000000 ) ) ;
#16269 = CARTESIAN_POINT ( 'NONE',  ( 33.30402655318503946, -1.750000000000010214, -39.18171244307202983 ) ) ;
#16270 = EDGE_CURVE ( 'NONE', #5639, #40502, #8057, .T. ) ;
#16271 = FACE_OUTER_BOUND ( 'NONE', #22079, .T. ) ;
#16272 = EDGE_CURVE ( 'NONE', #28356, #28555, #9521, .T. ) ;
#16273 = DIRECTION ( 'NONE',  ( 0.000000000000000000, 0.000000000000000000, 1.000000000000000000 ) ) ;
#16274 = VERTEX_POINT ( 'NONE', #15245 ) ;
#16275 = CARTESIAN_POINT ( 'NONE',  ( -0.3440687301471724857, -1.609937937016752585, 9.936700280135882579 ) ) ;
#16276 = EDGE_CURVE ( 'NONE', #17553, #43423, #31914, .T. ) ;
#16277 = CARTESIAN_POINT ( 'NONE',  ( 193.3040265531851105, -1.750000000000009992, -159.1817124430720298 ) ) ;
#16278 = EDGE_CURVE ( 'NONE', #42411, #7277, #8192, .T. ) ;
#16279 = ADVANCED_FACE ( 'NONE', ( #26787 ), #50330, .F. ) ;
#16280 = EDGE_LOOP ( 'NONE', ( #9364, #28253 ) ) ;
#16281 =( BOUNDED_CURVE ( )  B_SPLINE_CURVE ( 3, ( #43222, #23731, #19617, #35298 ),
 .UNSPECIFIED., .F., .F. ) 
 B_SPLINE_CURVE_WITH_KNOTS ( ( 4, 4 ),
 ( 3.141592653589793116, 4.712388980384689674 ),
 .UNSPECIFIED. ) 
 CURVE ( )  GEOMETRIC_REPRESENTATION_ITEM ( )  RATIONAL_B_SPLINE_CURVE ( ( 1.000000000000000000, 0.8047378541243649375, 0.8047378541243649375, 1.000000000000000000 ) ) 
 REPRESENTATION_ITEM ( '' )  );
#16282 = CIRCLE ( 'NONE', #34300, 8.000000000000000000 ) ;
#16283 = CARTESIAN_POINT ( 'NONE',  ( 36.97942854200454832, -6.226705766838405154, 8.914903342594563185 ) ) ;
#16284 = CARTESIAN_POINT ( 'NONE',  ( 1.011271242968688311, -0.7347315653655855927, -3.333333333333333481 ) ) ;
#16285 = EDGE_CURVE ( 'NONE', #18435, #4602, #35018, .T. ) ;
#16286 = LINE ( 'NONE', #8088, #28296 ) ;
#16287 =( BOUNDED_CURVE ( )  B_SPLINE_CURVE ( 3, ( #10773, #42070, #15133, #3322 ),
 .UNSPECIFIED., .F., .F. ) 
 B_SPLINE_CURVE_WITH_KNOTS ( ( 4, 4 ),
 ( 4.712388980384693227, 6.283185307179586232 ),
 .UNSPECIFIED. ) 
 CURVE ( )  GEOMETRIC_REPRESENTATION_ITEM ( )  RATIONAL_B_SPLINE_CURVE ( ( 1.000000000000000000, 0.8047378541243658256, 0.8047378541243658256, 1.000000000000000000 ) ) 
 REPRESENTATION_ITEM ( '' )  );
#16288 = ORIENTED_EDGE ( 'NONE', *, *, #32398, .F. ) ;
#16289 = CLOSED_SHELL ( 'NONE', ( #41860, #6726, #17416, #32462, #27067, #4351, #46629, #49747, #3928, #2692, #12943, #38317, #33208, #44374, #43689, #20363, #21584, #47421, #48196, #14705, #40003, #15502, #48388, #12089, #22410, #44056, #27471, #2287, #11175, #20483, #26212, #38110, #30945, #23651, #19328, #18730, #22113, #49015, #46681, #1376, #47790, #16478 ) ) ;
#16290 = VERTEX_POINT ( 'NONE', #3936 ) ;
#16291 = DIRECTION ( 'NONE',  ( -1.000000000000000000, 0.000000000000000000, 0.000000000000000000 ) ) ;
#16292 = CARTESIAN_POINT ( 'NONE',  ( 155.0540265531850537, 2.143131898507880377E-16, 79.06828755692797017 ) ) ;
#16293 = VERTEX_POINT ( 'NONE', #35259 ) ;
#16294 = VERTEX_POINT ( 'NONE', #102 ) ;
#16295 = LINE ( 'NONE', #38211, #19573 ) ;
#16296 = CARTESIAN_POINT ( 'NONE',  ( -0.3910393408547386818, -3.877122853643371947, 9.741991644047244492 ) ) ;
#16297 = CARTESIAN_POINT ( 'NONE',  ( 25.61277432017878297, -22.36370378792834757, 7.906207997025717304 ) ) ;
#16298 = CARTESIAN_POINT ( 'NONE',  ( 152.2789002873379900, 1.750000000000010436, 79.79316129108087807 ) ) ;
#16299 = FACE_OUTER_BOUND ( 'NONE', #8317, .T. ) ;
#16300 = ORIENTED_EDGE ( 'NONE', *, *, #31288, .F. ) ;
#16301 = VERTEX_POINT ( 'NONE', #31670 ) ;
#16302 = ORIENTED_EDGE ( 'NONE', *, *, #46857, .F. ) ;
#16303 = FACE_OUTER_BOUND ( 'NONE', #17564, .T. ) ;
#16304 = VERTEX_POINT ( 'NONE', #15735 ) ;
#16305 = CARTESIAN_POINT ( 'NONE',  ( 169.0000000000000000, -9.999999999999953815, -95.00000000000014211 ) ) ;
#16306 = VERTEX_POINT ( 'NONE', #31406 ) ;
#16307 = VERTEX_POINT ( 'NONE', #47000 ) ;
#16308 = DIRECTION ( 'NONE',  ( 0.000000000000000000, 2.969158215481698263E-48, -1.000000000000000000 ) ) ;
#16309 = EDGE_CURVE ( 'NONE', #18068, #35388, #28046, .T. ) ;
#16310 = CARTESIAN_POINT ( 'NONE',  ( -8.831420117243776957, -14.12636088103186260, -3.546734833711462365 ) ) ;
#16311 = CYLINDRICAL_SURFACE ( 'NONE', #16680, 1.750000000000008438 ) ;
#16312 = ORIENTED_EDGE ( 'NONE', *, *, #6890, .T. ) ;
#16313 = VERTEX_POINT ( 'NONE', #9558 ) ;
#16314 = EDGE_CURVE ( 'NONE', #12712, #13146, #4940, .T. ) ;
#16315 = CARTESIAN_POINT ( 'NONE',  ( -14.49999999999999822, -46.01315789473684248, -5.916985404131817283 ) ) ;
#16316 =( NAMED_UNIT ( * ) PLANE_ANGLE_UNIT ( ) SI_UNIT ( $, .RADIAN. ) );
#16318 = ORIENTED_EDGE ( 'NONE', *, *, #24293, .T. ) ;
#16317 = AXIS2_PLACEMENT_3D ( 'NONE', #18379, #30450, #33804 ) ;
#16319 = DIRECTION ( 'NONE',  ( 0.000000000000000000, -0.000000000000000000, 1.000000000000000000 ) ) ;
#16320 = DIRECTION ( 'NONE',  ( 0.000000000000000000, -1.000000000000000000, 0.000000000000000000 ) ) ;
#16321 = AXIS2_PLACEMENT_3D ( 'NONE', #4661, #19791, #20050 ) ;
#16322 = FACE_OUTER_BOUND ( 'NONE', #44001, .T. ) ;
#16323 = VECTOR ( 'NONE', #43886, 1000.000000000000000 ) ;
#16324 = VERTEX_POINT ( 'NONE', #21097 ) ;
#16325 = VECTOR ( 'NONE', #15663, 1000.000000000000000 ) ;
#16326 = DIRECTION ( 'NONE',  ( -1.000000000000000000, 0.000000000000000000, 0.000000000000000000 ) ) ;
#16327 = CARTESIAN_POINT ( 'NONE',  ( -46.69597344681494633, 1.750000000000010658, -79.18171244307201562 ) ) ;
#16328 = CARTESIAN_POINT ( 'NONE',  ( -31.46770792452106846, 38.94077080897363885, 3.199614146704519602 ) ) ;
#16329 = AXIS2_PLACEMENT_3D ( 'NONE', #27737, #24900, #20783 ) ;
#16330 = CARTESIAN_POINT ( 'NONE',  ( -69.99999999999816680, 16.00000000000000000, 65.00000000000000000 ) ) ;
#16331 = CARTESIAN_POINT ( 'NONE',  ( -6.880036658038864772, 197.4999999999999432, -228.6347188485896140 ) ) ;
#16332 = CARTESIAN_POINT ( 'NONE',  ( -7.721099712662037540, -1.750000000000023537, -118.1565861772249519 ) ) ;
#16333 = DIRECTION ( 'NONE',  ( -0.000000000000000000, -0.000000000000000000, -1.000000000000000000 ) ) ;
#16334 = EDGE_LOOP ( 'NONE', ( #5092, #47746, #12199, #25013, #12817, #8279 ) ) ;
#16335 = CARTESIAN_POINT ( 'NONE',  ( 169.0000000000000000, 2.775557561562891351E-14, -95.00000000000014211 ) ) ;
#16336 = VERTEX_POINT ( 'NONE', #8558 ) ;
#16337 = CARTESIAN_POINT ( 'NONE',  ( -8.445973446814964092, -1.025126265847097429, -120.9317124430720440 ) ) ;
#16338 = EDGE_CURVE ( 'NONE', #25029, #3215, #12893, .T. ) ;
#16339 = DIRECTION ( 'NONE',  ( 0.000000000000000000, 0.000000000000000000, 1.000000000000000000 ) ) ;
#16340 = LINE ( 'NONE', #31759, #29103 ) ;
#16341 = ORIENTED_EDGE ( 'NONE', *, *, #46136, .T. ) ;
#16342 = CARTESIAN_POINT ( 'NONE',  ( -206.6959734468149463, 1.750000000000009992, 0.8182875569279768335 ) ) ;
#16343 = ORIENTED_EDGE ( 'NONE', *, *, #43469, .T. ) ;
#16344 = EDGE_LOOP ( 'NONE', ( #45709, #39718, #20107, #26584 ) ) ;
#16345 = CARTESIAN_POINT ( 'NONE',  ( 210.0000000000000568, 2.143131898507881116E-16, 39.06828755692797728 ) ) ;
#16346 = DIRECTION ( 'NONE',  ( 0.000000000000000000, 0.000000000000000000, 1.000000000000000000 ) ) ;
#16347 = VECTOR ( 'NONE', #39945, 1000.000000000000000 ) ;
#16348 = ORIENTED_EDGE ( 'NONE', *, *, #21401, .T. ) ;
#16349 = CARTESIAN_POINT ( 'NONE',  ( -164.9459734468149463, 1.025126265847089213, -160.9317124430720014 ) ) ;
#16350 = CARTESIAN_POINT ( 'NONE',  ( -126.6959734468149321, 1.749999999999996891, 160.8182875569279702 ) ) ;
#16351 = ORIENTED_EDGE ( 'NONE', *, *, #30737, .F. ) ;
#16352 = AXIS2_PLACEMENT_3D ( 'NONE', #15038, #46041, #45793 ) ;
#16353 = AXIS2_PLACEMENT_3D ( 'NONE', #35670, #4822, #47644 ) ;
#16354 = B_SPLINE_CURVE_WITH_KNOTS ( 'NONE', 3,
 ( #45191, #37556, #50284, #22376 ),
 .UNSPECIFIED., .F., .F.,
 ( 4, 4 ),
 ( 0.000000000000000000, 0.0004072981213154963339 ),
 .UNSPECIFIED. ) ;
#16355 = DIRECTION ( 'NONE',  ( -1.000000000000000000, -0.000000000000000000, -0.000000000000000000 ) ) ;
#16356 = ORIENTED_EDGE ( 'NONE', *, *, #25406, .F. ) ;
#16357 = DIRECTION ( 'NONE',  ( -1.000000000000000000, 0.000000000000000000, 0.000000000000000000 ) ) ;
#16358 = CARTESIAN_POINT ( 'NONE',  ( 343.9999999999999432, -185.0000000000001421, 360.0000000000001137 ) ) ;
#16359 = CARTESIAN_POINT ( 'NONE',  ( -10.30302290646040575, -13.08520913973572419, -9.683996418299976483 ) ) ;
#16360 = AXIS2_PLACEMENT_3D ( 'NONE', #8589, #5234, #12423 ) ;
#16361 = ORIENTED_EDGE ( 'NONE', *, *, #4829, .F. ) ;
#16362 = CARTESIAN_POINT ( 'NONE',  ( 25.04522487443081502, -22.77512090857307925, 8.356839323120299312 ) ) ;
#16363 = ORIENTED_EDGE ( 'NONE', *, *, #17913, .F. ) ;
#16364 = ORIENTED_EDGE ( 'NONE', *, *, #25203, .F. ) ;
#16365 = VERTEX_POINT ( 'NONE', #20596 ) ;
#16366 = CARTESIAN_POINT ( 'NONE',  ( -210.0000000000000568, 0.000000000000000000, -157.4317124430720298 ) ) ;
#16367 = CARTESIAN_POINT ( 'NONE',  ( -19.99999999999908695, 17.00000000000000000, -24.99999999999999289 ) ) ;
#16368 = ORIENTED_EDGE ( 'NONE', *, *, #42738, .F. ) ;
#16369 = EDGE_CURVE ( 'NONE', #32346, #44491, #23861, .T. ) ;
#16370 = CARTESIAN_POINT ( 'NONE',  ( 181.0000000000000000, -7.999999999999952038, 339.9999999999998295 ) ) ;
#16371 = DIRECTION ( 'NONE',  ( -1.000000000000000000, 0.000000000000000000, 0.000000000000000000 ) ) ;
#16372 = LINE ( 'NONE', #7671, #14909 ) ;
#16373 = CARTESIAN_POINT ( 'NONE',  ( 194.9999999999999432, 173.0000000000000000, 252.0000000000000000 ) ) ;
#16374 = DIRECTION ( 'NONE',  ( 0.000000000000000000, 0.000000000000000000, 1.000000000000000000 ) ) ;
#16375 = CARTESIAN_POINT ( 'NONE',  ( 6.174150299305392053, -33.14591993373988998, 8.807470649214879543 ) ) ;
#16376 = LINE ( 'NONE', #43571, #10160 ) ;
#16377 = CARTESIAN_POINT ( 'NONE',  ( 0.000000000000000000, 0.000000000000000000, 10.00000000000000000 ) ) ;
#16378 = CARTESIAN_POINT ( 'NONE',  ( 115.0540265531850395, 2.143131898507847836E-16, 2.568287556927950632 ) ) ;
#16379 = PLANE ( 'NONE',  #27297 ) ;
#16380 = CARTESIAN_POINT ( 'NONE',  ( 29.61572577327002520, 16.11461842845735859, 8.807470649214879543 ) ) ;
#16381 = VECTOR ( 'NONE', #9030, 1000.000000000000000 ) ;
#16382 = VECTOR ( 'NONE', #14622, 1000.000000000000000 ) ;
#16383 = PLANE ( 'NONE',  #31480 ) ;
#16384 = CARTESIAN_POINT ( 'NONE',  ( -0.8808108730257375729, -0.8497440890243460609, 9.966990753365125855 ) ) ;
#16385 = ORIENTED_EDGE ( 'NONE', *, *, #24404, .T. ) ;
#16386 = VECTOR ( 'NONE', #4932, 1000.000000000000000 ) ;
#16387 = DIRECTION ( 'NONE',  ( -1.000000000000000000, 0.000000000000000000, -1.612977847700450206E-50 ) ) ;
#16388 = LINE ( 'NONE', #12286, #44954 ) ;
#16389 = CARTESIAN_POINT ( 'NONE',  ( 135.0000000000019043, 17.00000000000000000, 65.00000000000000000 ) ) ;
#16390 = FACE_OUTER_BOUND ( 'NONE', #10603, .T. ) ;
#16391 = AXIS2_PLACEMENT_3D ( 'NONE', #16982, #43657, #39848 ) ;
#16392 = VERTEX_POINT ( 'NONE', #32660 ) ;
#16393 = PLANE ( 'NONE',  #39580 ) ;
#16394 = CARTESIAN_POINT ( 'NONE',  ( -1.468624871022813583, -0.3222420739259539979, 9.936141075690077429 ) ) ;
#16395 = VERTEX_POINT ( 'NONE', #36273 ) ;
#16396 = CARTESIAN_POINT ( 'NONE',  ( -21.61731705588949382, -25.43568671410586290, -9.367992836599951190 ) ) ;
#16397 = EDGE_CURVE ( 'NONE', #18511, #9824, #1111, .T. ) ;
#16398 = CARTESIAN_POINT ( 'NONE',  ( -1.258633725701695294, 0.04081300982073285399, 9.974012008644017158 ) ) ;
#16399 = CARTESIAN_POINT ( 'NONE',  ( -214.9999999999999432, 173.0000000000000000, 112.0000000000000000 ) ) ;
#16400 = ORIENTED_EDGE ( 'NONE', *, *, #19527, .T. ) ;
#16401 = CYLINDRICAL_SURFACE ( 'NONE', #20002, 1.750000000000015543 ) ;
#16402 = EDGE_LOOP ( 'NONE', ( #36508, #40788, #38687, #46151 ) ) ;
#16403 = ORIENTED_EDGE ( 'NONE', *, *, #39122, .T. ) ;
#16404 = EDGE_CURVE ( 'NONE', #42389, #39773, #24208, .T. ) ;
#16405 = EDGE_CURVE ( 'NONE', #42393, #15989, #32409, .T. ) ;
#16406 = ORIENTED_EDGE ( 'NONE', *, *, #34690, .F. ) ;
#16407 = DIRECTION ( 'NONE',  ( 0.000000000000000000, -1.000000000000000000, 0.000000000000000000 ) ) ;
#16408 = CARTESIAN_POINT ( 'NONE',  ( -205.6708471809678827, 1.750000000000009548, 39.79316129108089228 ) ) ;
#16409 = ORIENTED_EDGE ( 'NONE', *, *, #3526, .T. ) ;
#16410 = CARTESIAN_POINT ( 'NONE',  ( 135.0000000000009663, 16.00000000000000000, 0.000000000000000000 ) ) ;
#16411 = DIRECTION ( 'NONE',  ( 0.000000000000000000, 0.000000000000000000, 1.000000000000000000 ) ) ;
#16412 = EDGE_CURVE ( 'NONE', #12217, #15843, #3832, .T. ) ;
#16413 = DIRECTION ( 'NONE',  ( -1.000000000000000000, 0.000000000000000000, -0.000000000000000000 ) ) ;
#16414 = EDGE_CURVE ( 'NONE', #48161, #2701, #22196, .T. ) ;
#16415 = CARTESIAN_POINT ( 'NONE',  ( -166.6959734468149463, -1.750000000000009992, 160.8182875569279702 ) ) ;
#16416 = ORIENTED_EDGE ( 'NONE', *, *, #30737, .T. ) ;
#16417 = CARTESIAN_POINT ( 'NONE',  ( 224.9999999999999716, -164.9999999999999716, 62.29650858650038003 ) ) ;
#16418 = AXIS2_PLACEMENT_3D ( 'NONE', #43221, #20372, #11930 ) ;
#16419 = EDGE_CURVE ( 'NONE', #18366, #38893, #29167, .T. ) ;
#16420 =( BOUNDED_CURVE ( )  B_SPLINE_CURVE ( 3, ( #43524, #12976, #44269, #8394 ),
 .UNSPECIFIED., .F., .F. ) 
 B_SPLINE_CURVE_WITH_KNOTS ( ( 4, 4 ),
 ( 0.000000000000000000, 1.570796326794896558 ),
 .UNSPECIFIED. ) 
 CURVE ( )  GEOMETRIC_REPRESENTATION_ITEM ( )  RATIONAL_B_SPLINE_CURVE ( ( 1.000000000000000000, 0.8047378541243649375, 0.8047378541243649375, 1.000000000000000000 ) ) 
 REPRESENTATION_ITEM ( '' )  );
#16421 = VECTOR ( 'NONE', #2081, 1000.000000000000000 ) ;
#16422 = ORIENTED_EDGE ( 'NONE', *, *, #20259, .T. ) ;
#16423 = CARTESIAN_POINT ( 'NONE',  ( -114.9999999999991047, 17.00000000000000000, 0.000000000000000000 ) ) ;
#16424 = CARTESIAN_POINT ( 'NONE',  ( -119.9999999999997158, 17.00000000000000000, -84.99999999999998579 ) ) ;
#16425 = VERTEX_POINT ( 'NONE', #29059 ) ;
#16426 = CARTESIAN_POINT ( 'NONE',  ( 195.0540265531851105, 2.143131898507880377E-16, 82.56828755692798438 ) ) ;
#16427 = AXIS2_PLACEMENT_3D ( 'NONE', #24080, #8684, #9169 ) ;
#16428=STYLED_ITEM('',(#50747),#5102);
#16429 = CARTESIAN_POINT ( 'NONE',  ( 27.73884755486784570, -25.23502201956245017, 7.697694107796188234 ) ) ;
#16430 = VECTOR ( 'NONE', #16642, 1000.000000000000000 ) ;
#16431 = EDGE_CURVE ( 'NONE', #42864, #38152, #37002, .T. ) ;
#16432 = ORIENTED_EDGE ( 'NONE', *, *, #18044, .T. ) ;
#16433 = EDGE_CURVE ( 'NONE', #2629, #28405, #37039, .T. ) ;
#16434 = B_SPLINE_CURVE_WITH_KNOTS ( 'NONE', 3,
 ( #17699, #21805, #33368, #5135 ),
 .UNSPECIFIED., .F., .F.,
 ( 4, 4 ),
 ( 7.273049277091620462E-19, 0.0002708531562905798062 ),
 .UNSPECIFIED. ) ;
#16435 = CARTESIAN_POINT ( 'NONE',  ( 23.79193388295309219, 28.98609808355011452, -9.422646554964176246 ) ) ;
#16436 = DIRECTION ( 'NONE',  ( -8.673617379884028076E-17, 1.000000000000000000, -0.000000000000000000 ) ) ;
#16437 = PLANE ( 'NONE',  #34 ) ;
#16438 = LINE ( 'NONE', #47439, #7559 ) ;
#16439 = ADVANCED_FACE ( 'NONE', ( #860 ), #1864, .F. ) ;
#16440 = EDGE_CURVE ( 'NONE', #1237, #18422, #24667, .T. ) ;
#16441 = EDGE_LOOP ( 'NONE', ( #50230, #15579, #23509, #23143 ) ) ;
#16442 = DIRECTION ( 'NONE',  ( 0.000000000000000000, 0.000000000000000000, 1.000000000000000000 ) ) ;
#16443 = ADVANCED_FACE ( 'NONE', ( #36781 ), #1615, .T. ) ;
#16444 = CARTESIAN_POINT ( 'NONE',  ( -2.052560157877107994, 0.2040521727611285530, 9.891980816076527461 ) ) ;
#16445 = EDGE_CURVE ( 'NONE', #9595, #40596, #23612, .T. ) ;
#16446 =( BOUNDED_CURVE ( )  B_SPLINE_CURVE ( 3, ( #11993, #8147, #12980, #9144 ),
 .UNSPECIFIED., .F., .F. ) 
 B_SPLINE_CURVE_WITH_KNOTS ( ( 4, 4 ),
 ( 3.141592653589793116, 4.712388980384689674 ),
 .UNSPECIFIED. ) 
 CURVE ( )  GEOMETRIC_REPRESENTATION_ITEM ( )  RATIONAL_B_SPLINE_CURVE ( ( 1.000000000000000000, 0.8047378541243649375, 0.8047378541243649375, 1.000000000000000000 ) ) 
 REPRESENTATION_ITEM ( '' )  );
#16447 = CARTESIAN_POINT ( 'NONE',  ( -25.04522487443065160, 22.77512090857326754, 8.356839323120299312 ) ) ;
#16448 = VERTEX_POINT ( 'NONE', #32927 ) ;
#16449 = VERTEX_POINT ( 'NONE', #22547 ) ;
#16450 = PRODUCT_CONTEXT ( 'NONE', #32208, 'mechanical' ) ;
#16451 = CARTESIAN_POINT ( 'NONE',  ( 355.9999999999999432, -174.9999999999999432, 357.9999999999998295 ) ) ;
#16452 = FACE_OUTER_BOUND ( 'NONE', #18065, .T. ) ;
#16453 = FACE_OUTER_BOUND ( 'NONE', #14181, .T. ) ;
#16454 = CARTESIAN_POINT ( 'NONE',  ( -88.44597344681497475, 0.000000000000000000, -80.93171244307204404 ) ) ;
#16455 = CARTESIAN_POINT ( 'NONE',  ( 18.67411147745603373, 27.51799019669827473, -3.760136334089591248 ) ) ;
#16456 = ORIENTED_EDGE ( 'NONE', *, *, #14612, .F. ) ;
#16457 = DIRECTION ( 'NONE',  ( -0.000000000000000000, -0.000000000000000000, 1.000000000000000000 ) ) ;
#16458 = LINE ( 'NONE', #32110, #18747 ) ;
#16459 = DIRECTION ( 'NONE',  ( 0.000000000000000000, 0.000000000000000000, 1.000000000000000000 ) ) ;
#16460 = EDGE_CURVE ( 'NONE', #44725, #42432, #26908, .T. ) ;
#16461 = CARTESIAN_POINT ( 'NONE',  ( 153.3040265531850537, -1.750000000000010658, -79.18171244307201562 ) ) ;
#16462 = AXIS2_PLACEMENT_3D ( 'NONE', #24436, #20318, #12610 ) ;
#16463 = ORIENTED_EDGE ( 'NONE', *, *, #10197, .T. ) ;
#16464 = AXIS2_PLACEMENT_3D ( 'NONE', #24858, #24614, #27952 ) ;
#16465 = EDGE_CURVE ( 'NONE', #29723, #3587, #34417, .T. ) ;
#16466 = FACE_OUTER_BOUND ( 'NONE', #18904, .T. ) ;
#16467 = EDGE_LOOP ( 'NONE', ( #859, #6754, #8654, #50640 ) ) ;
#16468 = EDGE_CURVE ( 'NONE', #12217, #4426, #14821, .T. ) ;
#16469 = CARTESIAN_POINT ( 'NONE',  ( -0.3370904143228927730, -0.2449105217885335917, 10.00000000000000000 ) ) ;
#16470 = ORIENTED_EDGE ( 'NONE', *, *, #35031, .F. ) ;
#16471 = CARTESIAN_POINT ( 'NONE',  ( 135.0000000000000000, 16.00000000000000000, -90.00000000000000000 ) ) ;
#16472 = EDGE_CURVE ( 'NONE', #37466, #21335, #28859, .T. ) ;
#16473 = DIRECTION ( 'NONE',  ( 0.000000000000000000, 0.000000000000000000, 1.000000000000000000 ) ) ;
#16474 = CIRCLE ( 'NONE', #8313, 40.00000000000000000 ) ;
#16475 = CARTESIAN_POINT ( 'NONE',  ( -115.0000000000000284, 17.00000000000000000, -114.9999999999999858 ) ) ;
#16476 = DIRECTION ( 'NONE',  ( 0.000000000000000000, 0.000000000000000000, 1.000000000000000000 ) ) ;
#16477 = EDGE_LOOP ( 'NONE', ( #40022, #42785, #10284, #42971, #24817, #41257 ) ) ;
#16478 = ADVANCED_FACE ( 'NONE', ( #19195 ), #15111, .T. ) ;
#16479 = CARTESIAN_POINT ( 'NONE',  ( 85.00000000000056843, 16.00000000000000000, -54.99999999999999289 ) ) ;
#16480 = CYLINDRICAL_SURFACE ( 'NONE', #38596, 1.750000000000015543 ) ;
#16481 = ORIENTED_EDGE ( 'NONE', *, *, #11171, .F. ) ;
#16482 = CARTESIAN_POINT ( 'NONE',  ( 9.998889670239195837, 0.1490146381531976816, 9.282506307616472441 ) ) ;
#16483 = DIRECTION ( 'NONE',  ( -1.000000000000000000, 0.000000000000000000, 0.000000000000000000 ) ) ;
#16484 = FACE_OUTER_BOUND ( 'NONE', #16344, .T. ) ;
#16485 = LINE ( 'NONE', #839, #47917 ) ;
#16486 = EDGE_LOOP ( 'NONE', ( #36703, #25483, #19559, #3924, #32725, #40221 ) ) ;
#16487 = ORIENTED_EDGE ( 'NONE', *, *, #7473, .T. ) ;
#16488 = PLANE ( 'NONE',  #39876 ) ;
#16489 = EDGE_CURVE ( 'NONE', #16293, #26090, #34120, .T. ) ;
#16490 = VERTEX_POINT ( 'NONE', #46620 ) ;
#16491 = DIRECTION ( 'NONE',  ( 0.000000000000000000, 0.000000000000000000, -1.000000000000000000 ) ) ;
#16492 = LINE ( 'NONE', #12137, #34138 ) ;
#16493 = CYLINDRICAL_SURFACE ( 'NONE', #47668, 1.750000000000001554 ) ;
#16494 = EDGE_CURVE ( 'NONE', #48126, #33089, #34619, .T. ) ;
#16495 = ORIENTED_EDGE ( 'NONE', *, *, #36329, .T. ) ;
#16496 = CARTESIAN_POINT ( 'NONE',  ( -0.3862712429686809279, -1.188820645368943163, 10.00000000000000000 ) ) ;
#16497 = FACE_OUTER_BOUND ( 'NONE', #44490, .T. ) ;
#16498 = VECTOR ( 'NONE', #48006, 1000.000000000000000 ) ;
#16499 = CARTESIAN_POINT ( 'NONE',  ( -1.158497635116737312, 16.61944452314319420, -3.546734833711462365 ) ) ;
#16500 = ADVANCED_FACE ( 'NONE', ( #26400 ), #30771, .T. ) ;
#16502 = VERTEX_POINT ( 'NONE', #49707 ) ;
#16501 = EDGE_CURVE ( 'NONE', #2288, #26701, #19458, .T. ) ;
#16503 = VERTEX_POINT ( 'NONE', #50465 ) ;
#16504 = ORIENTED_EDGE ( 'NONE', *, *, #47028, .T. ) ;
#16505 = CARTESIAN_POINT ( 'NONE',  ( 0.9925179869589159098, 1.714505518806294835E-15, -14.00000000000000355 ) ) ;
#16506 = EDGE_CURVE ( 'NONE', #38568, #17971, #4592, .T. ) ;
#16507 = DIRECTION ( 'NONE',  ( -1.000000000000000000, 0.000000000000000000, 0.000000000000000000 ) ) ;
#16508 = VECTOR ( 'NONE', #38675, 1000.000000000000000 ) ;
#16509 = DIRECTION ( 'NONE',  ( -0.000000000000000000, -0.000000000000000000, 1.000000000000000000 ) ) ;
#16510 = EDGE_CURVE ( 'NONE', #2282, #36948, #12366, .T. ) ;
#16511 = ORIENTED_EDGE ( 'NONE', *, *, #31423, .F. ) ;
#16512 = DIRECTION ( 'NONE',  ( 1.000000000000000000, 1.156482317317870492E-16, -0.000000000000000000 ) ) ;
#16513 = CIRCLE ( 'NONE', #27167, 5.000000000000000000 ) ;
#16514 = EDGE_LOOP ( 'NONE', ( #9172, #47643, #11001, #11258 ) ) ;
#16515 = ADVANCED_FACE ( 'NONE', ( #38484 ), #49954, .F. ) ;
#16516 = CARTESIAN_POINT ( 'NONE',  ( -44.94597344681493922, -1.025126265847089435, 82.56828755692798438 ) ) ;
#16517 = VERTEX_POINT ( 'NONE', #3044 ) ;
#16518 = DIRECTION ( 'NONE',  ( -1.000000000000000000, 0.000000000000000000, -7.793956916774525800E-48 ) ) ;
#16519 = CARTESIAN_POINT ( 'NONE',  ( -120.0000000000000426, 17.00000000000000000, -90.00000000000000000 ) ) ;
#16520 = DIRECTION ( 'NONE',  ( -1.000000000000000000, 0.000000000000000000, 0.000000000000000000 ) ) ;
#16521 = DIRECTION ( 'NONE',  ( 1.000000000000000000, 0.000000000000000000, 0.000000000000000000 ) ) ;
#16522 = DIRECTION ( 'NONE',  ( -1.000000000000000000, 0.000000000000000000, 0.000000000000000000 ) ) ;
#16523 = ORIENTED_EDGE ( 'NONE', *, *, #35069, .F. ) ;
#16524 = FACE_OUTER_BOUND ( 'NONE', #35918, .T. ) ;
#16525 = CARTESIAN_POINT ( 'NONE',  ( -64.99999999999971578, 16.00000000000000000, -60.00000000000000000 ) ) ;
#16526 = CARTESIAN_POINT ( 'NONE',  ( 0.000000000000000000, 0.000000000000000000, 800.0000000000000000 ) ) ;
#16527 = SURFACE_STYLE_USAGE ( .BOTH. , #19855 ) ;
#16528 = EDGE_CURVE ( 'NONE', #19349, #36804, #42049, .T. ) ;
#16529 =( BOUNDED_CURVE ( )  B_SPLINE_CURVE ( 3, ( #4423, #12613, #1083, #15712 ),
 .UNSPECIFIED., .F., .F. ) 
 B_SPLINE_CURVE_WITH_KNOTS ( ( 4, 4 ),
 ( 0.000000000000000000, 1.570796326794896558 ),
 .UNSPECIFIED. ) 
 CURVE ( )  GEOMETRIC_REPRESENTATION_ITEM ( )  RATIONAL_B_SPLINE_CURVE ( ( 1.000000000000000000, 0.8047378541243649375, 0.8047378541243649375, 1.000000000000000000 ) ) 
 REPRESENTATION_ITEM ( '' )  );
#16530 = CARTESIAN_POINT ( 'NONE',  ( 164.9999999999999716, -164.9999999999999432, 355.9999999999998863 ) ) ;
#16531 = ORIENTED_EDGE ( 'NONE', *, *, #3975, .F. ) ;
#16532 = LINE ( 'NONE', #27831, #45819 ) ;
#16533 = VECTOR ( 'NONE', #20085, 1000.000000000000000 ) ;
#16534 = CARTESIAN_POINT ( 'NONE',  ( -166.6959734468149463, 1.750000000000010658, 120.8182875569279702 ) ) ;
#16535 = ORIENTED_EDGE ( 'NONE', *, *, #15000, .F. ) ;
#16536 = VECTOR ( 'NONE', #24420, 1000.000000000000000 ) ;
#16537 = PLANE ( 'NONE',  #11471 ) ;
#16538 = CARTESIAN_POINT ( 'NONE',  ( -0.4166666666666664631, 0.000000000000000000, -10.00000000000000000 ) ) ;
#16539 = CARTESIAN_POINT ( 'NONE',  ( -33.08717642956897009, -5.870837526464928402, -8.016098858316199838 ) ) ;
#16540 = FACE_OUTER_BOUND ( 'NONE', #21084, .T. ) ;
#16541 = ADVANCED_FACE ( 'NONE', ( #7426 ), #50198, .T. ) ;
#16542 = VERTEX_POINT ( 'NONE', #4073 ) ;
#16543 = VECTOR ( 'NONE', #38946, 1000.000000000000000 ) ;
#16544 = ORIENTED_EDGE ( 'NONE', *, *, #28537, .T. ) ;
#16545 = DIRECTION ( 'NONE',  ( -0.000000000000000000, -0.000000000000000000, -1.000000000000000000 ) ) ;
#16546 = CARTESIAN_POINT ( 'NONE',  ( -0.3862712429686729343, -1.188820645368946050, -10.00000000000000000 ) ) ;
#16547 = EDGE_LOOP ( 'NONE', ( #50554, #49191, #22850, #9000 ) ) ;
#16548 = ORIENTED_EDGE ( 'NONE', *, *, #22415, .F. ) ;
#16549 = DIRECTION ( 'NONE',  ( -0.000000000000000000, -1.000000000000000000, 0.000000000000000000 ) ) ;
#16550 = DIRECTION ( 'NONE',  ( -1.000000000000000000, 0.000000000000000000, 0.000000000000000000 ) ) ;
#16551 = CARTESIAN_POINT ( 'NONE',  ( 153.3040265531850537, 1.750000000000010658, 80.81828755692798438 ) ) ;
#16552 = DIRECTION ( 'NONE',  ( 1.000000000000000000, 0.000000000000000000, 0.000000000000000000 ) ) ;
#16553 = VERTEX_POINT ( 'NONE', #20228 ) ;
#16554 = ORIENTED_EDGE ( 'NONE', *, *, #20260, .F. ) ;
#16555 = ORIENTED_EDGE ( 'NONE', *, *, #15157, .T. ) ;
#16556 = DIRECTION ( 'NONE',  ( 1.000000000000000000, 0.000000000000000000, 0.000000000000000000 ) ) ;
#16557 = EDGE_CURVE ( 'NONE', #14709, #17646, #26905, .T. ) ;
#16558 = EDGE_CURVE ( 'NONE', #22009, #48914, #32166, .T. ) ;
#16559 = CARTESIAN_POINT ( 'NONE',  ( -28.55116071645519327, 41.05976639056880373, -2.408242355805840784 ) ) ;
#16560 = ORIENTED_EDGE ( 'NONE', *, *, #49972, .F. ) ;
#16561 = EDGE_LOOP ( 'NONE', ( #41975, #28467, #8053, #3513, #2263, #42035 ) ) ;
#16562 = CARTESIAN_POINT ( 'NONE',  ( 185.0000000000000000, 6.000000000000060396, -340.0000000000001137 ) ) ;
#16563 = CARTESIAN_POINT ( 'NONE',  ( -1.035950918207909632, -33.23661552194049307, -2.408242355805840784 ) ) ;
#16564 = DIRECTION ( 'NONE',  ( 0.000000000000000000, -1.000000000000000000, 0.000000000000000000 ) ) ;
#16565 = EDGE_CURVE ( 'NONE', #36281, #4790, #39372, .T. ) ;
#16566 = ORIENTED_EDGE ( 'NONE', *, *, #13918, .T. ) ;
#16567 = VERTEX_POINT ( 'NONE', #40236 ) ;
#16568 =( GEOMETRIC_REPRESENTATION_CONTEXT ( 3 ) GLOBAL_UNCERTAINTY_ASSIGNED_CONTEXT ( ( #31214 ) ) GLOBAL_UNIT_ASSIGNED_CONTEXT ( ( #46703, #35218, #11342 ) ) REPRESENTATION_CONTEXT ( 'NONE', 'WORKASPACE' ) );
#16569 = EDGE_CURVE ( 'NONE', #4709, #19922, #31287, .T. ) ;
#16570 = CARTESIAN_POINT ( 'NONE',  ( -9.643172164747307207, 0.000000000000000000, 0.000000000000000000 ) ) ;
#16571 = FILL_AREA_STYLE_COLOUR ( '', #41968 ) ;
#16572 = VERTEX_POINT ( 'NONE', #19966 ) ;
#16573 = ADVANCED_FACE ( 'NONE', ( #43310 ), #46874, .F. ) ;
#16574 = DIRECTION ( 'NONE',  ( -0.000000000000000000, -0.000000000000000000, -1.000000000000000000 ) ) ;
#16575 = CARTESIAN_POINT ( 'NONE',  ( -1.760168014277137649, -0.8403809255486067720, 9.896382706792437034 ) ) ;
#16576 = CYLINDRICAL_SURFACE ( 'NONE', #32304, 1.750000000000001554 ) ;
#16577 = EDGE_LOOP ( 'NONE', ( #2334, #30310, #13157, #10818 ) ) ;
#16578 = CARTESIAN_POINT ( 'NONE',  ( -208.4459734468149463, 0.000000000000000000, 79.06828755692797017 ) ) ;
#16579 = CARTESIAN_POINT ( 'NONE',  ( 35.05402655318504657, -1.025126265847089435, -117.4317124430720156 ) ) ;
#16580 = EDGE_CURVE ( 'NONE', #12217, #5524, #35655, .T. ) ;
#16581 = CARTESIAN_POINT ( 'NONE',  ( 154.3291528190321458, 1.750000000000010214, 121.8434138227750623 ) ) ;
#16582 = DIRECTION ( 'NONE',  ( -0.000000000000000000, -0.000000000000000000, -1.000000000000000000 ) ) ;
#16583 =( BOUNDED_CURVE ( )  B_SPLINE_CURVE ( 3, ( #7101, #14531, #11451, #26849 ),
 .UNSPECIFIED., .F., .F. ) 
 B_SPLINE_CURVE_WITH_KNOTS ( ( 4, 4 ),
 ( 4.712388980384689674, 6.283185307179586232 ),
 .UNSPECIFIED. ) 
 CURVE ( )  GEOMETRIC_REPRESENTATION_ITEM ( )  RATIONAL_B_SPLINE_CURVE ( ( 1.000000000000000000, 0.8047378541243649375, 0.8047378541243649375, 1.000000000000000000 ) ) 
 REPRESENTATION_ITEM ( '' )  );
#16584 = CYLINDRICAL_SURFACE ( 'NONE', #39286, 2.000000000000001776 ) ;
#16585 =( BOUNDED_CURVE ( )  B_SPLINE_CURVE ( 3, ( #13802, #49679, #33585, #29472 ),
 .UNSPECIFIED., .F., .F. ) 
 B_SPLINE_CURVE_WITH_KNOTS ( ( 4, 4 ),
 ( 3.141592653589793116, 4.712388980384689674 ),
 .UNSPECIFIED. ) 
 CURVE ( )  GEOMETRIC_REPRESENTATION_ITEM ( )  RATIONAL_B_SPLINE_CURVE ( ( 1.000000000000000000, 0.8047378541243649375, 0.8047378541243649375, 1.000000000000000000 ) ) 
 REPRESENTATION_ITEM ( '' )  );
#16586 = AXIS2_PLACEMENT_3D ( 'NONE', #40277, #5107, #20763 ) ;
#16587 = CARTESIAN_POINT ( 'NONE',  ( 210.0000000000000568, 2.143131898507880377E-16, 159.0682875569279702 ) ) ;
#16588 = CARTESIAN_POINT ( 'NONE',  ( 0.9983599181300923942, 1.124146016603553733, 9.953784399990620813 ) ) ;
#16589 = ORIENTED_EDGE ( 'NONE', *, *, #30071, .T. ) ;
#16590 = CARTESIAN_POINT ( 'NONE',  ( 21.23829395927641883, -7.388441598285492518, 229.0000000000000000 ) ) ;
#16591 = CARTESIAN_POINT ( 'NONE',  ( -36.28567981536816234, -9.465698090293395595, -9.422646554964174470 ) ) ;
#16592 = COLOUR_RGB ( '',0.7921568627450980005, 0.8196078431372548767, 0.9333333333333333481 ) ;
#16593 = ORIENTED_EDGE ( 'NONE', *, *, #16177, .F. ) ;
#16594 = DIRECTION ( 'NONE',  ( -1.000000000000000000, 0.000000000000000000, 0.000000000000000000 ) ) ;
#16595 = CARTESIAN_POINT ( 'NONE',  ( 341.9999999999999432, 182.1715728752539860, -357.1715728752541281 ) ) ;
#16596 = ORIENTED_EDGE ( 'NONE', *, *, #13563, .F. ) ;
#16597 = CARTESIAN_POINT ( 'NONE',  ( -166.6959734468149463, -1.750000000000010214, -39.18171244307202983 ) ) ;
#16598 = ORIENTED_EDGE ( 'NONE', *, *, #17379, .F. ) ;
#16599 = VERTEX_POINT ( 'NONE', #47376 ) ;
#16600 = CARTESIAN_POINT ( 'NONE',  ( -0.8051714816310078238, 0.2116216362810395268, 9.985686052694763504 ) ) ;
#16602 = ADVANCED_FACE ( 'NONE', ( #12271 ), #24091, .T. ) ;
#16601 = VECTOR ( 'NONE', #13848, 1000.000000000000000 ) ;
#16603 = CARTESIAN_POINT ( 'NONE',  ( 358.0000000000001137, 182.1715728752538439, 357.1715728752535597 ) ) ;
#16604 = VERTEX_POINT ( 'NONE', #4581 ) ;
#16605 = VECTOR ( 'NONE', #49018, 1000.000000000000000 ) ;
#16606 = CARTESIAN_POINT ( 'NONE',  ( -5.000000000000000000, -165.1999999999999602, -340.2000000000001592 ) ) ;
#16607 = ORIENTED_EDGE ( 'NONE', *, *, #10830, .F. ) ;
#16608 = CARTESIAN_POINT ( 'NONE',  ( -19.99999999999846523, 17.00000000000000000, 35.00000000000000000 ) ) ;
#16609 = ORIENTED_EDGE ( 'NONE', *, *, #17142, .T. ) ;
#16610 = LINE ( 'NONE', #35631, #31553 ) ;
#16611 = CYLINDRICAL_SURFACE ( 'NONE', #47921, 1.749999999999973799 ) ;
#16612 = CYLINDRICAL_SURFACE ( 'NONE', #28389, 1.750000000000001554 ) ;
#16613 = ORIENTED_EDGE ( 'NONE', *, *, #13057, .T. ) ;
#16614 = DIRECTION ( 'NONE',  ( -1.000000000000000000, 0.000000000000000000, 0.000000000000000000 ) ) ;
#16615 = CARTESIAN_POINT ( 'NONE',  ( 73.30402655318508209, 1.750000000000010658, 120.8182875569279702 ) ) ;
#16616 = EDGE_LOOP ( 'NONE', ( #38962, #42538, #28807, #30902, #38013, #32335 ) ) ;
#16617 = ORIENTED_EDGE ( 'NONE', *, *, #39122, .F. ) ;
#16618 = EDGE_LOOP ( 'NONE', ( #45471, #50451, #40645, #19544, #50228 ) ) ;
#16619 = VECTOR ( 'NONE', #41849, 1000.000000000000000 ) ;
#16620 = CARTESIAN_POINT ( 'NONE',  ( 343.9999999999999432, -183.0000000000002558, -358.0000000000003411 ) ) ;
#16621 = EDGE_LOOP ( 'NONE', ( #42569, #1900, #20383, #27038 ) ) ;
#16622 = CARTESIAN_POINT ( 'NONE',  ( 210.0000000000000568, 2.143131898507880377E-16, -160.9317124430720298 ) ) ;
#16623 = CARTESIAN_POINT ( 'NONE',  ( -46.69597344681494633, 0.000000000000000000, 165.0000000000000000 ) ) ;
#16624 = ADVANCED_FACE ( 'NONE', ( #39235 ), #729, .T. ) ;
#16625 = DIRECTION ( 'NONE',  ( 0.000000000000000000, 0.000000000000000000, 1.000000000000000000 ) ) ;
#16626 = CARTESIAN_POINT ( 'NONE',  ( 210.0000000000000568, 2.143131898507880377E-16, -160.9317124430720298 ) ) ;
#16627 = CARTESIAN_POINT ( 'NONE',  ( 168.9999999999999716, -77.49999999999995737, -115.0000000000001563 ) ) ;
#16628 = CARTESIAN_POINT ( 'NONE',  ( -204.9459734468149463, 2.143131898507880377E-16, -120.9317124430720156 ) ) ;
#16629 = EDGE_CURVE ( 'NONE', #33089, #18511, #12518, .T. ) ;
#16630 = VECTOR ( 'NONE', #19202, 1000.000000000000000 ) ;
#16631 = CARTESIAN_POINT ( 'NONE',  ( -210.0000000000000568, 0.000000000000000000, 40.81828755692798438 ) ) ;
#16632 = CARTESIAN_POINT ( 'NONE',  ( 181.0000000000000284, -174.9999999999999716, -99.00000000000014211 ) ) ;
#16633 = CARTESIAN_POINT ( 'NONE',  ( 195.0540265531851105, 2.143131898507880377E-16, 165.0000000000000000 ) ) ;
#16634 = B_SPLINE_CURVE_WITH_KNOTS ( 'NONE', 3,
 ( #13224, #8385, #36616, #44259 ),
 .UNSPECIFIED., .F., .F.,
 ( 4, 4 ),
 ( 0.000000000000000000, 0.002368422649471283847 ),
 .UNSPECIFIED. ) ;
#16635 = MECHANICAL_DESIGN_GEOMETRIC_PRESENTATION_REPRESENTATION (  '', ( #24846 ), #1078 ) ;
#16636 = DIRECTION ( 'NONE',  ( 0.000000000000000000, 0.000000000000000000, 1.000000000000000000 ) ) ;
#16637 = DIRECTION ( 'NONE',  ( 0.000000000000000000, 0.000000000000000000, -1.000000000000000000 ) ) ;
#16638 = VERTEX_POINT ( 'NONE', #43817 ) ;
#16639 = PLANE ( 'NONE',  #13841 ) ;
#16640 = CARTESIAN_POINT ( 'NONE',  ( 0.3862712429686894766, -1.188820645368940276, 10.00000000000000000 ) ) ;
#16641 = LINE ( 'NONE', #28700, #40612 ) ;
#16642 = DIRECTION ( 'NONE',  ( 1.000000000000000000, 0.000000000000000000, 0.000000000000000000 ) ) ;
#16643 = ORIENTED_EDGE ( 'NONE', *, *, #22751, .T. ) ;
#16644 = CARTESIAN_POINT ( 'NONE',  ( 10.50000000000000178, -46.01315789473684248, 5.916985404131813731 ) ) ;
#16645 = CARTESIAN_POINT ( 'NONE',  ( -1.468535767197700181, -0.3224370614408916813, 9.944962737616616977 ) ) ;
#16646 = ORIENTED_EDGE ( 'NONE', *, *, #13491, .F. ) ;
#16647 = LINE ( 'NONE', #40763, #36964 ) ;
#16648 = CARTESIAN_POINT ( 'NONE',  ( 20.72411365307712572, -36.23316402738139885, -8.080361901872242569 ) ) ;
#16649 = DIRECTION ( 'NONE',  ( 0.000000000000000000, 0.000000000000000000, -1.000000000000000000 ) ) ;
#16650 = ORIENTED_EDGE ( 'NONE', *, *, #42738, .T. ) ;
#16651 = LINE ( 'NONE', #4844, #15909 ) ;
#16652 = VERTEX_POINT ( 'NONE', #24349 ) ;
#16653 = ORIENTED_EDGE ( 'NONE', *, *, #12283, .F. ) ;
#16654 = EDGE_CURVE ( 'NONE', #26020, #16170, #20013, .T. ) ;
#16655 = VERTEX_POINT ( 'NONE', #27423 ) ;
#16656 = CARTESIAN_POINT ( 'NONE',  ( 181.0000000000000000, -272.4999999999999432, -343.9999999999999432 ) ) ;
#16657 = CARTESIAN_POINT ( 'NONE',  ( 344.0000000000000000, -165.0000000000001137, -340.0000000000002842 ) ) ;
#16658 = VECTOR ( 'NONE', #33274, 1000.000000000000000 ) ;
#16659 = ORIENTED_EDGE ( 'NONE', *, *, #21594, .T. ) ;
#16660 = DIRECTION ( 'NONE',  ( 1.000000000000000000, 0.000000000000000000, 0.000000000000000000 ) ) ;
#16661 = LINE ( 'NONE', #20761, #49590 ) ;
#16662 = VECTOR ( 'NONE', #45808, 1000.000000000000000 ) ;
#16663 = LINE ( 'NONE', #24875, #22441 ) ;
#16664 = DIRECTION ( 'NONE',  ( -0.000000000000000000, 0.000000000000000000, -1.000000000000000000 ) ) ;
#16665 = ORIENTED_EDGE ( 'NONE', *, *, #13922, .T. ) ;
#16666 = CARTESIAN_POINT ( 'NONE',  ( 15.00000000000000000, 12.98684210526315930, -19.37312575500899570 ) ) ;
#16667 = EDGE_LOOP ( 'NONE', ( #20306, #3659, #48679, #35182 ) ) ;
#16668 =( GEOMETRIC_REPRESENTATION_CONTEXT ( 3 ) GLOBAL_UNCERTAINTY_ASSIGNED_CONTEXT ( ( #38918 ) ) GLOBAL_UNIT_ASSIGNED_CONTEXT ( ( #13172, #35536, #47775 ) ) REPRESENTATION_CONTEXT ( 'NONE', 'WORKASPACE' ) );
#16669 = CARTESIAN_POINT ( 'NONE',  ( 152.2789002873379900, 1.750000000000009548, 81.84341382277507648 ) ) ;
#16670 = CARTESIAN_POINT ( 'NONE',  ( 35.00000000000186162, 17.00000000000000000, 65.00000000000000000 ) ) ;
#16671 = ORIENTED_EDGE ( 'NONE', *, *, #33326, .T. ) ;
#16672 = CARTESIAN_POINT ( 'NONE',  ( -119.9999999999990905, 17.00000000000000000, 0.000000000000000000 ) ) ;
#16673 = DIRECTION ( 'NONE',  ( -0.000000000000000000, -1.000000000000000000, -0.000000000000000000 ) ) ;
#16674 = B_SPLINE_SURFACE_WITH_KNOTS ( 'NONE', 3, 3, ( 
 ( #487, #46111, #34618, #11006 ),
 ( #23572, #7425, #39234, #233 ),
 ( #31540, #42306, #30770, #50197 ),
 ( #38483, #18942, #4072, #46381 ) ),
 .UNSPECIFIED., .F., .F., .F.,
 ( 4, 4 ),
 ( 4, 4 ),
 ( 0.000000000000000000, 1.000000000000000000 ),
 ( 0.000000000000000000, 1.000000000000000000 ),
 .UNSPECIFIED. ) ;
#16675 = ORIENTED_EDGE ( 'NONE', *, *, #41057, .F. ) ;
#16676 = CARTESIAN_POINT ( 'NONE',  ( -16.16402646813540755, 4.033894069732547827, -3.546734833711462365 ) ) ;
#16677 = CARTESIAN_POINT ( 'NONE',  ( -208.4459734468149463, 0.000000000000000000, -37.43171244307205825 ) ) ;
#16678 = LINE ( 'NONE', #48187, #40169 ) ;
#16679 = CARTESIAN_POINT ( 'NONE',  ( -2.188678504086925880, 0.3267089737526900350, 9.881002359080270026 ) ) ;
#16680 = AXIS2_PLACEMENT_3D ( 'NONE', #1179, #32224, #29122 ) ;
#16681 = ORIENTED_EDGE ( 'NONE', *, *, #32215, .T. ) ;
#16682 = CARTESIAN_POINT ( 'NONE',  ( -128.4459734468149179, 0.000000000000000000, 165.0000000000000000 ) ) ;
#16684 = EDGE_CURVE ( 'NONE', #37965, #1676, #132, .T. ) ;
#16683 = CARTESIAN_POINT ( 'NONE',  ( 45.21167770612395742, 22.65616271077811206, 7.906207997025717304 ) ) ;
#16685 = FACE_OUTER_BOUND ( 'NONE', #41798, .T. ) ;
#16686 = EDGE_LOOP ( 'NONE', ( #35789, #20077, #45977, #39642 ) ) ;
#16687 = ORIENTED_EDGE ( 'NONE', *, *, #27535, .T. ) ;
#16688 = CARTESIAN_POINT ( 'NONE',  ( 30.00000000000217781, 16.00000000000000000, 95.00000000000000000 ) ) ;
#16689 = CARTESIAN_POINT ( 'NONE',  ( 191.5540265531850537, -1.025126265847089657, -120.9317124430720440 ) ) ;
#16690 = CARTESIAN_POINT ( 'NONE',  ( -165.3973046169136012, 54.43801056904003133, -17.65743994998275213 ) ) ;
#16691 = VECTOR ( 'NONE', #40087, 1000.000000000000114 ) ;
#16692 = CARTESIAN_POINT ( 'NONE',  ( 356.0000000000000568, 183.0000000000000853, 357.9999999999998295 ) ) ;
#16693 = CARTESIAN_POINT ( 'NONE',  ( -48.44597344681495343, 0.000000000000000000, 42.56828755692798438 ) ) ;
#16694 = ORIENTED_EDGE ( 'NONE', *, *, #35811, .T. ) ;
#16695 = LINE ( 'NONE', #48212, #7529 ) ;
#16696 = AXIS2_PLACEMENT_3D ( 'NONE', #27687, #35407, #24102 ) ;
#16697 = EDGE_CURVE ( 'NONE', #1440, #7897, #8025, .T. ) ;
#16698 = CARTESIAN_POINT ( 'NONE',  ( -168.4459734468149463, 0.000000000000000000, -77.43171244307204404 ) ) ;
#16699 = CARTESIAN_POINT ( 'NONE',  ( 339.9999999999999432, -169.0000000000001137, -349.9999999999998863 ) ) ;
#16700 = VECTOR ( 'NONE', #6617, 1000.000000000000000 ) ;
#16701 = DIRECTION ( 'NONE',  ( 0.000000000000000000, 0.000000000000000000, 1.000000000000000000 ) ) ;
#16702 = ADVANCED_FACE ( 'NONE', ( #5066 ), #9430, .T. ) ;
#16703 = CIRCLE ( 'NONE', #45349, 4.000000000000003553 ) ;
#16704 = VERTEX_POINT ( 'NONE', #32550 ) ;
#16705 = DIRECTION ( 'NONE',  ( 0.000000000000000000, 0.000000000000000000, 1.000000000000000000 ) ) ;
#16706 = ORIENTED_EDGE ( 'NONE', *, *, #12832, .T. ) ;
#16707 = CYLINDRICAL_SURFACE ( 'NONE', #18780, 4.000000000000003553 ) ;
#16708 = ORIENTED_EDGE ( 'NONE', *, *, #19513, .T. ) ;
#16709 = DIRECTION ( 'NONE',  ( 1.000000000000000000, -0.000000000000000000, -0.000000000000000000 ) ) ;
#16710 = CARTESIAN_POINT ( 'NONE',  ( 168.9999999999999716, -95.49999999999998579, -340.0000000000001137 ) ) ;
#16711 = EDGE_CURVE ( 'NONE', #12321, #36910, #43531, .T. ) ;
#16712 = DIRECTION ( 'NONE',  ( 0.000000000000000000, 0.000000000000000000, 1.000000000000000000 ) ) ;
#16713 = CARTESIAN_POINT ( 'NONE',  ( 1.347864860736642800, 0.3239901621378048491, 9.960033073700785167 ) ) ;
#16714 = EDGE_CURVE ( 'NONE', #14077, #4803, #35790, .T. ) ;
#16715 = VERTEX_POINT ( 'NONE', #9683 ) ;
#16716 =( BOUNDED_CURVE ( )  B_SPLINE_CURVE ( 3, ( #38889, #15277, #22453, #42201 ),
 .UNSPECIFIED., .F., .F. ) 
 B_SPLINE_CURVE_WITH_KNOTS ( ( 4, 4 ),
 ( 3.141592653589793116, 4.712388980384689674 ),
 .UNSPECIFIED. ) 
 CURVE ( )  GEOMETRIC_REPRESENTATION_ITEM ( )  RATIONAL_B_SPLINE_CURVE ( ( 1.000000000000000000, 0.8047378541243649375, 0.8047378541243649375, 1.000000000000000000 ) ) 
 REPRESENTATION_ITEM ( '' )  );
#16717 = EDGE_CURVE ( 'NONE', #35676, #35737, #48131, .T. ) ;
#16718 = EDGE_CURVE ( 'NONE', #20200, #11140, #30644, .T. ) ;
#16719 = VECTOR ( 'NONE', #36409, 1000.000000000000000 ) ;
#16720 = CARTESIAN_POINT ( 'NONE',  ( 84.99999999999997158, 16.00000000000000000, -114.9999999999999858 ) ) ;
#16721 = ORIENTED_EDGE ( 'NONE', *, *, #43830, .T. ) ;
#16722 = CARTESIAN_POINT ( 'NONE',  ( 164.9999999999999716, -93.50000000000005684, -340.0000000000001137 ) ) ;
#16723 = CYLINDRICAL_SURFACE ( 'NONE', #37997, 1.750000000000001554 ) ;
#16724 = FACE_OUTER_BOUND ( 'NONE', #40262, .T. ) ;
#16725 = CARTESIAN_POINT ( 'NONE',  ( 10.50000000000000178, -46.01315789473684248, -5.916985404131818171 ) ) ;
#16726 =( BOUNDED_CURVE ( )  B_SPLINE_CURVE ( 3, ( #2790, #37471, #34118, #26659 ),
 .UNSPECIFIED., .F., .F. ) 
 B_SPLINE_CURVE_WITH_KNOTS ( ( 4, 4 ),
 ( 4.712388980384689674, 6.283185307179586232 ),
 .UNSPECIFIED. ) 
 CURVE ( )  GEOMETRIC_REPRESENTATION_ITEM ( )  RATIONAL_B_SPLINE_CURVE ( ( 1.000000000000000000, 0.8047378541243649375, 0.8047378541243649375, 1.000000000000000000 ) ) 
 REPRESENTATION_ITEM ( '' )  );
#16727 = ORIENTED_EDGE ( 'NONE', *, *, #50642, .F. ) ;
#16728 = ORIENTED_EDGE ( 'NONE', *, *, #22387, .T. ) ;
#16729 = PLANE ( 'NONE',  #49653 ) ;
#16730 = VERTEX_POINT ( 'NONE', #40492 ) ;
#16731 = PLANE ( 'NONE',  #41345 ) ;
#16732 = CARTESIAN_POINT ( 'NONE',  ( -14.99999999999812594, 16.00000000000000000, 65.00000000000000000 ) ) ;
#16733 = VECTOR ( 'NONE', #29793, 1000.000000000000000 ) ;
#16734 = AXIS2_PLACEMENT_3D ( 'NONE', #46851, #27398, #32018 ) ;
#16735 = DIRECTION ( 'NONE',  ( -1.000000000000000000, 0.000000000000000000, -0.000000000000000000 ) ) ;
#16736 = ORIENTED_EDGE ( 'NONE', *, *, #26240, .F. ) ;
#16737 = CARTESIAN_POINT ( 'NONE',  ( -128.4459734468149179, 0.000000000000000000, -120.9317124430720156 ) ) ;
#16738 = AXIS2_PLACEMENT_3D ( 'NONE', #18473, #10281, #30044 ) ;
#16739 =( BOUNDED_CURVE ( )  B_SPLINE_CURVE ( 3, ( #10434, #10934, #14789, #22237 ),
 .UNSPECIFIED., .F., .F. ) 
 B_SPLINE_CURVE_WITH_KNOTS ( ( 4, 4 ),
 ( 0.000000000000000000, 1.570796326794896558 ),
 .UNSPECIFIED. ) 
 CURVE ( )  GEOMETRIC_REPRESENTATION_ITEM ( )  RATIONAL_B_SPLINE_CURVE ( ( 1.000000000000000000, 0.8047378541243649375, 0.8047378541243649375, 1.000000000000000000 ) ) 
 REPRESENTATION_ITEM ( '' )  );
#16740 = CARTESIAN_POINT ( 'NONE',  ( -7.822422304254325276, 2.683863964738837371, 226.0000000000000000 ) ) ;
#16741 = EDGE_CURVE ( 'NONE', #18435, #23225, #25338, .T. ) ;
#16742 = AXIS2_PLACEMENT_3D ( 'NONE', #24648, #9733, #20533 ) ;
#16743 = CARTESIAN_POINT ( 'NONE',  ( 5.990542248694086247, 8.025558178072422777, 3.215106848023467911 ) ) ;
#16744 = DIRECTION ( 'NONE',  ( -0.000000000000000000, -1.000000000000000000, -0.000000000000000000 ) ) ;
#16745 = CARTESIAN_POINT ( 'NONE',  ( 164.9999999999999716, 17.00000000000000000, -1.387778780781445676E-14 ) ) ;
#16746 = CARTESIAN_POINT ( 'NONE',  ( 151.5540265531850537, 0.000000000000000000, -80.93171244307201562 ) ) ;
#16747 = EDGE_CURVE ( 'NONE', #46762, #2324, #40988, .T. ) ;
#16748 = EDGE_LOOP ( 'NONE', ( #11420, #49444, #16385, #1870, #48145, #39735 ) ) ;
#16749 = EDGE_CURVE ( 'NONE', #40480, #36547, #13020, .T. ) ;
#16750 = ORIENTED_EDGE ( 'NONE', *, *, #18236, .F. ) ;
#16751 = VERTEX_POINT ( 'NONE', #17633 ) ;
#16752 = DIRECTION ( 'NONE',  ( 0.7233555441435720601, -0.6904757466825006684, 0.000000000000000000 ) ) ;
#16754 = ADVANCED_FACE ( 'NONE', ( #28931, #36408 ), #9932, .T. ) ;
#16753 = LINE ( 'NONE', #49261, #18518 ) ;
#16755 = CARTESIAN_POINT ( 'NONE',  ( 3.808200756227633654, 0.8261963378076531139, 9.741991644047248045 ) ) ;
#16756 = ORIENTED_EDGE ( 'NONE', *, *, #33201, .F. ) ;
#16757 = EDGE_CURVE ( 'NONE', #25407, #28907, #13772, .T. ) ;
#16758 = PLANE ( 'NONE',  #34039 ) ;
#16759 = VERTEX_POINT ( 'NONE', #6085 ) ;
#16760 =( NAMED_UNIT ( * ) PLANE_ANGLE_UNIT ( ) SI_UNIT ( $, .RADIAN. ) );
#16761 = CARTESIAN_POINT ( 'NONE',  ( -124.9459734468149463, 2.143131898507847836E-16, 39.06828755692798438 ) ) ;
#16762 = CARTESIAN_POINT ( 'NONE',  ( -69.99999999999879208, 16.00000000000000000, 5.000000000000004441 ) ) ;
#16763 = DIRECTION ( 'NONE',  ( 1.000000000000000000, -4.758098676964956461E-16, -8.975803739141899931E-48 ) ) ;
#16764 = VECTOR ( 'NONE', #31357, 1000.000000000000000 ) ;
#16765 = CARTESIAN_POINT ( 'NONE',  ( -6.880036658038864772, 197.4999999999999432, -228.6347188485896140 ) ) ;
#16766 = DIRECTION ( 'NONE',  ( 0.000000000000000000, -0.000000000000000000, 1.000000000000000000 ) ) ;
#16767 = VECTOR ( 'NONE', #23320, 1000.000000000000000 ) ;
#16768 = CARTESIAN_POINT ( 'NONE',  ( -0.6440276692615888310, -16.64212148744554298, -9.683996418299976483 ) ) ;
#16769 = ORIENTED_EDGE ( 'NONE', *, *, #13758, .F. ) ;
#16770 = LINE ( 'NONE', #43699, #44378 ) ;
#16771 = DIRECTION ( 'NONE',  ( -1.000000000000000000, 0.000000000000000000, 0.000000000000000000 ) ) ;
#16772 = CARTESIAN_POINT ( 'NONE',  ( -126.6959734468149321, 0.000000000000000000, 165.0000000000000000 ) ) ;
#16773 = CARTESIAN_POINT ( 'NONE',  ( 16.52264463346132572, -2.779753662172757878, 9.403735324607438884 ) ) ;
#16774 = ORIENTED_EDGE ( 'NONE', *, *, #29206, .T. ) ;
#16775 = AXIS2_PLACEMENT_3D ( 'NONE', #23033, #2530, #22531 ) ;
#16776 = EDGE_CURVE ( 'NONE', #3156, #5291, #48885, .T. ) ;
#16777 = PLANE ( 'NONE',  #13040 ) ;
#16778 = ORIENTED_EDGE ( 'NONE', *, *, #31586, .T. ) ;
#16779 = LINE ( 'NONE', #24486, #9026 ) ;
#16780 = EDGE_CURVE ( 'NONE', #38434, #18354, #5329, .T. ) ;
#16781 = DIRECTION ( 'NONE',  ( -0.000000000000000000, -1.000000000000000000, -0.000000000000000000 ) ) ;
#16782 = ADVANCED_FACE ( 'NONE', ( #13269, #20989 ), #1740, .T. ) ;
#16783 = AXIS2_PLACEMENT_3D ( 'NONE', #20919, #31978, #40428 ) ;
#16784 = EDGE_LOOP ( 'NONE', ( #10613, #18108, #34214, #21013 ) ) ;
#16785 = EDGE_CURVE ( 'NONE', #20063, #41652, #12825, .T. ) ;
#16786 = EDGE_CURVE ( 'NONE', #12663, #44970, #37424, .T. ) ;
#16787 = CARTESIAN_POINT ( 'NONE',  ( 4.763548243873389154, -16.57409059453848599, 8.727788335465566760 ) ) ;
#16788 = DIRECTION ( 'NONE',  ( -1.000000000000000000, 0.000000000000000000, -0.000000000000000000 ) ) ;
#16789 = CARTESIAN_POINT ( 'NONE',  ( -16.73672383626882976, -2.341008440547994063, -9.008049429158100807 ) ) ;
#16790 = EDGE_CURVE ( 'NONE', #11473, #25384, #18057, .T. ) ;
#16791 = DIRECTION ( 'NONE',  ( -0.000000000000000000, 1.000000000000000000, 0.000000000000000000 ) ) ;
#16792 = EDGE_CURVE ( 'NONE', #32969, #27078, #7104, .T. ) ;
#16793 = EDGE_LOOP ( 'NONE', ( #9001, #40340, #29278, #30387, #41038 ) ) ;
#16794 = ORIENTED_EDGE ( 'NONE', *, *, #15761, .T. ) ;
#16795 = DIRECTION ( 'NONE',  ( -0.000000000000000000, -0.000000000000000000, -1.000000000000000000 ) ) ;
#16796 = CARTESIAN_POINT ( 'NONE',  ( 15.98719783915691650, -4.501063718205879916, 3.266473740018926541 ) ) ;
#16797 = AXIS2_PLACEMENT_3D ( 'NONE', #2514, #45825, #21502 ) ;
#16798 = VERTEX_POINT ( 'NONE', #15320 ) ;
#16799 = ORIENTED_EDGE ( 'NONE', *, *, #37565, .F. ) ;
#16800 = CARTESIAN_POINT ( 'NONE',  ( 339.9999999999998863, 181.0000000000000284, -360.0000000000003411 ) ) ;
#16801 = FACE_OUTER_BOUND ( 'NONE', #22829, .T. ) ;
#16802 = LINE ( 'NONE', #31959, #21004 ) ;
#16803 = LINE ( 'NONE', #23999, #22325 ) ;
#16804 = ORIENTED_EDGE ( 'NONE', *, *, #514, .F. ) ;
#16805 = CIRCLE ( 'NONE', #43007, 4.000000000000003553 ) ;
#16806 = EDGE_LOOP ( 'NONE', ( #31195, #30333, #32811, #24778 ) ) ;
#16807 = ORIENTED_EDGE ( 'NONE', *, *, #28702, .T. ) ;
#16808 = CARTESIAN_POINT ( 'NONE',  ( -46.69597344681494633, -1.750000000000009992, -159.1817124430720298 ) ) ;
#16809 = AXIS2_PLACEMENT_3D ( 'NONE', #28190, #4815, #43820 ) ;
#16810 = EDGE_CURVE ( 'NONE', #23987, #750, #11213, .T. ) ;
#16811 = ADVANCED_FACE ( 'NONE', ( #14794 ), #30973, .F. ) ;
#16812 = DIRECTION ( 'NONE',  ( 1.000000000000000000, -4.996003610813203446E-16, 1.033975765691284226E-24 ) ) ;
#16813 = AXIS2_PLACEMENT_3D ( 'NONE', #6327, #2468, #2714 ) ;
#16814 = VERTEX_POINT ( 'NONE', #2489 ) ;
#16815 = ORIENTED_EDGE ( 'NONE', *, *, #16506, .F. ) ;
#16816 = DIRECTION ( 'NONE',  ( 1.000000000000000000, -0.000000000000000000, -0.000000000000000000 ) ) ;
#16817 = DIRECTION ( 'NONE',  ( -0.000000000000000000, -1.000000000000000000, -0.000000000000000000 ) ) ;
#16818 = AXIS2_PLACEMENT_3D ( 'NONE', #47199, #23893, #42366 ) ;
#16819 = ORIENTED_EDGE ( 'NONE', *, *, #42456, .F. ) ;
#16820 = ORIENTED_EDGE ( 'NONE', *, *, #3004, .T. ) ;
#16821 = VECTOR ( 'NONE', #39120, 1000.000000000000000 ) ;
#16822 = DIRECTION ( 'NONE',  ( 8.673617379884028076E-17, -1.000000000000000000, 0.000000000000000000 ) ) ;
#16823 = SURFACE_STYLE_FILL_AREA ( #1183 ) ;
#16824 = EDGE_LOOP ( 'NONE', ( #25824, #34587, #22810, #34359, #50045, #16650 ) ) ;
#16825 = CARTESIAN_POINT ( 'NONE',  ( 15.00000000000000000, 12.98684210526315930, 0.000000000000000000 ) ) ;
#16826 = CARTESIAN_POINT ( 'NONE',  ( 130.0000000000018474, 17.00000000000000000, 65.00000000000000000 ) ) ;
#16827 = CARTESIAN_POINT ( 'NONE',  ( -210.0000000000000568, 2.143131898507876926E-16, 79.06828755692797017 ) ) ;
#16828 =( BOUNDED_CURVE ( )  B_SPLINE_CURVE ( 3, ( #20993, #36412, #9939, #48889 ),
 .UNSPECIFIED., .F., .F. ) 
 B_SPLINE_CURVE_WITH_KNOTS ( ( 4, 4 ),
 ( 4.712388980384689674, 6.283185307179586232 ),
 .UNSPECIFIED. ) 
 CURVE ( )  GEOMETRIC_REPRESENTATION_ITEM ( )  RATIONAL_B_SPLINE_CURVE ( ( 1.000000000000000000, 0.8047378541243649375, 0.8047378541243649375, 1.000000000000000000 ) ) 
 REPRESENTATION_ITEM ( '' )  );
#16829 = FACE_OUTER_BOUND ( 'NONE', #48406, .T. ) ;
#16830 = VERTEX_POINT ( 'NONE', #10439 ) ;
#16831 = EDGE_CURVE ( 'NONE', #30864, #48470, #18131, .T. ) ;
#16832 = DIRECTION ( 'NONE',  ( -0.000000000000000000, -0.000000000000000000, -1.000000000000000000 ) ) ;
#16833 = DIRECTION ( 'NONE',  ( 0.000000000000000000, -2.537652627714643577E-15, -1.000000000000000000 ) ) ;
#16834 = CARTESIAN_POINT ( 'NONE',  ( 35.00000000000186162, 16.00000000000000000, 65.00000000000000000 ) ) ;
#16835 = VECTOR ( 'NONE', #42699, 1000.000000000000000 ) ;
#16836 = EDGE_CURVE ( 'NONE', #11587, #22898, #34829, .T. ) ;
#16837 = VECTOR ( 'NONE', #3569, 1000.000000000000000 ) ;
#16838 = CARTESIAN_POINT ( 'NONE',  ( 195.0540265531851105, 2.143131898507880377E-16, -0.9317124430720247208 ) ) ;
#16839 = CARTESIAN_POINT ( 'NONE',  ( 153.3040265531850537, 0.000000000000000000, -165.0000000000000000 ) ) ;
#16840 = VECTOR ( 'NONE', #2370, 1000.000000000000000 ) ;
#16841 = DIRECTION ( 'NONE',  ( 0.000000000000000000, 0.000000000000000000, 1.000000000000000000 ) ) ;
#16842 = CARTESIAN_POINT ( 'NONE',  ( 48.98697415750968531, 11.03699497439252752, -8.016098858316199838 ) ) ;
#16843 = VERTEX_POINT ( 'NONE', #42486 ) ;
#16844 = FACE_BOUND ( 'NONE', #12581, .T. ) ;
#16845 = CIRCLE ( 'NONE', #3723, 4.000000000000003553 ) ;
#16846 = EDGE_CURVE ( 'NONE', #5769, #42417, #9819, .T. ) ;
#16847 = ADVANCED_FACE ( 'NONE', ( #37916 ), #2732, .T. ) ;
#16848 = DIRECTION ( 'NONE',  ( 0.000000000000000000, -1.000000000000000000, 0.000000000000000000 ) ) ;
#16849 = AXIS2_PLACEMENT_3D ( 'NONE', #22187, #37854, #42424 ) ;
#16850 = VECTOR ( 'NONE', #21981, 1000.000000000000000 ) ;
#16851 = VERTEX_POINT ( 'NONE', #22987 ) ;
#16852 = CARTESIAN_POINT ( 'NONE',  ( -19.61585174098950546, 31.96834229807166139, -9.011255500499645521 ) ) ;
#16853 = CARTESIAN_POINT ( 'NONE',  ( -204.9459734468148895, -1.025126265847089435, -77.43171244307200141 ) ) ;
#16854 = EDGE_CURVE ( 'NONE', #48255, #15017, #49832, .T. ) ;
#16855 = EDGE_LOOP ( 'NONE', ( #35960, #42593, #36468, #19861 ) ) ;
#16856 = FACE_OUTER_BOUND ( 'NONE', #48166, .T. ) ;
#16857 = ORIENTED_EDGE ( 'NONE', *, *, #9079, .F. ) ;
#16858 = VERTEX_POINT ( 'NONE', #7358 ) ;
#16859 = CIRCLE ( 'NONE', #23416, 10.00000000000000000 ) ;
#16860 = CARTESIAN_POINT ( 'NONE',  ( 1.250000000000000222, 0.000000000000000000, -10.00000000000000000 ) ) ;
#16861 = EDGE_CURVE ( 'NONE', #8725, #22263, #15067, .T. ) ;
#16862 = DIRECTION ( 'NONE',  ( -0.000000000000000000, 1.604368532695312981E-16, 1.000000000000000000 ) ) ;
#16863 = EDGE_CURVE ( 'NONE', #27926, #41541, #6847, .T. ) ;
#16864 = ORIENTED_EDGE ( 'NONE', *, *, #15636, .T. ) ;
#16865 = PLANE ( 'NONE',  #38562 ) ;
#16866 = VERTEX_POINT ( 'NONE', #50408 ) ;
#16867 = ORIENTED_EDGE ( 'NONE', *, *, #2395, .T. ) ;
#16868 = EDGE_CURVE ( 'NONE', #23377, #43115, #14280, .T. ) ;
#16869 = CARTESIAN_POINT ( 'NONE',  ( -8.445973446814976526, 0.000000000000000000, 2.568287556928034121 ) ) ;
#16870 = EDGE_LOOP ( 'NONE', ( #39604, #46153, #22023 ) ) ;
#16871 = CARTESIAN_POINT ( 'NONE',  ( 344.0000000000000000, 175.0000000000000284, -94.00000000000019895 ) ) ;
#16872 = CARTESIAN_POINT ( 'NONE',  ( 349.9999999999999432, -180.9999999999999716, 341.9999999999997726 ) ) ;
#16873 = DIRECTION ( 'NONE',  ( -0.000000000000000000, -0.000000000000000000, -1.000000000000000000 ) ) ;
#16874 = AXIS2_PLACEMENT_3D ( 'NONE', #2956, #49855, #39153 ) ;
#16875 = ORIENTED_EDGE ( 'NONE', *, *, #31809, .T. ) ;
#16876 = CARTESIAN_POINT ( 'NONE',  ( -4.999999999999997335, 214.9999999999999716, -234.7500000000000000 ) ) ;
#16877 = CARTESIAN_POINT ( 'NONE',  ( 13.35436367797824353, 31.26996044524050333, 7.906207997025717304 ) ) ;
#16878 = ORIENTED_EDGE ( 'NONE', *, *, #3110, .T. ) ;
#16879 = VECTOR ( 'NONE', #36327, 1000.000000000000000 ) ;
#16880 = VERTEX_POINT ( 'NONE', #38168 ) ;
#16881 = ORIENTED_EDGE ( 'NONE', *, *, #18086, .F. ) ;
#16882 = PLANE ( 'NONE',  #16427 ) ;
#16883 = VECTOR ( 'NONE', #14359, 1000.000000000000000 ) ;
#16884 = DIRECTION ( 'NONE',  ( 1.000000000000000000, 0.000000000000000000, 2.958228394578794270E-31 ) ) ;
#16885 = ORIENTED_EDGE ( 'NONE', *, *, #40592, .T. ) ;
#16886 = CARTESIAN_POINT ( 'NONE',  ( -17.51065725283106289, 28.41934970907792746, -9.367992836599954742 ) ) ;
#16887 = CARTESIAN_POINT ( 'NONE',  ( -84.94597344681493212, -1.025126265847089435, 162.5682875569279133 ) ) ;
#16888 = CARTESIAN_POINT ( 'NONE',  ( -6.695973446814940111, -1.750000000000023315, 0.8182875569279768335 ) ) ;
#16889 =( BOUNDED_CURVE ( )  B_SPLINE_CURVE ( 3, ( #48494, #37772, #5684, #45158 ),
 .UNSPECIFIED., .F., .F. ) 
 B_SPLINE_CURVE_WITH_KNOTS ( ( 4, 4 ),
 ( 3.141592653589793116, 4.712388980384689674 ),
 .UNSPECIFIED. ) 
 CURVE ( )  GEOMETRIC_REPRESENTATION_ITEM ( )  RATIONAL_B_SPLINE_CURVE ( ( 1.000000000000000000, 0.8047378541243649375, 0.8047378541243649375, 1.000000000000000000 ) ) 
 REPRESENTATION_ITEM ( '' )  );
#16890 = CARTESIAN_POINT ( 'NONE',  ( 185.0000000000000000, -5.999999999999950262, 339.9999999999998295 ) ) ;
#16891 = CARTESIAN_POINT ( 'NONE',  ( 350.0000000000000000, -184.9999999999999716, -344.0000000000001705 ) ) ;
#16892 = AXIS2_PLACEMENT_3D ( 'NONE', #23887, #4389, #47447 ) ;
#16893 = CARTESIAN_POINT ( 'NONE',  ( -19.99999999999815969, 17.00000000000000000, 65.00000000000000000 ) ) ;
#16894 = CARTESIAN_POINT ( 'NONE',  ( -164.9999999999997442, 16.00000000000000000, -84.99999999999998579 ) ) ;
#16895 = DIRECTION ( 'NONE',  ( 1.000000000000000000, 0.000000000000000000, 0.000000000000000000 ) ) ;
#16896 =( BOUNDED_CURVE ( )  B_SPLINE_CURVE ( 3, ( #48828, #21415, #41680, #37600 ),
 .UNSPECIFIED., .F., .F. ) 
 B_SPLINE_CURVE_WITH_KNOTS ( ( 4, 4 ),
 ( 4.712388980384689674, 6.283185307179586232 ),
 .UNSPECIFIED. ) 
 CURVE ( )  GEOMETRIC_REPRESENTATION_ITEM ( )  RATIONAL_B_SPLINE_CURVE ( ( 1.000000000000000000, 0.8047378541243649375, 0.8047378541243649375, 1.000000000000000000 ) ) 
 REPRESENTATION_ITEM ( '' )  );
#16897 = FACE_OUTER_BOUND ( 'NONE', #26111, .T. ) ;
#16898 = CARTESIAN_POINT ( 'NONE',  ( -124.9459734468149321, -1.025126265847081886, 119.0682875569279702 ) ) ;
#16899 = EDGE_CURVE ( 'NONE', #11165, #23532, #37612, .T. ) ;
#16900 = VECTOR ( 'NONE', #6560, 1000.000000000000000 ) ;
#16901 = CARTESIAN_POINT ( 'NONE',  ( 154.1026953830863420, 103.9380105690400597, -17.65743994998277699 ) ) ;
#16902 = UNCERTAINTY_MEASURE_WITH_UNIT (LENGTH_MEASURE( 1.000000000000000082E-05 ), #2311, 'distance_accuracy_value', 'NONE');
#16903 = FACE_OUTER_BOUND ( 'NONE', #29136, .T. ) ;
#16904 = ORIENTED_EDGE ( 'NONE', *, *, #2313, .F. ) ;
#16905 = DIRECTION ( 'NONE',  ( -0.000000000000000000, -0.000000000000000000, -1.000000000000000000 ) ) ;
#16906 = DIRECTION ( 'NONE',  ( -1.000000000000000000, 0.000000000000000000, 0.000000000000000000 ) ) ;
#16907 = DIRECTION ( 'NONE',  ( -1.000000000000000000, -0.000000000000000000, -0.000000000000000000 ) ) ;
#16908 = LINE ( 'NONE', #13785, #16430 ) ;
#16909 = VERTEX_POINT ( 'NONE', #27113 ) ;
#16910 = VECTOR ( 'NONE', #49306, 1000.000000000000000 ) ;
#16911 = PLANE ( 'NONE',  #33863 ) ;
#16912 = ADVANCED_FACE ( 'NONE', ( #14534 ), #46053, .F. ) ;
#16913 = EDGE_CURVE ( 'NONE', #865, #16365, #19660, .T. ) ;
#16914 = VECTOR ( 'NONE', #25641, 1000.000000000000000 ) ;
#16915 = LINE ( 'NONE', #48155, #25394 ) ;
#16916 = AXIS2_PLACEMENT_3D ( 'NONE', #1299, #16947, #33300 ) ;
#16917 = EDGE_LOOP ( 'NONE', ( #50591, #21579, #50526, #33889 ) ) ;
#16918 = CARTESIAN_POINT ( 'NONE',  ( 0.3862712429686727678, 1.188820645368945605, -3.333333333333333481 ) ) ;
#16919 = CARTESIAN_POINT ( 'NONE',  ( 75.05402655318509630, -1.025126265847089657, -120.9317124430720440 ) ) ;
#16920 = CARTESIAN_POINT ( 'NONE',  ( -44.94597344681493922, 2.143131898507880377E-16, -0.9317124430720247208 ) ) ;
#16921 = ORIENTED_EDGE ( 'NONE', *, *, #16506, .T. ) ;
#16922 = LINE ( 'NONE', #31572, #8551 ) ;
#16923 = ORIENTED_EDGE ( 'NONE', *, *, #49599, .T. ) ;
#16924 = ORIENTED_EDGE ( 'NONE', *, *, #44782, .F. ) ;
#16925 = EDGE_CURVE ( 'NONE', #26133, #11313, #38929, .T. ) ;
#16926 = ADVANCED_FACE ( 'NONE', ( #23244 ), #8628, .F. ) ;
#16927 = AXIS2_PLACEMENT_3D ( 'NONE', #34285, #33529, #41212 ) ;
#16928 = ORIENTED_EDGE ( 'NONE', *, *, #10726, .F. ) ;
#16929 = CARTESIAN_POINT ( 'NONE',  ( 130.0000000000018474, 16.00000000000000000, 90.00000000000000000 ) ) ;
#16930 = DIRECTION ( 'NONE',  ( 0.000000000000000000, 0.000000000000000000, 1.000000000000000000 ) ) ;
#16931 = ORIENTED_EDGE ( 'NONE', *, *, #5778, .F. ) ;
#16932 = DIRECTION ( 'NONE',  ( -1.000000000000000000, 4.996003610813203446E-16, -1.033975765691284226E-24 ) ) ;
#16933 = CARTESIAN_POINT ( 'NONE',  ( 185.0000000000000000, -272.4999999999999432, -343.9999999999987494 ) ) ;
#16934 = EDGE_CURVE ( 'NONE', #50336, #46082, #4518, .T. ) ;
#16935 = DIRECTION ( 'NONE',  ( -0.8637789008984334549, 0.000000000000000000, 0.5038710255240862468 ) ) ;
#16936 = CARTESIAN_POINT ( 'NONE',  ( -26.20171990995768141, 42.76673505352046334, -8.466730184410787174 ) ) ;
#16937 = ORIENTED_EDGE ( 'NONE', *, *, #11810, .T. ) ;
#16938 = VECTOR ( 'NONE', #18489, 1000.000000000000000 ) ;
#16939 = LINE ( 'NONE', #9221, #209 ) ;
#16940 = ORIENTED_EDGE ( 'NONE', *, *, #28017, .T. ) ;
#16941 = LINE ( 'NONE', #17180, #2965 ) ;
#16942 = CARTESIAN_POINT ( 'NONE',  ( 350.0000000000000000, -166.9999999999999432, -344.0000000000001705 ) ) ;
#16943 = VERTEX_POINT ( 'NONE', #20161 ) ;
#16944 = ORIENTED_EDGE ( 'NONE', *, *, #40314, .T. ) ;
#16945 = CARTESIAN_POINT ( 'NONE',  ( -210.0000000000000568, 2.143131898507890731E-16, 159.0682875569279702 ) ) ;
#16946 = VERTEX_POINT ( 'NONE', #43256 ) ;
#16947 = DIRECTION ( 'NONE',  ( -1.000000000000000000, -0.000000000000000000, -0.000000000000000000 ) ) ;
#16948 = DIRECTION ( 'NONE',  ( 0.000000000000000000, -1.000000000000000000, 0.000000000000000000 ) ) ;
#16949 = FACE_OUTER_BOUND ( 'NONE', #17375, .T. ) ;
#16950 = CARTESIAN_POINT ( 'NONE',  ( 18.67411147745603373, 27.51799019669827473, -3.760136334089591248 ) ) ;
#16951 = VECTOR ( 'NONE', #48249, 1000.000000000000000 ) ;
#16952 = VERTEX_POINT ( 'NONE', #15812 ) ;
#16953 = CARTESIAN_POINT ( 'NONE',  ( -4.945973446814917018, 1.025126265847097207, -40.93171244307204404 ) ) ;
#16954 = CARTESIAN_POINT ( 'NONE',  ( 1.011271242968688311, -0.7347315653655855927, 10.00000000000000000 ) ) ;
#16955 = CARTESIAN_POINT ( 'NONE',  ( -5.000000000000000000, 184.8000000000000114, -359.8000000000002387 ) ) ;
#16956 = ORIENTED_EDGE ( 'NONE', *, *, #18888, .F. ) ;
#16957 = EDGE_CURVE ( 'NONE', #36969, #12576, #3178, .T. ) ;
#16958 = VERTEX_POINT ( 'NONE', #19408 ) ;
#16959 = CARTESIAN_POINT ( 'NONE',  ( 232.4999999999999716, -169.9999999999999716, 474.9999999999998863 ) ) ;
#16960 = CARTESIAN_POINT ( 'NONE',  ( 113.3040265531850537, -1.749999999999997335, -79.18171244307201562 ) ) ;
#16961 = CYLINDRICAL_SURFACE ( 'NONE', #7634, 1.750000000000015543 ) ;
#16962 = VERTEX_POINT ( 'NONE', #35089 ) ;
#16963 = DIRECTION ( 'NONE',  ( -1.000000000000000000, -0.000000000000000000, -0.000000000000000000 ) ) ;
#16964 = DIRECTION ( 'NONE',  ( 0.5038710255240862468, 0.000000000000000000, 0.8637789008984334549 ) ) ;
#16965 = CARTESIAN_POINT ( 'NONE',  ( -164.9459734468149463, 2.143131898507880377E-16, 165.0000000000000000 ) ) ;
#16966 = CARTESIAN_POINT ( 'NONE',  ( 33.57695195286775913, 16.69845195084893064, 8.914903342594561408 ) ) ;
#16967 = AXIS2_PLACEMENT_3D ( 'NONE', #31010, #34595, #19700 ) ;
#16968 = ORIENTED_EDGE ( 'NONE', *, *, #39308, .T. ) ;
#16969 = CARTESIAN_POINT ( 'NONE',  ( 3.345242017215822372, -2.159124855890657724, -4.878909776184769953E-16 ) ) ;
#16970 = ORIENTED_EDGE ( 'NONE', *, *, #9327, .T. ) ;
#16971 = LINE ( 'NONE', #25171, #42555 ) ;
#16972 = ORIENTED_EDGE ( 'NONE', *, *, #25879, .F. ) ;
#16973 = DIRECTION ( 'NONE',  ( -1.000000000000000000, -0.000000000000000000, -0.000000000000000000 ) ) ;
#16974 = CARTESIAN_POINT ( 'NONE',  ( 185.0000000000000284, -174.9999999999999716, -111.0000000000001563 ) ) ;
#16975 = VERTEX_POINT ( 'NONE', #24285 ) ;
#16976 = B_SPLINE_CURVE_WITH_KNOTS ( 'NONE', 3,
 ( #4314, #44532, #20712, #40217 ),
 .UNSPECIFIED., .F., .F.,
 ( 4, 4 ),
 ( 1.093600287244414006E-15, 0.0004154657329504815111 ),
 .UNSPECIFIED. ) ;
#16978 = CARTESIAN_POINT ( 'NONE',  ( 20.21530556545302559, -31.58467066308217497, -9.422646554964174470 ) ) ;
#16977 = B_SPLINE_CURVE_WITH_KNOTS ( 'NONE', 3,
 ( #7260, #37331, #18542, #17799 ),
 .UNSPECIFIED., .F., .F.,
 ( 4, 4 ),
 ( 0.0009679537044783742029, 0.001281751046851238845 ),
 .UNSPECIFIED. ) ;
#16979 = VERTEX_POINT ( 'NONE', #50659 ) ;
#16980 = PLANE ( 'NONE',  #25393 ) ;
#16981 = DIRECTION ( 'NONE',  ( 1.000000000000000000, 0.000000000000000000, -0.000000000000000000 ) ) ;
#16982 = CARTESIAN_POINT ( 'NONE',  ( -49.75871208702130133, 40.58472229863599523, 5.000000000000000000 ) ) ;
#16983 = DIRECTION ( 'NONE',  ( 0.000000000000000000, 0.000000000000000000, 1.000000000000000000 ) ) ;
#16984 = EDGE_CURVE ( 'NONE', #42393, #639, #671, .T. ) ;
#16985 = DIRECTION ( 'NONE',  ( -0.000000000000000000, -0.000000000000000000, -1.000000000000000000 ) ) ;
#16986 = ORIENTED_EDGE ( 'NONE', *, *, #9534, .T. ) ;
#16987 = ORIENTED_EDGE ( 'NONE', *, *, #23993, .F. ) ;
#16988 = CARTESIAN_POINT ( 'NONE',  ( -119.9999999999978400, 16.00000000000000000, 95.00000000000000000 ) ) ;
#16989 = ORIENTED_EDGE ( 'NONE', *, *, #44950, .F. ) ;
#16990 = DIRECTION ( 'NONE',  ( 0.000000000000000000, 0.000000000000000000, -1.000000000000000000 ) ) ;
#16991 = CARTESIAN_POINT ( 'NONE',  ( 192.2789002873380184, 1.750000000000009326, -158.1565861772249377 ) ) ;
#16992 = DIRECTION ( 'NONE',  ( 0.000000000000000000, 1.000000000000000000, 3.186989995019654210E-49 ) ) ;
#16993 = ORIENTED_EDGE ( 'NONE', *, *, #13920, .T. ) ;
#16994 = CARTESIAN_POINT ( 'NONE',  ( -0.1475726264153620626, -1.496347932843211215, 9.927319414211227766 ) ) ;
#16995 = PLANE ( 'NONE',  #7065 ) ;
#16996 = CARTESIAN_POINT ( 'NONE',  ( 1.256322718835040542, 0.9753643601100148164, 9.933322880749875239 ) ) ;
#16997 = CARTESIAN_POINT ( 'NONE',  ( -32.36066692128246558, 7.813306791043033606, 3.199614146704519602 ) ) ;
#16998 = CARTESIAN_POINT ( 'NONE',  ( 0.000000000000000000, 33.89193117067290473, 910.0000000000000000 ) ) ;
#16999 = DIRECTION ( 'NONE',  ( -1.000000000000000000, 0.000000000000000000, 0.000000000000000000 ) ) ;
#17000 = ORIENTED_EDGE ( 'NONE', *, *, #596, .F. ) ;
#17001 = ORIENTED_EDGE ( 'NONE', *, *, #7113, .T. ) ;
#17002 = ORIENTED_EDGE ( 'NONE', *, *, #7054, .T. ) ;
#17003 = DIRECTION ( 'NONE',  ( -0.000000000000000000, 1.000000000000000000, 1.224646799147353207E-16 ) ) ;
#17004 = DIRECTION ( 'NONE',  ( 0.000000000000000000, -1.000000000000000000, 2.537652627714643577E-15 ) ) ;
#17005 = DIRECTION ( 'NONE',  ( -1.000000000000000000, 0.000000000000000000, 0.000000000000000000 ) ) ;
#17006 = DIRECTION ( 'NONE',  ( 1.000000000000000000, 0.000000000000000000, 0.000000000000000000 ) ) ;
#17007 = VERTEX_POINT ( 'NONE', #35341 ) ;
#17008 = CARTESIAN_POINT ( 'NONE',  ( -44.94597344681493922, 2.143131898507880377E-16, 82.56828755692798438 ) ) ;
#17009 = ORIENTED_EDGE ( 'NONE', *, *, #17476, .F. ) ;
#17010 =( NAMED_UNIT ( * ) SI_UNIT ( $, .STERADIAN. ) SOLID_ANGLE_UNIT ( ) );
#17011 = LINE ( 'NONE', #36790, #20411 ) ;
#17012 = CARTESIAN_POINT ( 'NONE',  ( -6.695973446814940111, 1.750000000000024203, -119.1817124430720440 ) ) ;
#17013 = CARTESIAN_POINT ( 'NONE',  ( 153.3040265531850537, -1.750000000000009992, -159.1817124430720298 ) ) ;
#17014 = VECTOR ( 'NONE', #44252, 1000.000000000000000 ) ;
#17015 = CARTESIAN_POINT ( 'NONE',  ( 195.0540265531851105, 2.143131898507880377E-16, 165.0000000000000000 ) ) ;
#17016 = DIRECTION ( 'NONE',  ( -6.938893903907233308E-16, 1.000000000000000000, 0.000000000000000000 ) ) ;
#17017 = CARTESIAN_POINT ( 'NONE',  ( -126.6959734468149321, 1.749999999999996891, 0.8182875569279768335 ) ) ;
#17018 = VERTEX_POINT ( 'NONE', #24025 ) ;
#17019 = DIRECTION ( 'NONE',  ( -0.000000000000000000, -0.000000000000000000, -1.000000000000000000 ) ) ;
#17020 = CYLINDRICAL_SURFACE ( 'NONE', #37578, 1.750000000000001554 ) ;
#17021 = CYLINDRICAL_SURFACE ( 'NONE', #34838, 1.750000000000036193 ) ;
#17022 =( BOUNDED_CURVE ( )  B_SPLINE_CURVE ( 3, ( #17984, #21861, #48989, #13875 ),
 .UNSPECIFIED., .F., .F. ) 
 B_SPLINE_CURVE_WITH_KNOTS ( ( 4, 4 ),
 ( 1.570796326794896558, 3.141592653589793116 ),
 .UNSPECIFIED. ) 
 CURVE ( )  GEOMETRIC_REPRESENTATION_ITEM ( )  RATIONAL_B_SPLINE_CURVE ( ( 1.000000000000000000, 0.8047378541243649375, 0.8047378541243649375, 1.000000000000000000 ) ) 
 REPRESENTATION_ITEM ( '' )  );
#17023 = CARTESIAN_POINT ( 'NONE',  ( -3.566525152643847285, 1.569997364305458776, 9.741991644046965604 ) ) ;
#17024 = EDGE_LOOP ( 'NONE', ( #20037, #15917, #27588, #16687, #9601, #16220, #47932, #25547, #37089, #19342, #24428, #50016 ) ) ;
#17025 = DIRECTION ( 'NONE',  ( -0.000000000000000000, -0.000000000000000000, -1.000000000000000000 ) ) ;
#17026 = VERTEX_POINT ( 'NONE', #20407 ) ;
#17027 = CARTESIAN_POINT ( 'NONE',  ( -5.325039556154594678, 2.676059031921508513, 6.606856988583542645E-16 ) ) ;
#17028 =( BOUNDED_CURVE ( )  B_SPLINE_CURVE ( 3, ( #17008, #16516, #23704, #48261 ),
 .UNSPECIFIED., .F., .F. ) 
 B_SPLINE_CURVE_WITH_KNOTS ( ( 4, 4 ),
 ( 3.141592653589793116, 4.712388980384689674 ),
 .UNSPECIFIED. ) 
 CURVE ( )  GEOMETRIC_REPRESENTATION_ITEM ( )  RATIONAL_B_SPLINE_CURVE ( ( 1.000000000000000000, 0.8047378541243649375, 0.8047378541243649375, 1.000000000000000000 ) ) 
 REPRESENTATION_ITEM ( '' )  );
#17029 = CARTESIAN_POINT ( 'NONE',  ( 73.30402655318508209, -1.750000000000009992, 0.8182875569279768335 ) ) ;
#17030 = CARTESIAN_POINT ( 'NONE',  ( -167.7210997126620384, 1.750000000000010436, 119.7931612910808781 ) ) ;
#17031 = ORIENTED_EDGE ( 'NONE', *, *, #12381, .T. ) ;
#17032 = EDGE_CURVE ( 'NONE', #2259, #10372, #15562, .T. ) ;
#17033 = CARTESIAN_POINT ( 'NONE',  ( 0.3370904143228981575, -0.2449105217885261532, 10.00000000000000000 ) ) ;
#17034 = CARTESIAN_POINT ( 'NONE',  ( 12.16428377685533135, 11.73151505502934988, -9.008049429158100807 ) ) ;
#17035 = B_SPLINE_CURVE_WITH_KNOTS ( 'NONE', 3,
 ( #47973, #21067, #36753, #48965 ),
 .UNSPECIFIED., .F., .F.,
 ( 4, 4 ),
 ( 0.000000000000000000, 0.002368422649471300760 ),
 .UNSPECIFIED. ) ;
#17036 = LINE ( 'NONE', #9592, #19613 ) ;
#17037 = CARTESIAN_POINT ( 'NONE',  ( -165.6708471809677974, -1.750000000000009548, 81.84341382277507648 ) ) ;
#17038 = ADVANCED_FACE ( 'NONE', ( #39435 ), #23772, .F. ) ;
#17039 =( BOUNDED_CURVE ( )  B_SPLINE_CURVE ( 3, ( #30182, #42238, #10186, #30442 ),
 .UNSPECIFIED., .F., .F. ) 
 B_SPLINE_CURVE_WITH_KNOTS ( ( 4, 4 ),
 ( 0.000000000000000000, 1.570796326794896558 ),
 .UNSPECIFIED. ) 
 CURVE ( )  GEOMETRIC_REPRESENTATION_ITEM ( )  RATIONAL_B_SPLINE_CURVE ( ( 1.000000000000000000, 0.8047378541243649375, 0.8047378541243649375, 1.000000000000000000 ) ) 
 REPRESENTATION_ITEM ( '' )  );
#17040 = ORIENTED_EDGE ( 'NONE', *, *, #27535, .F. ) ;
#17041 = VERTEX_POINT ( 'NONE', #19906 ) ;
#17042 = CARTESIAN_POINT ( 'NONE',  ( -1.250000000000000222, 0.000000000000000000, -10.00000000000000000 ) ) ;
#17043 = EDGE_CURVE ( 'NONE', #17726, #43380, #31225, .T. ) ;
#17044 = LINE ( 'NONE', #36316, #32882 ) ;
#17045 = EDGE_CURVE ( 'NONE', #3886, #31711, #424, .T. ) ;
#17046 = ORIENTED_EDGE ( 'NONE', *, *, #37886, .T. ) ;
#17047 = VERTEX_POINT ( 'NONE', #43508 ) ;
#17048 = CARTESIAN_POINT ( 'NONE',  ( -1.019713130072858798, -3.848720492505054658, 6.098637220230962441E-17 ) ) ;
#17049 = CARTESIAN_POINT ( 'NONE',  ( 71.55402655318505367, 0.000000000000000000, 82.56828755692799859 ) ) ;
#17050 = DIRECTION ( 'NONE',  ( 0.000000000000000000, -1.000000000000000000, 0.000000000000000000 ) ) ;
#17051 = CARTESIAN_POINT ( 'NONE',  ( 111.5540265531850679, 0.000000000000000000, -120.9317124430720156 ) ) ;
#17052 = ORIENTED_EDGE ( 'NONE', *, *, #19924, .F. ) ;
#17053 = VERTEX_POINT ( 'NONE', #16071 ) ;
#17054 = VERTEX_POINT ( 'NONE', #27361 ) ;
#17055 = EDGE_CURVE ( 'NONE', #48113, #5629, #49573, .T. ) ;
#17056 = DIRECTION ( 'NONE',  ( -0.000000000000000000, 1.000000000000000000, 0.000000000000000000 ) ) ;
#17057 = CARTESIAN_POINT ( 'NONE',  ( 341.9999999999999432, -169.0000000000001137, -349.9999999999998863 ) ) ;
#17058 = ORIENTED_EDGE ( 'NONE', *, *, #44355, .F. ) ;
#17059 = EDGE_LOOP ( 'NONE', ( #9401, #2479, #3015, #3540, #43921 ) ) ;
#17060 = CARTESIAN_POINT ( 'NONE',  ( -7.721099712662037540, -1.750000000000023537, -78.15658617722490931 ) ) ;
#17061 = DIRECTION ( 'NONE',  ( 0.000000000000000000, -1.000000000000000000, 0.000000000000000000 ) ) ;
#17062 = EDGE_LOOP ( 'NONE', ( #9853, #3969, #13213, #28036 ) ) ;
#17063 = EDGE_CURVE ( 'NONE', #2158, #7144, #7374, .T. ) ;
#17064 = ADVANCED_FACE ( 'NONE', ( #46815 ), #12461, .F. ) ;
#17065 = ORIENTED_EDGE ( 'NONE', *, *, #25589, .T. ) ;
#17066 = FACE_OUTER_BOUND ( 'NONE', #17062, .T. ) ;
#17067 = CARTESIAN_POINT ( 'NONE',  ( -46.33529284216709243, 19.19803090445757121, -8.466730184410787174 ) ) ;
#17068 = ORIENTED_EDGE ( 'NONE', *, *, #48982, .T. ) ;
#17069 = EDGE_CURVE ( 'NONE', #21648, #46923, #7877, .T. ) ;
#17070 = DIRECTION ( 'NONE',  ( -0.9928768384869219865, 0.000000000000000000, -0.1191452206184307749 ) ) ;
#17071 = FACE_BOUND ( 'NONE', #25720, .T. ) ;
#17072 = CARTESIAN_POINT ( 'NONE',  ( 0.000000000000000000, 181.0000000000000284, 341.9999999999997726 ) ) ;
#17073 = EDGE_CURVE ( 'NONE', #27540, #26544, #13217, .T. ) ;
#17074 = DIRECTION ( 'NONE',  ( 1.000000000000000000, 0.000000000000000000, 0.000000000000000000 ) ) ;
#17075 = EDGE_LOOP ( 'NONE', ( #34419, #11876, #45667, #18560 ) ) ;
#17076 = ADVANCED_FACE ( 'NONE', ( #25039 ), #28877, .F. ) ;
#17077 = CARTESIAN_POINT ( 'NONE',  ( 195.0540265531851105, 2.143131898507880377E-16, 165.0000000000000000 ) ) ;
#17078 = EDGE_CURVE ( 'NONE', #42683, #46160, #24489, .T. ) ;
#17079 = FACE_OUTER_BOUND ( 'NONE', #5664, .T. ) ;
#17080 = CARTESIAN_POINT ( 'NONE',  ( -119.9999999999990905, 16.00000000000000000, -24.99999999999999289 ) ) ;
#17081 = CARTESIAN_POINT ( 'NONE',  ( 21.60170755165891521, -30.69732439037074911, -6.568693074176334967 ) ) ;
#17082 = VECTOR ( 'NONE', #41123, 1000.000000000000000 ) ;
#17083 =( BOUNDED_CURVE ( )  B_SPLINE_CURVE ( 3, ( #46944, #19785, #50, #307 ),
 .UNSPECIFIED., .F., .F. ) 
 B_SPLINE_CURVE_WITH_KNOTS ( ( 4, 4 ),
 ( 0.000000000000000000, 1.570796326794896558 ),
 .UNSPECIFIED. ) 
 CURVE ( )  GEOMETRIC_REPRESENTATION_ITEM ( )  RATIONAL_B_SPLINE_CURVE ( ( 1.000000000000000000, 0.8047378541243649375, 0.8047378541243649375, 1.000000000000000000 ) ) 
 REPRESENTATION_ITEM ( '' )  );
#17084 = CARTESIAN_POINT ( 'NONE',  ( 6.875132362119187768, -33.14667368551891258, 8.356839323120299312 ) ) ;
#17085 = FACE_OUTER_BOUND ( 'NONE', #21015, .T. ) ;
#17086 = CARTESIAN_POINT ( 'NONE',  ( -1.655785408455817675, -0.7536129375911022610, 9.903764339332079558 ) ) ;
#17087 = ADVANCED_FACE ( 'NONE', ( #36858 ), #2187, .T. ) ;
#17088 = CARTESIAN_POINT ( 'NONE',  ( 135.0000000000012790, 17.00000000000000000, 5.000000000000004441 ) ) ;
#17089 = ORIENTED_EDGE ( 'NONE', *, *, #15929, .T. ) ;
#17090 = CARTESIAN_POINT ( 'NONE',  ( 72.27890028733797578, -1.750000000000009548, -160.2068387089191219 ) ) ;
#17091 = EDGE_CURVE ( 'NONE', #35246, #7644, #28614, .T. ) ;
#17092 = EDGE_CURVE ( 'NONE', #921, #11040, #8911, .T. ) ;
#17093 = DIRECTION ( 'NONE',  ( -1.000000000000000000, 0.000000000000000000, 0.000000000000000000 ) ) ;
#17094 = CARTESIAN_POINT ( 'NONE',  ( -164.9999999999987779, 17.00000000000000000, 5.000000000000004441 ) ) ;
#17095 = CYLINDRICAL_SURFACE ( 'NONE', #17580, 1.750000000000001554 ) ;
#17096 = CARTESIAN_POINT ( 'NONE',  ( 240.0000000000000000, -175.0000000000000000, 444.9999999999998295 ) ) ;
#17097 = EDGE_LOOP ( 'NONE', ( #31766, #10654, #19404, #46347, #34873, #19988 ) ) ;
#17098 = CARTESIAN_POINT ( 'NONE',  ( 181.0000000000000284, -174.9999999999999716, -111.0000000000001563 ) ) ;
#17099 = PRODUCT ( 'housing door', 'housing door', '', ( #28999 ) ) ;
#17100 = ORIENTED_EDGE ( 'NONE', *, *, #41675, .T. ) ;
#17101 = CARTESIAN_POINT ( 'NONE',  ( -166.6959734468149463, 1.750000000000010214, -39.18171244307202983 ) ) ;
#17102 = EDGE_CURVE ( 'NONE', #49685, #16572, #40928, .T. ) ;
#17103 = CARTESIAN_POINT ( 'NONE',  ( 31.55402655318503236, -1.025126265847089657, -120.9317124430720440 ) ) ;
#17104 = VERTEX_POINT ( 'NONE', #44253 ) ;
#17105 = DIRECTION ( 'NONE',  ( -1.000000000000000000, 0.000000000000000000, 0.000000000000000000 ) ) ;
#17106 = LINE ( 'NONE', #5043, #22442 ) ;
#17107 = VERTEX_POINT ( 'NONE', #17823 ) ;
#17108 = ORIENTED_EDGE ( 'NONE', *, *, #5599, .T. ) ;
#17109 = CARTESIAN_POINT ( 'NONE',  ( -4.999999999999999112, 222.4999999999999716, -228.6347188485896140 ) ) ;
#17110 = VERTEX_POINT ( 'NONE', #41170 ) ;
#17111 = EDGE_CURVE ( 'NONE', #35640, #35926, #32492, .T. ) ;
#17112 = CARTESIAN_POINT ( 'NONE',  ( 115.0540265531850395, 2.143131898507847836E-16, 79.06828755692798438 ) ) ;
#17113 = FACE_OUTER_BOUND ( 'NONE', #14843, .T. ) ;
#17114 = VECTOR ( 'NONE', #8379, 1000.000000000000000 ) ;
#17115 = LINE ( 'NONE', #9417, #49602 ) ;
#17116 = ORIENTED_EDGE ( 'NONE', *, *, #16161, .T. ) ;
#17117 = VECTOR ( 'NONE', #40009, 1000.000000000000000 ) ;
#17118 = CARTESIAN_POINT ( 'NONE',  ( 0.000000000000000000, 23.48684210526316107, -3.750000000000000000 ) ) ;
#17119 = ORIENTED_EDGE ( 'NONE', *, *, #8791, .T. ) ;
#17120 =( BOUNDED_CURVE ( )  B_SPLINE_CURVE ( 3, ( #26398, #35653, #47631, #23571 ),
 .UNSPECIFIED., .F., .F. ) 
 B_SPLINE_CURVE_WITH_KNOTS ( ( 4, 4 ),
 ( 4.712388980384689674, 6.283185307179586232 ),
 .UNSPECIFIED. ) 
 CURVE ( )  GEOMETRIC_REPRESENTATION_ITEM ( )  RATIONAL_B_SPLINE_CURVE ( ( 1.000000000000000000, 0.8047378541243649375, 0.8047378541243649375, 1.000000000000000000 ) ) 
 REPRESENTATION_ITEM ( '' )  );
#17121 = EDGE_CURVE ( 'NONE', #14780, #7447, #49082, .T. ) ;
#17122 = VERTEX_POINT ( 'NONE', #1683 ) ;
#17123 = VERTEX_POINT ( 'NONE', #17323 ) ;
#17124 = CARTESIAN_POINT ( 'NONE',  ( 14.48769039275578407, 30.44468701195595983, 8.807470649214879543 ) ) ;
#17125 = VECTOR ( 'NONE', #22120, 1000.000000000000000 ) ;
#17126 = CIRCLE ( 'NONE', #9751, 1.750000000000015543 ) ;
#17127 = LINE ( 'NONE', #13517, #4538 ) ;
#17128 = VERTEX_POINT ( 'NONE', #44995 ) ;
#17129 = AXIS2_PLACEMENT_3D ( 'NONE', #41799, #6649, #21542 ) ;
#17130 = CARTESIAN_POINT ( 'NONE',  ( -9.260964247899874380, 13.84230907185616744, -9.683996418299976483 ) ) ;
#17131 = CARTESIAN_POINT ( 'NONE',  ( -34.76907794179056310, 14.14424844080176236, -5.338708898921615820 ) ) ;
#17132 = CARTESIAN_POINT ( 'NONE',  ( -64.99999999999815259, 16.00000000000000000, 65.00000000000000000 ) ) ;
#17133 = ADVANCED_FACE ( 'NONE', ( #40433 ), #37365, .F. ) ;
#17134 = CARTESIAN_POINT ( 'NONE',  ( 113.3040265531850537, 1.749999999999997113, -39.18171244307202983 ) ) ;
#17135 = DIRECTION ( 'NONE',  ( 0.000000000000000000, 1.000000000000000000, 0.000000000000000000 ) ) ;
#17136 = EDGE_CURVE ( 'NONE', #42553, #46647, #20314, .T. ) ;
#17137 = CARTESIAN_POINT ( 'NONE',  ( 28.55116071645549525, -41.05976639056858346, -2.408242355805840784 ) ) ;
#17138 = PLANE ( 'NONE',  #45495 ) ;
#17139 = EDGE_CURVE ( 'NONE', #4161, #18435, #33495, .T. ) ;
#17140 = CARTESIAN_POINT ( 'NONE',  ( 0.9985466430067150290, 1.124040728742683903, 9.944962737436837230 ) ) ;
#17141 = PLANE ( 'NONE',  #679 ) ;
#17142 = EDGE_CURVE ( 'NONE', #9269, #9029, #44004, .T. ) ;
#17143 = EDGE_CURVE ( 'NONE', #29017, #25893, #28378, .T. ) ;
#17144 = CARTESIAN_POINT ( 'NONE',  ( -33.14391172085785797, -37.72293746533094350, -8.016098858316205167 ) ) ;
#17145 = CARTESIAN_POINT ( 'NONE',  ( -15.80799809827351154, 29.65358618225718956, -8.016098858316199838 ) ) ;
#17146 = ORIENTED_EDGE ( 'NONE', *, *, #25699, .T. ) ;
#17147 = CARTESIAN_POINT ( 'NONE',  ( -128.4459734468149179, 0.000000000000000000, 165.0000000000000000 ) ) ;
#17148 = CARTESIAN_POINT ( 'NONE',  ( 35.05402655318504657, -1.025126265847089657, -80.93171244307201562 ) ) ;
#17149 = DIRECTION ( 'NONE',  ( 0.000000000000000000, 1.000000000000000000, 0.000000000000000000 ) ) ;
#17150 = CARTESIAN_POINT ( 'NONE',  ( 181.0000000000000000, -182.9999999999999716, -115.0000000000001279 ) ) ;
#17151 = AXIS2_PLACEMENT_3D ( 'NONE', #13734, #13979, #33506 ) ;
#17152 = ORIENTED_EDGE ( 'NONE', *, *, #17977, .T. ) ;
#17153 = AXIS2_PLACEMENT_3D ( 'NONE', #39629, #8831, #12665 ) ;
#17154 = B_SPLINE_CURVE_WITH_KNOTS ( 'NONE', 3,
 ( #45448, #40637, #18266, #1883 ),
 .UNSPECIFIED., .F., .F.,
 ( 4, 4 ),
 ( 0.0003760194760206989387, 0.0006307719036365364972 ),
 .UNSPECIFIED. ) ;
#17155 = ADVANCED_FACE ( 'NONE', ( #36346, #40179 ), #5014, .T. ) ;
#17156 = DIRECTION ( 'NONE',  ( 0.4055129968046615185, -0.4055129968046615185, -0.8192181753629524943 ) ) ;
#17157 = VERTEX_POINT ( 'NONE', #16827 ) ;
#17158 = DIRECTION ( 'NONE',  ( -3.363195139050033768E-16, -0.7071067811865474617, -0.7071067811865475727 ) ) ;
#17159 = DIRECTION ( 'NONE',  ( 0.000000000000000000, 0.000000000000000000, -1.000000000000000000 ) ) ;
#17160 = VECTOR ( 'NONE', #16387, 1000.000000000000000 ) ;
#17161 = FACE_OUTER_BOUND ( 'NONE', #44945, .T. ) ;
#17162 = ORIENTED_EDGE ( 'NONE', *, *, #6265, .F. ) ;
#17163 = CARTESIAN_POINT ( 'NONE',  ( -65.00000000000002842, 17.00000000000000000, -114.9999999999999858 ) ) ;
#17164 = ORIENTED_EDGE ( 'NONE', *, *, #21501, .T. ) ;
#17165 = ORIENTED_EDGE ( 'NONE', *, *, #46483, .T. ) ;
#17166 = VECTOR ( 'NONE', #28146, 1000.000000000000114 ) ;
#17167 = ORIENTED_EDGE ( 'NONE', *, *, #6401, .F. ) ;
#17168 = CARTESIAN_POINT ( 'NONE',  ( -175.0000000000000000, 0.000000000000000000, -122.5000000000000000 ) ) ;
#17169 = CARTESIAN_POINT ( 'NONE',  ( 210.0000000000000568, 0.000000000000000000, 42.56828755692799149 ) ) ;
#17170 = ORIENTED_EDGE ( 'NONE', *, *, #46152, .T. ) ;
#17171 = FACE_OUTER_BOUND ( 'NONE', #27795, .T. ) ;
#17172 = DIRECTION ( 'NONE',  ( -1.000000000000000000, -0.000000000000000000, -0.000000000000000000 ) ) ;
#17173 = FACE_OUTER_BOUND ( 'NONE', #6621, .T. ) ;
#17174 = B_SPLINE_CURVE_WITH_KNOTS ( 'NONE', 3,
 ( #26790, #22929, #42418, #15489 ),
 .UNSPECIFIED., .F., .F.,
 ( 4, 4 ),
 ( 0.0002936521407534355859, 0.0006663369986142269122 ),
 .UNSPECIFIED. ) ;
#17175 = CARTESIAN_POINT ( 'NONE',  ( -16.37555114979269888, 29.24217402453077597, -8.466730184410787174 ) ) ;
#17176 = ORIENTED_EDGE ( 'NONE', *, *, #36041, .F. ) ;
#17177 = DIRECTION ( 'NONE',  ( 1.000000000000000000, 0.000000000000000000, 0.000000000000000000 ) ) ;
#17178 =( BOUNDED_CURVE ( )  B_SPLINE_CURVE ( 3, ( #31235, #49892, #46570, #14802 ),
 .UNSPECIFIED., .F., .F. ) 
 B_SPLINE_CURVE_WITH_KNOTS ( ( 4, 4 ),
 ( 3.141592653589793116, 4.712388980384689674 ),
 .UNSPECIFIED. ) 
 CURVE ( )  GEOMETRIC_REPRESENTATION_ITEM ( )  RATIONAL_B_SPLINE_CURVE ( ( 1.000000000000000000, 0.8047378541243649375, 0.8047378541243649375, 1.000000000000000000 ) ) 
 REPRESENTATION_ITEM ( '' )  );
#17179 = ORIENTED_EDGE ( 'NONE', *, *, #17960, .F. ) ;
#17180 = CARTESIAN_POINT ( 'NONE',  ( 210.0000000000000568, 0.000000000000000000, 2.568287556927987048 ) ) ;
#17181 = CARTESIAN_POINT ( 'NONE',  ( -5.647304616913629616, 296.6525076104601339, 145.3277671506088780 ) ) ;
#17182 = ORIENTED_EDGE ( 'NONE', *, *, #12727, .T. ) ;
#17183 = VERTEX_POINT ( 'NONE', #32728 ) ;
#17184 = ORIENTED_EDGE ( 'NONE', *, *, #49451, .F. ) ;
#17185 = DIRECTION ( 'NONE',  ( -0.000000000000000000, -1.000000000000000000, -0.000000000000000000 ) ) ;
#17186 =( BOUNDED_CURVE ( )  B_SPLINE_CURVE ( 3, ( #2242, #49890, #45571, #18386 ),
 .UNSPECIFIED., .F., .F. ) 
 B_SPLINE_CURVE_WITH_KNOTS ( ( 4, 4 ),
 ( 4.712388980384689674, 6.283185307179586232 ),
 .UNSPECIFIED. ) 
 CURVE ( )  GEOMETRIC_REPRESENTATION_ITEM ( )  RATIONAL_B_SPLINE_CURVE ( ( 1.000000000000000000, 0.8047378541243649375, 0.8047378541243649375, 1.000000000000000000 ) ) 
 REPRESENTATION_ITEM ( '' )  );
#17187 = CARTESIAN_POINT ( 'NONE',  ( 71.55402655318505367, 0.000000000000000000, -0.9317124430720524764 ) ) ;
#17188 = EDGE_LOOP ( 'NONE', ( #17568, #29235, #15363, #5262 ) ) ;
#17189 = AXIS2_PLACEMENT_3D ( 'NONE', #11558, #27206, #8470 ) ;
#17190 = VECTOR ( 'NONE', #19743, 1000.000000000000000 ) ;
#17191 = CARTESIAN_POINT ( 'NONE',  ( -12.35406723005387875, 11.51001571518090039, 9.178419661560148768 ) ) ;
#17192 = DIRECTION ( 'NONE',  ( 0.000000000000000000, 0.000000000000000000, 1.000000000000000000 ) ) ;
#17193 = CARTESIAN_POINT ( 'NONE',  ( 12.78770032058947237, 31.68259716188277864, 7.455576670931136185 ) ) ;
#17194 = EDGE_CURVE ( 'NONE', #8176, #29055, #42628, .T. ) ;
#17195 = VECTOR ( 'NONE', #19032, 1000.000000000000000 ) ;
#17196 = EDGE_CURVE ( 'NONE', #26544, #19216, #6449, .T. ) ;
#17197 = VERTEX_POINT ( 'NONE', #18822 ) ;
#17198 = FACE_OUTER_BOUND ( 'NONE', #14106, .T. ) ;
#17199 = FACE_OUTER_BOUND ( 'NONE', #49114, .T. ) ;
#17200 = VECTOR ( 'NONE', #38227, 1000.000000000000000 ) ;
#17201 = EDGE_CURVE ( 'NONE', #5410, #42631, #10390, .T. ) ;
#17202 = CARTESIAN_POINT ( 'NONE',  ( 0.000000000000000000, 13.98684210526316107, 0.000000000000000000 ) ) ;
#17203 = ORIENTED_EDGE ( 'NONE', *, *, #28126, .F. ) ;
#17204 = ORIENTED_EDGE ( 'NONE', *, *, #13890, .F. ) ;
#17205 = EDGE_CURVE ( 'NONE', #42094, #30761, #49331, .T. ) ;
#17206 = CONTEXT_DEPENDENT_SHAPE_REPRESENTATION ( #7623, #35648 ) ;
#17207 = EDGE_CURVE ( 'NONE', #38997, #11761, #34504, .T. ) ;
#17209 = DIRECTION ( 'NONE',  ( 0.000000000000000000, 0.000000000000000000, -1.000000000000000000 ) ) ;
#17208 = AXIS2_PLACEMENT_3D ( 'NONE', #48170, #32330, #13059 ) ;
#17210 = CARTESIAN_POINT ( 'NONE',  ( 1.468446590252912465, 0.3226319952343980058, 9.953784399990622589 ) ) ;
#17211 = CARTESIAN_POINT ( 'NONE',  ( -5.000000000000000000, 184.8000000000000114, -359.8000000000002387 ) ) ;
#17212 = CARTESIAN_POINT ( 'NONE',  ( -49.46074318306826001, 9.578883844007169301, 8.807470649214879543 ) ) ;
#17213 = ORIENTED_EDGE ( 'NONE', *, *, #18007, .F. ) ;
#17214 = CARTESIAN_POINT ( 'NONE',  ( 113.3040265531850537, 1.749999999999997335, -79.18171244307201562 ) ) ;
#17215 = ADVANCED_FACE ( 'NONE', ( #3430 ), #26797, .T. ) ;
#17216 = DIRECTION ( 'NONE',  ( 0.000000000000000000, -0.000000000000000000, -1.000000000000000000 ) ) ;
#17217 = DIRECTION ( 'NONE',  ( 0.000000000000000000, 0.000000000000000000, 1.000000000000000000 ) ) ;
#17218 = DIRECTION ( 'NONE',  ( 1.000000000000000000, 0.000000000000000000, 0.000000000000000000 ) ) ;
#17219 = ORIENTED_EDGE ( 'NONE', *, *, #14183, .F. ) ;
#17220 = CARTESIAN_POINT ( 'NONE',  ( -167.7210997126620384, 1.750000000000009326, 1.843413822775066269 ) ) ;
#17221 = EDGE_LOOP ( 'NONE', ( #23851, #29486, #49988, #36437, #44988 ) ) ;
#17222 = DIRECTION ( 'NONE',  ( 0.000000000000000000, -1.000000000000000000, 2.406552799042969348E-16 ) ) ;
#17223 = ORIENTED_EDGE ( 'NONE', *, *, #18160, .F. ) ;
#17224 = CARTESIAN_POINT ( 'NONE',  ( 193.3040265531851105, -1.750000000000010658, -79.18171244307201562 ) ) ;
#17225 = FACE_OUTER_BOUND ( 'NONE', #31455, .T. ) ;
#17226 = ORIENTED_EDGE ( 'NONE', *, *, #33700, .F. ) ;
#17227 = AXIS2_PLACEMENT_3D ( 'NONE', #30937, #3447, #35297 ) ;
#17228 = AXIS2_PLACEMENT_3D ( 'NONE', #22639, #45196, #3128 ) ;
#17229 = CARTESIAN_POINT ( 'NONE',  ( -204.9459734468149463, 2.143131898507880377E-16, -80.93171244307201562 ) ) ;
#17230 = ORIENTED_EDGE ( 'NONE', *, *, #41579, .F. ) ;
#17231 = VECTOR ( 'NONE', #38358, 1000.000000000000000 ) ;
#17232 = CARTESIAN_POINT ( 'NONE',  ( 210.0000000000000568, 0.000000000000000000, -79.18171244307201562 ) ) ;
#17234 = VECTOR ( 'NONE', #9626, 1000.000000000000000 ) ;
#17233 = LINE ( 'NONE', #32899, #34743 ) ;
#17235 = CYLINDRICAL_SURFACE ( 'NONE', #5730, 1.750000000000001554 ) ;
#17236 = DIRECTION ( 'NONE',  ( -1.000000000000000000, 0.000000000000000000, 0.000000000000000000 ) ) ;
#17237 = AXIS2_PLACEMENT_3D ( 'NONE', #36662, #5569, #8920 ) ;
#17238 = CARTESIAN_POINT ( 'NONE',  ( -5.647304616913629616, 2.688010569040066411, 741.9425600500172777 ) ) ;
#17239 = VECTOR ( 'NONE', #37974, 1000.000000000000000 ) ;
#17240 = ORIENTED_EDGE ( 'NONE', *, *, #47108, .F. ) ;
#17241 = ORIENTED_EDGE ( 'NONE', *, *, #21949, .F. ) ;
#17242 = CARTESIAN_POINT ( 'NONE',  ( 168.9999999999999716, -252.4999999999999432, -349.9999999999999432 ) ) ;
#17243 = EDGE_CURVE ( 'NONE', #50656, #3572, #6785, .T. ) ;
#17244 = VERTEX_POINT ( 'NONE', #10629 ) ;
#17245 = CARTESIAN_POINT ( 'NONE',  ( 113.3040265531850537, -1.749999999999997335, 80.81828755692798438 ) ) ;
#17246 = DIRECTION ( 'NONE',  ( 0.000000000000000000, -1.000000000000000000, 1.604368532695312981E-16 ) ) ;
#17247 = EDGE_LOOP ( 'NONE', ( #10263, #11730, #48254, #2782, #43801, #36395 ) ) ;
#17248 = LINE ( 'NONE', #9049, #7387 ) ;
#17249 = LINE ( 'NONE', #17497, #21825 ) ;
#17250 = ORIENTED_EDGE ( 'NONE', *, *, #30204, .F. ) ;
#17251 = PLANE ( 'NONE',  #13706 ) ;
#17252 = CARTESIAN_POINT ( 'NONE',  ( 0.3862712429686810944, 1.188820645368943607, -10.00000000000000000 ) ) ;
#17253 = DIRECTION ( 'NONE',  ( 1.000000000000000000, 0.000000000000000000, 7.793956916774525800E-48 ) ) ;
#17254 = LINE ( 'NONE', #21868, #24775 ) ;
#17255 = ORIENTED_EDGE ( 'NONE', *, *, #27826, .T. ) ;
#17256 = VERTEX_POINT ( 'NONE', #37857 ) ;
#17257 = ORIENTED_EDGE ( 'NONE', *, *, #14535, .T. ) ;
#17258 = DIRECTION ( 'NONE',  ( -1.000000000000000000, 0.000000000000000000, 0.000000000000000000 ) ) ;
#17259 = LINE ( 'NONE', #13151, #43902 ) ;
#17260 = PLANE ( 'NONE',  #9329 ) ;
#17261 = PLANE ( 'NONE',  #28867 ) ;
#17262 = ORIENTED_EDGE ( 'NONE', *, *, #18699, .F. ) ;
#17263 = CARTESIAN_POINT ( 'NONE',  ( 210.0000000000000568, 0.000000000000000000, -157.4317124430720298 ) ) ;
#17265 = EDGE_LOOP ( 'NONE', ( #41646, #19848, #50387, #39155 ) ) ;
#17264 = VECTOR ( 'NONE', #45830, 1000.000000000000000 ) ;
#17266 = DIRECTION ( 'NONE',  ( -0.000000000000000000, -0.000000000000000000, -1.000000000000000000 ) ) ;
#17267 = CARTESIAN_POINT ( 'NONE',  ( 210.0000000000000568, 0.000000000000000000, 40.81828755692798438 ) ) ;
#17268 = CARTESIAN_POINT ( 'NONE',  ( 35.00000000000061107, 17.00000000000000000, -54.99999999999999289 ) ) ;
#17269 = VECTOR ( 'NONE', #1896, 1000.000000000000000 ) ;
#17270 = DIRECTION ( 'NONE',  ( -1.000000000000000000, -0.000000000000000000, -0.000000000000000000 ) ) ;
#17271 = FACE_OUTER_BOUND ( 'NONE', #7589, .T. ) ;
#17272 = CARTESIAN_POINT ( 'NONE',  ( -164.9999999999997442, 17.00000000000000000, -60.00000000000000000 ) ) ;
#17273 = EDGE_LOOP ( 'NONE', ( #3198, #9953, #28796, #42069 ) ) ;
#17274 = ADVANCED_FACE ( 'NONE', ( #33996 ), #22685, .F. ) ;
#17275 = DIRECTION ( 'NONE',  ( -6.765175596986472868E-16, 0.9749645535258953943, -0.2223603367690637489 ) ) ;
#17276 = VECTOR ( 'NONE', #46169, 1000.000000000000114 ) ;
#17278 = AXIS2_PLACEMENT_3D ( 'NONE', #44386, #2070, #13351 ) ;
#17277 = DIRECTION ( 'NONE',  ( 0.000000000000000000, -0.000000000000000000, 1.000000000000000000 ) ) ;
#17279 = CARTESIAN_POINT ( 'NONE',  ( -15.00099850811941948, -7.462898891544107016, 9.403735324607438884 ) ) ;
#17280 = B_SPLINE_CURVE_WITH_KNOTS ( 'NONE', 3,
 ( #29246, #21042, #48691, #9995 ),
 .UNSPECIFIED., .F., .F.,
 ( 4, 4 ),
 ( 0.009557256062580683775, 0.01933991692386597544 ),
 .UNSPECIFIED. ) ;
#17281 = PLANE ( 'NONE',  #23217 ) ;
#17282 = ORIENTED_EDGE ( 'NONE', *, *, #15864, .T. ) ;
#17283 = CARTESIAN_POINT ( 'NONE',  ( 72.27890028733797578, 1.750000000000010436, -80.20683870891910772 ) ) ;
#17284 = VERTEX_POINT ( 'NONE', #13968 ) ;
#17285 = CYLINDRICAL_SURFACE ( 'NONE', #39330, 1.749999999999987566 ) ;
#17286 = CARTESIAN_POINT ( 'NONE',  ( -69.99999999999816680, 17.00000000000000000, 90.00000000000000000 ) ) ;
#17287 = EDGE_LOOP ( 'NONE', ( #21700, #46426, #16363, #36527 ) ) ;
#17288 = PLANE ( 'NONE',  #45856 ) ;
#17289 = CARTESIAN_POINT ( 'NONE',  ( 17.43089236541784359, 28.36237856644539690, 3.199614146704519602 ) ) ;
#17290 = CARTESIAN_POINT ( 'NONE',  ( -29.61572577327014955, -16.11461842845715253, 8.807470649214879543 ) ) ;
#17291 = CARTESIAN_POINT ( 'NONE',  ( 0.3862712429686727678, 1.188820645368945605, 10.00000000000000000 ) ) ;
#17292 = ORIENTED_EDGE ( 'NONE', *, *, #45237, .T. ) ;
#17293 = VERTEX_POINT ( 'NONE', #49827 ) ;
#17294 = CARTESIAN_POINT ( 'NONE',  ( -0.3656201545664206076, 2.182515578491385000, 9.881002359080270026 ) ) ;
#17295 = CARTESIAN_POINT ( 'NONE',  ( 344.0000000000000568, 165.0000000000000000, 349.9999999999998295 ) ) ;
#17296 = ADVANCED_FACE ( 'NONE', ( #41938 ), #46252, .F. ) ;
#17297 = AXIS2_PLACEMENT_3D ( 'NONE', #50111, #47037, #42213 ) ;
#17298 = ORIENTED_EDGE ( 'NONE', *, *, #40091, .T. ) ;
#17299 = ORIENTED_EDGE ( 'NONE', *, *, #50304, .F. ) ;
#17300 = DIRECTION ( 'NONE',  ( -0.000000000000000000, -0.000000000000000000, 1.000000000000000000 ) ) ;
#17301 = CARTESIAN_POINT ( 'NONE',  ( -86.69597344681494633, 1.750000000000010658, 80.81828755692798438 ) ) ;
#17302 = CARTESIAN_POINT ( 'NONE',  ( -20.08067494016849608, -41.72051557472617134, 7.455576670931136185 ) ) ;
#17303 = CARTESIAN_POINT ( 'NONE',  ( 112.2789002873379758, -1.749999999999996891, 79.79316129108087807 ) ) ;
#17304 = ORIENTED_EDGE ( 'NONE', *, *, #40896, .F. ) ;
#17305 = VERTEX_POINT ( 'NONE', #29628 ) ;
#17306 = ORIENTED_EDGE ( 'NONE', *, *, #46650, .T. ) ;
#17307 = VECTOR ( 'NONE', #27585, 1000.000000000000114 ) ;
#17308 = DIRECTION ( 'NONE',  ( -0.1191452206184307749, 0.000000000000000000, 0.9928768384869220975 ) ) ;
#17309 = DIRECTION ( 'NONE',  ( -0.000000000000000000, -1.000000000000000000, -0.000000000000000000 ) ) ;
#17310 = VERTEX_POINT ( 'NONE', #45246 ) ;
#17311 = VERTEX_POINT ( 'NONE', #22937 ) ;
#17312 = CARTESIAN_POINT ( 'NONE',  ( 35.05402655318504657, 2.143131898507880377E-16, -0.9317124430720247208 ) ) ;
#17313 = DIRECTION ( 'NONE',  ( -1.000000000000000000, -0.000000000000000000, -0.000000000000000000 ) ) ;
#17314 = ORIENTED_EDGE ( 'NONE', *, *, #25466, .T. ) ;
#17315 = ORIENTED_EDGE ( 'NONE', *, *, #19752, .T. ) ;
#17316 = DIRECTION ( 'NONE',  ( -0.000000000000000000, -0.000000000000000000, -1.000000000000000000 ) ) ;
#17317 = CARTESIAN_POINT ( 'NONE',  ( 9.358026734184097251, 6.123233995736766282E-16, 5.000000000000000000 ) ) ;
#17318 = ORIENTED_EDGE ( 'NONE', *, *, #23988, .T. ) ;
#17319 = LINE ( 'NONE', #48324, #48733 ) ;
#17320 =( BOUNDED_CURVE ( )  B_SPLINE_CURVE ( 3, ( #13106, #44392, #9267, #24927 ),
 .UNSPECIFIED., .F., .F. ) 
 B_SPLINE_CURVE_WITH_KNOTS ( ( 4, 4 ),
 ( 1.570796326794896558, 3.141592653589793116 ),
 .UNSPECIFIED. ) 
 CURVE ( )  GEOMETRIC_REPRESENTATION_ITEM ( )  RATIONAL_B_SPLINE_CURVE ( ( 1.000000000000000000, 0.8047378541243649375, 0.8047378541243649375, 1.000000000000000000 ) ) 
 REPRESENTATION_ITEM ( '' )  );
#17321 = DIRECTION ( 'NONE',  ( 0.000000000000000000, 0.000000000000000000, 1.000000000000000000 ) ) ;
#17322 = CYLINDRICAL_SURFACE ( 'NONE', #8820, 2.000000000000001776 ) ;
#17323 = CARTESIAN_POINT ( 'NONE',  ( 113.3040265531850537, -1.749999999999996891, -159.1817124430720298 ) ) ;
#17324 = CARTESIAN_POINT ( 'NONE',  ( -204.9459734468149463, 2.143131898507880377E-16, 165.0000000000000000 ) ) ;
#17325 = ORIENTED_EDGE ( 'NONE', *, *, #2361, .T. ) ;
#17326 = EDGE_CURVE ( 'NONE', #936, #48234, #21936, .T. ) ;
#17327 = CARTESIAN_POINT ( 'NONE',  ( -6.695973446814940111, 1.750000000000023315, 160.8182875569279702 ) ) ;
#17328 =( BOUNDED_CURVE ( )  B_SPLINE_CURVE ( 3, ( #14157, #33443, #21114, #21884 ),
 .UNSPECIFIED., .F., .F. ) 
 B_SPLINE_CURVE_WITH_KNOTS ( ( 4, 4 ),
 ( 3.141592653589793116, 4.712388980384689674 ),
 .UNSPECIFIED. ) 
 CURVE ( )  GEOMETRIC_REPRESENTATION_ITEM ( )  RATIONAL_B_SPLINE_CURVE ( ( 1.000000000000000000, 0.8047378541243649375, 0.8047378541243649375, 1.000000000000000000 ) ) 
 REPRESENTATION_ITEM ( '' )  );
#17329 = VECTOR ( 'NONE', #43933, 1000.000000000000000 ) ;
#17330 = CARTESIAN_POINT ( 'NONE',  ( 2.500000000000002665, 204.9999999999999716, -230.2499999999999716 ) ) ;
#17331 = CARTESIAN_POINT ( 'NONE',  ( -8.843309649387274263, 14.11631751497152720, -2.870787844569587133 ) ) ;
#17332 = CARTESIAN_POINT ( 'NONE',  ( 339.9999999999999432, 169.0000000000000000, -340.0000000000001705 ) ) ;
#17333 = VECTOR ( 'NONE', #8436, 1000.000000000000000 ) ;
#17334 = DIRECTION ( 'NONE',  ( 0.000000000000000000, 0.000000000000000000, 1.000000000000000000 ) ) ;
#17335 = CARTESIAN_POINT ( 'NONE',  ( 31.55402655318503236, -1.025126265847089879, 122.5682875569280128 ) ) ;
#17336 = EDGE_CURVE ( 'NONE', #15017, #49245, #14736, .T. ) ;
#17337 = EDGE_CURVE ( 'NONE', #44970, #34157, #41294, .T. ) ;
#17338 =( BOUNDED_CURVE ( )  B_SPLINE_CURVE ( 3, ( #32746, #12471, #1452, #35856 ),
 .UNSPECIFIED., .F., .F. ) 
 B_SPLINE_CURVE_WITH_KNOTS ( ( 4, 4 ),
 ( 3.141592653589793116, 4.712388980384689674 ),
 .UNSPECIFIED. ) 
 CURVE ( )  GEOMETRIC_REPRESENTATION_ITEM ( )  RATIONAL_B_SPLINE_CURVE ( ( 1.000000000000000000, 0.8047378541243649375, 0.8047378541243649375, 1.000000000000000000 ) ) 
 REPRESENTATION_ITEM ( '' )  );
#17339 = AXIS2_PLACEMENT_3D ( 'NONE', #9021, #41253, #43907 ) ;
#17340 = EDGE_CURVE ( 'NONE', #12862, #34493, #26292, .T. ) ;
#17341 = ORIENTED_EDGE ( 'NONE', *, *, #1387, .T. ) ;
#17342 = CARTESIAN_POINT ( 'NONE',  ( 112.2789002873379758, 1.749999999999996669, 121.8434138227750481 ) ) ;
#17343 = CARTESIAN_POINT ( 'NONE',  ( -0.3862712429686895876, 1.188820645368940720, -3.333333333333333481 ) ) ;
#17344 = CYLINDRICAL_SURFACE ( 'NONE', #46644, 1.750000000000008438 ) ;
#17345 = DIRECTION ( 'NONE',  ( 0.000000000000000000, -1.000000000000000000, 0.000000000000000000 ) ) ;
#17346 = CARTESIAN_POINT ( 'NONE',  ( 210.0000000000000568, 0.000000000000000000, -117.4317124430720298 ) ) ;
#17347 = EDGE_LOOP ( 'NONE', ( #1661, #44789 ) ) ;
#17348 = DIRECTION ( 'NONE',  ( 0.000000000000000000, 0.000000000000000000, -1.000000000000000000 ) ) ;
#17349 = ADVANCED_FACE ( 'NONE', ( #10885 ), #38103, .F. ) ;
#17351 = ORIENTED_EDGE ( 'NONE', *, *, #35942, .T. ) ;
#17350 = EDGE_CURVE ( 'NONE', #25227, #42832, #42179, .T. ) ;
#17352 = FACE_OUTER_BOUND ( 'NONE', #40126, .T. ) ;
#17353 = CARTESIAN_POINT ( 'NONE',  ( 111.5540265531850679, 0.000000000000000000, 119.0682875569279844 ) ) ;
#17354 = EDGE_CURVE ( 'NONE', #42166, #39210, #20102, .T. ) ;
#17355 = EDGE_CURVE ( 'NONE', #16242, #34818, #28059, .T. ) ;
#17356 = ORIENTED_EDGE ( 'NONE', *, *, #32906, .T. ) ;
#17357 = CARTESIAN_POINT ( 'NONE',  ( 33.30402655318503946, 1.750000000000010658, 80.81828755692798438 ) ) ;
#17358 = CARTESIAN_POINT ( 'NONE',  ( 0.000000000000000000, 165.2000000000000171, 340.1999999999997044 ) ) ;
#17359 = VERTEX_POINT ( 'NONE', #31681 ) ;
#17360 = VERTEX_POINT ( 'NONE', #30917 ) ;
#17361 = VECTOR ( 'NONE', #18503, 1000.000000000000000 ) ;
#17362 = EDGE_CURVE ( 'NONE', #17487, #3809, #7023, .T. ) ;
#17363 = DIRECTION ( 'NONE',  ( 1.000000000000000000, 0.000000000000000000, 0.000000000000000000 ) ) ;
#17364 = CARTESIAN_POINT ( 'NONE',  ( -124.9459734468149321, -1.025126265847081442, -160.9317124430720014 ) ) ;
#17365 = CARTESIAN_POINT ( 'NONE',  ( 210.0000000000000568, 0.000000000000000000, 80.81828755692798438 ) ) ;
#17366 = ORIENTED_EDGE ( 'NONE', *, *, #5322, .F. ) ;
#17367 = DIRECTION ( 'NONE',  ( -0.9928768384869220975, 0.000000000000000000, -0.1191452206184309970 ) ) ;
#17368 = AXIS2_PLACEMENT_3D ( 'NONE', #50604, #27574, #19350 ) ;
#17369 = CARTESIAN_POINT ( 'NONE',  ( 339.9999999999999432, -168.9999999999999432, -356.0000000000002274 ) ) ;
#17370 = LINE ( 'NONE', #13005, #796 ) ;
#17371 = EDGE_LOOP ( 'NONE', ( #12439, #6982, #34152, #8714 ) ) ;
#17372 = ORIENTED_EDGE ( 'NONE', *, *, #41861, .T. ) ;
#17373 = ORIENTED_EDGE ( 'NONE', *, *, #33766, .T. ) ;
#17374 = CARTESIAN_POINT ( 'NONE',  ( 130.0000000000021032, 17.00000000000000000, 115.0000000000000142 ) ) ;
#17375 = EDGE_LOOP ( 'NONE', ( #9909, #26028, #19517, #39259 ) ) ;
#17376 = ADVANCED_FACE ( 'NONE', ( #11653, #8320 ), #7554, .T. ) ;
#17377 = CARTESIAN_POINT ( 'NONE',  ( 210.0000000000000568, 0.000000000000000000, -117.4317124430720298 ) ) ;
#17378 = DIRECTION ( 'NONE',  ( -1.000000000000000000, -0.000000000000000000, -0.000000000000000000 ) ) ;
#17379 = EDGE_CURVE ( 'NONE', #35747, #2019, #15495, .T. ) ;
#17380 = DIRECTION ( 'NONE',  ( -1.000000000000000000, -0.000000000000000000, -0.000000000000000000 ) ) ;
#17381 = CARTESIAN_POINT ( 'NONE',  ( 181.0000000000000000, -9.999999999999953815, -350.0000000000001705 ) ) ;
#17382 = EDGE_CURVE ( 'NONE', #49918, #24712, #31162, .T. ) ;
#17383 = CARTESIAN_POINT ( 'NONE',  ( -204.9459734468149463, 2.143131898507880377E-16, 42.56828755692798438 ) ) ;
#17384 = CARTESIAN_POINT ( 'NONE',  ( 7.398363427652525637, -15.19415887381133246, -9.008049429158100807 ) ) ;
#17385 = ADVANCED_FACE ( 'NONE', ( #47524 ), #116, .T. ) ;
#17386 = CARTESIAN_POINT ( 'NONE',  ( 154.1026953830863420, 103.9380105690400597, -17.65743994998277699 ) ) ;
#17387 = AXIS2_PLACEMENT_3D ( 'NONE', #43233, #27605, #19632 ) ;
#17388 = DIRECTION ( 'NONE',  ( 0.000000000000000000, 0.000000000000000000, 1.000000000000000000 ) ) ;
#17389 = DIRECTION ( 'NONE',  ( -0.000000000000000000, -0.000000000000000000, -1.000000000000000000 ) ) ;
#17390 = EDGE_CURVE ( 'NONE', #40762, #10372, #23305, .T. ) ;
#17391 = CARTESIAN_POINT ( 'NONE',  ( 48.99656738986517723, -11.00747004110342431, 1.847720168420772691 ) ) ;
#17392 = CARTESIAN_POINT ( 'NONE',  ( 192.2789002873380184, -1.750000000000009548, 159.7931612910809065 ) ) ;
#17393 = VECTOR ( 'NONE', #24836, 1000.000000000000000 ) ;
#17394 = ORIENTED_EDGE ( 'NONE', *, *, #34464, .F. ) ;
#17395 = CARTESIAN_POINT ( 'NONE',  ( -204.9459734468149463, 2.143131898507880377E-16, 82.56828755692798438 ) ) ;
#17396 = AXIS2_PLACEMENT_3D ( 'NONE', #7283, #35265, #22676 ) ;
#17397 = LINE ( 'NONE', #24851, #24556 ) ;
#17398 = FACE_OUTER_BOUND ( 'NONE', #8887, .T. ) ;
#17399 = DIRECTION ( 'NONE',  ( 0.000000000000000000, -0.000000000000000000, 1.000000000000000000 ) ) ;
#17400 = PRESENTATION_LAYER_ASSIGNMENT (  '', '', ( #35483 ) ) ;
#17401 = ORIENTED_EDGE ( 'NONE', *, *, #16557, .T. ) ;
#17402 = CYLINDRICAL_SURFACE ( 'NONE', #33055, 1.750000000000001554 ) ;
#17403 = VECTOR ( 'NONE', #43862, 1000.000000000000000 ) ;
#17404 = CARTESIAN_POINT ( 'NONE',  ( -47.72109971266203132, 1.750000000000009548, 161.8434138227750907 ) ) ;
#17405 = EDGE_CURVE ( 'NONE', #17745, #5629, #31417, .T. ) ;
#17406 = ORIENTED_EDGE ( 'NONE', *, *, #37116, .T. ) ;
#17407 = CARTESIAN_POINT ( 'NONE',  ( 34.08355720199905647, -2.371364769369109116, 7.455576670931136185 ) ) ;
#17408 = LINE ( 'NONE', #40259, #37165 ) ;
#17409 = CARTESIAN_POINT ( 'NONE',  ( 169.0000000000000000, -168.9999999999999432, -115.0000000000001847 ) ) ;
#17410 = EDGE_LOOP ( 'NONE', ( #2221, #12143, #39517, #48413, #607, #16804, #28416, #32829 ) ) ;
#17411 = FACE_OUTER_BOUND ( 'NONE', #42020, .T. ) ;
#17412 = ORIENTED_EDGE ( 'NONE', *, *, #45287, .F. ) ;
#17413 = ORIENTED_EDGE ( 'NONE', *, *, #28513, .F. ) ;
#17414 = CARTESIAN_POINT ( 'NONE',  ( 153.3040265531850537, 0.000000000000000000, 165.0000000000000000 ) ) ;
#17415 = EDGE_CURVE ( 'NONE', #38712, #18511, #39619, .T. ) ;
#17416 = ADVANCED_FACE ( 'NONE', ( #46753 ), #46500, .F. ) ;
#17417 = ORIENTED_EDGE ( 'NONE', *, *, #26161, .T. ) ;
#17418 = CARTESIAN_POINT ( 'NONE',  ( 191.5540265531851105, 0.000000000000000000, 79.06828755692797017 ) ) ;
#17419 = CARTESIAN_POINT ( 'NONE',  ( -5.888214538810513154, -16.20866436362413410, 8.727788335465566760 ) ) ;
#17420 = EDGE_LOOP ( 'NONE', ( #45228, #39412, #24729, #37967, #3080 ) ) ;
#17421 = CARTESIAN_POINT ( 'NONE',  ( 153.3040265531850537, -1.750000000000010658, 80.81828755692798438 ) ) ;
#17422 = DIRECTION ( 'NONE',  ( 1.000000000000000000, -4.758098676964956461E-16, -8.975803739141899931E-48 ) ) ;
#17423 = ADVANCED_FACE ( 'NONE', ( #42936, #8568 ), #7816, .T. ) ;
#17424 = CARTESIAN_POINT ( 'NONE',  ( -167.4999999999999432, -62.49999999999998579, -10.00000000000000000 ) ) ;
#17425 = VECTOR ( 'NONE', #38019, 1000.000000000000000 ) ;
#17426 = EDGE_CURVE ( 'NONE', #45594, #28550, #8070, .T. ) ;
#17427 = ORIENTED_EDGE ( 'NONE', *, *, #8974, .F. ) ;
#17428 = EDGE_CURVE ( 'NONE', #1861, #26957, #47119, .T. ) ;
#17429 = DIRECTION ( 'NONE',  ( 0.000000000000000000, 0.000000000000000000, 1.000000000000000000 ) ) ;
#17430 = EDGE_LOOP ( 'NONE', ( #1030, #7963, #9916, #13006, #13568, #28415 ) ) ;
#17431 = LINE ( 'NONE', #13813, #49666 ) ;
#17432 = CARTESIAN_POINT ( 'NONE',  ( -14.99999999999876366, 17.00000000000000000, 30.00000000000000000 ) ) ;
#17433 = VERTEX_POINT ( 'NONE', #3690 ) ;
#17434 = AXIS2_PLACEMENT_3D ( 'NONE', #26036, #27755, #571 ) ;
#17435 = EDGE_LOOP ( 'NONE', ( #16721, #3077, #45773, #42995 ) ) ;
#17436 = VERTEX_POINT ( 'NONE', #39125 ) ;
#17437 = LINE ( 'NONE', #37709, #17200 ) ;
#17438 = AXIS2_PLACEMENT_3D ( 'NONE', #43574, #40001, #20234 ) ;
#17439 = CARTESIAN_POINT ( 'NONE',  ( -166.6959734468149463, -1.750000000000010658, 120.8182875569279702 ) ) ;
#17440 = ORIENTED_EDGE ( 'NONE', *, *, #7340, .F. ) ;
#17441 = VECTOR ( 'NONE', #7953, 1000.000000000000000 ) ;
#17442 = CARTESIAN_POINT ( 'NONE',  ( -1.150625731496824011, 0.4126014017553036872, 9.969517326150318937 ) ) ;
#17443 = CARTESIAN_POINT ( 'NONE',  ( -2.569099690548740877, 33.19126772784019153, 3.199614146704519602 ) ) ;
#17444 = CARTESIAN_POINT ( 'NONE',  ( 193.3040265531851105, 1.750000000000009992, 160.8182875569279702 ) ) ;
#17445 = EDGE_CURVE ( 'NONE', #38893, #8676, #36071, .T. ) ;
#17446 = AXIS2_PLACEMENT_3D ( 'NONE', #45441, #21363, #9574 ) ;
#17447 = ORIENTED_EDGE ( 'NONE', *, *, #47446, .T. ) ;
#17448 = DIRECTION ( 'NONE',  ( 3.172065745548403743E-16, 1.000000000000000000, 0.000000000000000000 ) ) ;
#17449 = DIRECTION ( 'NONE',  ( -0.000000000000000000, -1.000000000000000000, -0.000000000000000000 ) ) ;
#17450 = CARTESIAN_POINT ( 'NONE',  ( 75.05402655318509630, 1.025126265847089879, -117.4317124430720156 ) ) ;
#17451 = PRODUCT_DEFINITION ( 'UNKNOWN', '', #11918, #4202 ) ;
#17452 = EDGE_LOOP ( 'NONE', ( #16302, #19775, #39038, #9226 ) ) ;
#17453 = DIRECTION ( 'NONE',  ( 1.000000000000000000, 0.000000000000000000, 0.000000000000000000 ) ) ;
#17454 = DIRECTION ( 'NONE',  ( 7.793956916774525800E-48, 0.000000000000000000, -1.000000000000000000 ) ) ;
#17455 = DIRECTION ( 'NONE',  ( 0.000000000000000000, 0.000000000000000000, 1.000000000000000000 ) ) ;
#17456 = FACE_OUTER_BOUND ( 'NONE', #45392, .T. ) ;
#17457 = ORIENTED_EDGE ( 'NONE', *, *, #5098, .T. ) ;
#17458 = CARTESIAN_POINT ( 'NONE',  ( -166.6959734468149463, 0.000000000000000000, 165.0000000000000000 ) ) ;
#17459 = EDGE_CURVE ( 'NONE', #44566, #36764, #3947, .T. ) ;
#17460 = CARTESIAN_POINT ( 'NONE',  ( -64.99999999999877787, 16.00000000000000000, 30.00000000000000000 ) ) ;
#17461 = FACE_OUTER_BOUND ( 'NONE', #44318, .T. ) ;
#17462 = CARTESIAN_POINT ( 'NONE',  ( 10.00000000000000000, -250.0000000000000000, 225.0000000000000000 ) ) ;
#17463 = FACE_OUTER_BOUND ( 'NONE', #6567, .T. ) ;
#17464 = ORIENTED_EDGE ( 'NONE', *, *, #41775, .F. ) ;
#17465 = CARTESIAN_POINT ( 'NONE',  ( 359.9999999999998863, -183.3431457505076310, 358.3431457505074036 ) ) ;
#17466 = ORIENTED_EDGE ( 'NONE', *, *, #28847, .T. ) ;
#17467 = CARTESIAN_POINT ( 'NONE',  ( 11.73320209285708415, -11.96063479729170886, 9.403735324607438884 ) ) ;
#17468 = ORIENTED_EDGE ( 'NONE', *, *, #22040, .F. ) ;
#17469 = DIRECTION ( 'NONE',  ( 1.000000000000000000, 0.000000000000000000, 0.000000000000000000 ) ) ;
#17470 = VECTOR ( 'NONE', #675, 1000.000000000000000 ) ;
#17471 = PLANE ( 'NONE',  #28211 ) ;
#17472 = EDGE_LOOP ( 'NONE', ( #39390, #20154, #42873, #19111, #9138, #50434, #3408, #48512 ) ) ;
#17473 = CIRCLE ( 'NONE', #43650, 0.5000000000000000000 ) ;
#17474 = EDGE_CURVE ( 'NONE', #46647, #40582, #46497, .T. ) ;
#17475 = CARTESIAN_POINT ( 'NONE',  ( -14.99999999999876366, 17.00000000000000000, 5.000000000000004441 ) ) ;
#17476 = EDGE_CURVE ( 'NONE', #21871, #32124, #12730, .T. ) ;
#17477 = VECTOR ( 'NONE', #39063, 1000.000000000000000 ) ;
#17478 = ORIENTED_EDGE ( 'NONE', *, *, #45007, .F. ) ;
#17479 = CARTESIAN_POINT ( 'NONE',  ( -86.69597344681494633, 1.750000000000009992, 0.8182875569279768335 ) ) ;
#17480 = CARTESIAN_POINT ( 'NONE',  ( -19.99999999999940670, 17.00000000000000000, -54.99999999999999289 ) ) ;
#17481 = PLANE ( 'NONE',  #38543 ) ;
#17482 = CARTESIAN_POINT ( 'NONE',  ( -1.540526284687967706, 1.371707213411501147, 9.886433018048069954 ) ) ;
#17483 = CARTESIAN_POINT ( 'NONE',  ( 32.43949840348898306, 7.871562655726499713, -9.367992836599954742 ) ) ;
#17484 =( BOUNDED_CURVE ( )  B_SPLINE_CURVE ( 3, ( #38865, #27305, #3689, #12402 ),
 .UNSPECIFIED., .F., .F. ) 
 B_SPLINE_CURVE_WITH_KNOTS ( ( 4, 4 ),
 ( 4.712388980384689674, 6.283185307179586232 ),
 .UNSPECIFIED. ) 
 CURVE ( )  GEOMETRIC_REPRESENTATION_ITEM ( )  RATIONAL_B_SPLINE_CURVE ( ( 1.000000000000000000, 0.8047378541243649375, 0.8047378541243649375, 1.000000000000000000 ) ) 
 REPRESENTATION_ITEM ( '' )  );
#17485 = EDGE_LOOP ( 'NONE', ( #5929, #3503, #12201, #46522, #2936, #979 ) ) ;
#17486 = EDGE_CURVE ( 'NONE', #49286, #9722, #33189, .T. ) ;
#17487 = VERTEX_POINT ( 'NONE', #24725 ) ;
#17488 = DIRECTION ( 'NONE',  ( 0.000000000000000000, 1.000000000000000000, 0.000000000000000000 ) ) ;
#17489 = ADVANCED_FACE ( 'NONE', ( #47764 ), #36288, .T. ) ;
#17490 = EDGE_CURVE ( 'NONE', #36250, #34589, #995, .T. ) ;
#17491 = ORIENTED_EDGE ( 'NONE', *, *, #14289, .T. ) ;
#17492 = CARTESIAN_POINT ( 'NONE',  ( 115.0540265531850395, 2.143131898507847836E-16, 165.0000000000000000 ) ) ;
#17493 = CARTESIAN_POINT ( 'NONE',  ( 44.99506233596246574, 23.32283626942318477, 7.455576670931136185 ) ) ;
#17494 = EDGE_LOOP ( 'NONE', ( #45934, #1920, #10030, #608 ) ) ;
#17495 = DIRECTION ( 'NONE',  ( 0.000000000000000000, 0.000000000000000000, 1.000000000000000000 ) ) ;
#17496 = EDGE_CURVE ( 'NONE', #20578, #27386, #13667, .T. ) ;
#17497 = CARTESIAN_POINT ( 'NONE',  ( 164.9999999999999716, 17.00000000000000000, -30.00000000000001421 ) ) ;
#17498 = ORIENTED_EDGE ( 'NONE', *, *, #19984, .F. ) ;
#17499 = CARTESIAN_POINT ( 'NONE',  ( -7.216980890441389462, 6.922079660550276792, 0.000000000000000000 ) ) ;
#17500 = CARTESIAN_POINT ( 'NONE',  ( -15.45175104485246820, 6.222373774239106758, -2.870787844569587133 ) ) ;
#17501 = CARTESIAN_POINT ( 'NONE',  ( 31.55402655318503236, -1.025126265847089213, -0.9317124430720324924 ) ) ;
#17502 = ORIENTED_EDGE ( 'NONE', *, *, #12886, .F. ) ;
#17503 = ORIENTED_EDGE ( 'NONE', *, *, #8254, .T. ) ;
#17504 = AXIS2_PLACEMENT_3D ( 'NONE', #33250, #44497, #25037 ) ;
#17505 = AXIS2_PLACEMENT_3D ( 'NONE', #40333, #78, #16483 ) ;
#17506 = ORIENTED_EDGE ( 'NONE', *, *, #45038, .T. ) ;
#17507 = CARTESIAN_POINT ( 'NONE',  ( 343.9999999999999432, -174.9999999999999716, 355.9999999999998295 ) ) ;
#17508 = CARTESIAN_POINT ( 'NONE',  ( -19.99999999999815969, 17.00000000000000000, 90.00000000000000000 ) ) ;
#17509 = VECTOR ( 'NONE', #7438, 1000.000000000000000 ) ;
#17510 = DIRECTION ( 'NONE',  ( 1.000000000000000000, 0.000000000000000000, 7.793956916774525800E-48 ) ) ;
#17511 = ORIENTED_EDGE ( 'NONE', *, *, #41392, .F. ) ;
#17512 = VECTOR ( 'NONE', #48968, 1000.000000000000000 ) ;
#17513 = CARTESIAN_POINT ( 'NONE',  ( -50.00000000000000000, 50.00000000000000000, 900.0000000000000000 ) ) ;
#17514 = ORIENTED_EDGE ( 'NONE', *, *, #15062, .F. ) ;
#17515 = AXIS2_PLACEMENT_3D ( 'NONE', #31801, #32302, #1255 ) ;
#17516 = LINE ( 'NONE', #43690, #40890 ) ;
#17517 = DIRECTION ( 'NONE',  ( 0.000000000000000000, -0.4027858274925602000, -0.9152942571496522906 ) ) ;
#17518 = DIRECTION ( 'NONE',  ( -1.000000000000000000, -0.000000000000000000, -0.000000000000000000 ) ) ;
#17519 = CARTESIAN_POINT ( 'NONE',  ( 350.0000000000000000, -168.9999999999999432, -356.0000000000002274 ) ) ;
#17520 = CARTESIAN_POINT ( 'NONE',  ( 15.00000000000000000, 8.875661936878628921, -18.94832733001756253 ) ) ;
#17521 = DIRECTION ( 'NONE',  ( -1.000000000000000000, 0.000000000000000000, 0.000000000000000000 ) ) ;
#17522 = ORIENTED_EDGE ( 'NONE', *, *, #37753, .F. ) ;
#17523 = CARTESIAN_POINT ( 'NONE',  ( 181.0000000000000284, -9.999999999999953815, -115.0000000000001563 ) ) ;
#17524 = B_SPLINE_SURFACE_WITH_KNOTS ( 'NONE', 3, 3, ( 
 ( #41500, #17145, #1504, #28944 ),
 ( #33561, #21745, #37178, #21240 ),
 ( #10203, #32560, #33314, #29444 ),
 ( #29204, #44555, #5339, #44820 ) ),
 .UNSPECIFIED., .F., .F., .F.,
 ( 4, 4 ),
 ( 4, 4 ),
 ( 0.000000000000000000, 1.000000000000000000 ),
 ( 0.000000000000000000, 1.000000000000000000 ),
 .UNSPECIFIED. ) ;
#17525 = DIRECTION ( 'NONE',  ( 0.000000000000000000, 0.000000000000000000, 1.000000000000000000 ) ) ;
#17526 = CARTESIAN_POINT ( 'NONE',  ( 0.000000000000000000, 13.98684210526316107, 0.000000000000000000 ) ) ;
#17527 = ADVANCED_FACE ( 'NONE', ( #9569, #24473 ), #28313, .T. ) ;
#17528 = VECTOR ( 'NONE', #39171, 1000.000000000000000 ) ;
#17529 = CARTESIAN_POINT ( 'NONE',  ( 33.64889274059390090, -3.704246042440748621, 8.356839323120299312 ) ) ;
#17530 = ORIENTED_EDGE ( 'NONE', *, *, #11070, .F. ) ;
#17531 = CARTESIAN_POINT ( 'NONE',  ( -23.31729631074215092, -24.19776167542410406, -8.016098858316199838 ) ) ;
#17532 = ORIENTED_EDGE ( 'NONE', *, *, #26140, .T. ) ;
#17533 = CARTESIAN_POINT ( 'NONE',  ( 71.55402655318505367, 0.000000000000000000, -77.43171244307198720 ) ) ;
#17534 = CARTESIAN_POINT ( 'NONE',  ( 181.0000000000000284, 2.775557561562891351E-14, -95.00000000000014211 ) ) ;
#17535 = B_SPLINE_CURVE_WITH_KNOTS ( 'NONE', 3,
 ( #40188, #5024, #20684, #1201 ),
 .UNSPECIFIED., .F., .F.,
 ( 4, 4 ),
 ( 0.0009679537044783566389, 0.001281751046851271805 ),
 .UNSPECIFIED. ) ;
#17536 = CARTESIAN_POINT ( 'NONE',  ( 0.3370904143228924954, 0.2449105217885333141, -10.00000000000000000 ) ) ;
#17537 = ORIENTED_EDGE ( 'NONE', *, *, #3272, .T. ) ;
#17538 = EDGE_CURVE ( 'NONE', #24424, #2781, #6241, .T. ) ;
#17539 = EDGE_CURVE ( 'NONE', #16006, #31946, #43950, .T. ) ;
#17540 = CARTESIAN_POINT ( 'NONE',  ( 12.78770032058947237, 31.68259716188277864, 7.455576670931136185 ) ) ;
#17541 = VECTOR ( 'NONE', #36184, 1000.000000000000000 ) ;
#17542 = LINE ( 'NONE', #33215, #9895 ) ;
#17543 = AXIS2_PLACEMENT_3D ( 'NONE', #26380, #49680, #29725 ) ;
#17544 = CARTESIAN_POINT ( 'NONE',  ( 340.0000000000000568, 181.0000000000000284, 355.9999999999997726 ) ) ;
#17545 = CARTESIAN_POINT ( 'NONE',  ( -207.7210997126620384, -1.750000000000009548, -40.20683870891912193 ) ) ;
#17546 = VECTOR ( 'NONE', #26996, 1000.000000000000000 ) ;
#17547 = ORIENTED_EDGE ( 'NONE', *, *, #41546, .F. ) ;
#17548 = ORIENTED_EDGE ( 'NONE', *, *, #49281, .T. ) ;
#17549 = CARTESIAN_POINT ( 'NONE',  ( 1.249999999999999778, -0.000000000000000000, -10.00000000000000000 ) ) ;
#17550 = CARTESIAN_POINT ( 'NONE',  ( 9.999999999999996447, -34.54492135858216528, -5.000000000000000000 ) ) ;
#17551 = ADVANCED_FACE ( 'NONE', ( #28818 ), #44439, .T. ) ;
#17552 = EDGE_CURVE ( 'NONE', #31866, #6992, #39070, .T. ) ;
#17553 = VERTEX_POINT ( 'NONE', #28562 ) ;
#17554 = ORIENTED_EDGE ( 'NONE', *, *, #17390, .T. ) ;
#17555 = CARTESIAN_POINT ( 'NONE',  ( -310.0878471510133068, -227.3959007404658337, 296.3011729072028402 ) ) ;
#17556 = CARTESIAN_POINT ( 'NONE',  ( 181.0000000000000000, -81.49999999999997158, -350.0000000000001705 ) ) ;
#17557 = CARTESIAN_POINT ( 'NONE',  ( -204.9459734468149463, 2.143131898507880377E-16, 79.06828755692797017 ) ) ;
#17558 = CARTESIAN_POINT ( 'NONE',  ( 210.0000000000000568, 0.000000000000000000, 82.56828755692799859 ) ) ;
#17559 = EDGE_LOOP ( 'NONE', ( #17000, #33083, #23343, #29731 ) ) ;
#17560 = ADVANCED_FACE ( 'NONE', ( #44194, #9068 ), #40372, .T. ) ;
#17561 = ORIENTED_EDGE ( 'NONE', *, *, #37371, .F. ) ;
#17562 = CARTESIAN_POINT ( 'NONE',  ( -115.0000000000000284, 17.00000000000000000, -114.9999999999999858 ) ) ;
#17563 = CARTESIAN_POINT ( 'NONE',  ( 195.0540265531851105, 1.025126265847089657, 119.0682875569279560 ) ) ;
#17564 = EDGE_LOOP ( 'NONE', ( #44991, #36940, #50339, #5321 ) ) ;
#17565 = EDGE_LOOP ( 'NONE', ( #27572, #44835, #7084 ) ) ;
#17566 = CARTESIAN_POINT ( 'NONE',  ( 0.000000000000000000, 165.2000000000000171, -340.2000000000001592 ) ) ;
#17567 = DIRECTION ( 'NONE',  ( 0.000000000000000000, 1.000000000000000000, 6.123233995736766036E-17 ) ) ;
#17568 = ORIENTED_EDGE ( 'NONE', *, *, #16397, .F. ) ;
#17569 = ORIENTED_EDGE ( 'NONE', *, *, #27525, .T. ) ;
#17570 = CARTESIAN_POINT ( 'NONE',  ( -5.000000000000000000, -165.1999999999999602, -340.2000000000001592 ) ) ;
#17571 = CARTESIAN_POINT ( 'NONE',  ( 240.0000000000000000, -175.0000000000000000, 32.29650858650035161 ) ) ;
#17572 = EDGE_LOOP ( 'NONE', ( #10599, #8197, #24951, #32710 ) ) ;
#17573 = PLANE ( 'NONE',  #36543 ) ;
#17574 = DIRECTION ( 'NONE',  ( 0.000000000000000000, 0.000000000000000000, 1.000000000000000000 ) ) ;
#17575 = CARTESIAN_POINT ( 'NONE',  ( 47.55282581475750447, 15.45084971874791080, 0.000000000000000000 ) ) ;
#17576 = DIRECTION ( 'NONE',  ( -1.000000000000000000, -0.000000000000000000, -0.000000000000000000 ) ) ;
#17577 = AXIS2_PLACEMENT_3D ( 'NONE', #5181, #16990, #36006 ) ;
#17578 = CARTESIAN_POINT ( 'NONE',  ( -44.94597344681493922, -1.025126265847089657, -120.9317124430720440 ) ) ;
#17579 = ORIENTED_EDGE ( 'NONE', *, *, #35008, .F. ) ;
#17580 = AXIS2_PLACEMENT_3D ( 'NONE', #9399, #40456, #25058 ) ;
#17581 = CARTESIAN_POINT ( 'NONE',  ( 113.3040265531850537, -1.749999999999997113, 40.81828755692798438 ) ) ;
#17582 = CARTESIAN_POINT ( 'NONE',  ( 48.99656738986517723, -11.00747004110342431, 1.847720168420772691 ) ) ;
#17583 = LINE ( 'NONE', #33257, #24491 ) ;
#17584 = LINE ( 'NONE', #48840, #29989 ) ;
#17585 = VECTOR ( 'NONE', #32654, 1000.000000000000000 ) ;
#17586 = EDGE_CURVE ( 'NONE', #25002, #43342, #40625, .T. ) ;
#17587 = CARTESIAN_POINT ( 'NONE',  ( 0.000000000000000000, 13.48684210526315930, 0.000000000000000000 ) ) ;
#17588 = CARTESIAN_POINT ( 'NONE',  ( 73.30402655318508209, -1.750000000000010658, 120.8182875569279702 ) ) ;
#17589 = CARTESIAN_POINT ( 'NONE',  ( -164.9999999999981526, 17.00000000000000000, 90.00000000000000000 ) ) ;
#17590 = CARTESIAN_POINT ( 'NONE',  ( -119.9999999999990905, 16.00000000000000000, -24.99999999999999289 ) ) ;
#17591 = DIRECTION ( 'NONE',  ( -0.000000000000000000, -0.000000000000000000, -1.000000000000000000 ) ) ;
#17592 = EDGE_LOOP ( 'NONE', ( #43898, #33419, #45551, #28779 ) ) ;
#17593 = CARTESIAN_POINT ( 'NONE',  ( -166.6959734468149463, 0.000000000000000000, 165.0000000000000000 ) ) ;
#17594 = VECTOR ( 'NONE', #38043, 1000.000000000000000 ) ;
#17595 = CARTESIAN_POINT ( 'NONE',  ( -166.6959734468149463, -1.750000000000009992, -159.1817124430720298 ) ) ;
#17596 = AXIS2_PLACEMENT_3D ( 'NONE', #6415, #6925, #34387 ) ;
#17597 = FACE_OUTER_BOUND ( 'NONE', #8574, .T. ) ;
#17598 = CARTESIAN_POINT ( 'NONE',  ( 1.377636575563020438, -0.6021164824561170414, 9.953784399990622589 ) ) ;
#17599 = LINE ( 'NONE', #6556, #49522 ) ;
#17600 = VERTEX_POINT ( 'NONE', #36792 ) ;
#17601 = DIRECTION ( 'NONE',  ( 0.000000000000000000, 1.000000000000000000, 0.000000000000000000 ) ) ;
#17602 = ORIENTED_EDGE ( 'NONE', *, *, #5113, .T. ) ;
#17603 = CARTESIAN_POINT ( 'NONE',  ( 0.3862712429686810944, 1.188820645368943607, 10.00000000000000000 ) ) ;
#17604 = CARTESIAN_POINT ( 'NONE',  ( -4.030066147382709296, 6.879218662320311317, 9.147955830346443662E-16 ) ) ;
#17605 = B_SPLINE_CURVE_WITH_KNOTS ( 'NONE', 3,
 ( #30617, #26764, #6750, #2644 ),
 .UNSPECIFIED., .F., .F.,
 ( 4, 4 ),
 ( 0.002911903035958271057, 0.009050416366962861503 ),
 .UNSPECIFIED. ) ;
#17606 = EDGE_LOOP ( 'NONE', ( #46281, #33202, #24703, #7043 ) ) ;
#17607 = CARTESIAN_POINT ( 'NONE',  ( -44.94597344681493922, 1.025126265847088991, 162.5682875569279133 ) ) ;
#17608 = FACE_OUTER_BOUND ( 'NONE', #46973, .T. ) ;
#17609 = AXIS2_PLACEMENT_3D ( 'NONE', #18358, #34040, #49622 ) ;
#17610 = ORIENTED_EDGE ( 'NONE', *, *, #5933, .F. ) ;
#17611 = ORIENTED_EDGE ( 'NONE', *, *, #37198, .F. ) ;
#17612 = EDGE_CURVE ( 'NONE', #39424, #30540, #23397, .T. ) ;
#17613 = CARTESIAN_POINT ( 'NONE',  ( -0.5349938414998356428, -3.214699992961246977, 9.799352050262458036 ) ) ;
#17614 = DIRECTION ( 'NONE',  ( 1.586032892321651989E-16, -3.736034562988530447E-32, 1.000000000000000000 ) ) ;
#17615 = CYLINDRICAL_SURFACE ( 'NONE', #3799, 1.750000000000001554 ) ;
#17616 =( BOUNDED_CURVE ( )  B_SPLINE_CURVE ( 3, ( #12356, #39839, #22766, #26104 ),
 .UNSPECIFIED., .F., .F. ) 
 B_SPLINE_CURVE_WITH_KNOTS ( ( 4, 4 ),
 ( 3.141592653589793116, 4.712388980384689674 ),
 .UNSPECIFIED. ) 
 CURVE ( )  GEOMETRIC_REPRESENTATION_ITEM ( )  RATIONAL_B_SPLINE_CURVE ( ( 1.000000000000000000, 0.8047378541243649375, 0.8047378541243649375, 1.000000000000000000 ) ) 
 REPRESENTATION_ITEM ( '' )  );
#17617 = VERTEX_POINT ( 'NONE', #34197 ) ;
#17618 = CARTESIAN_POINT ( 'NONE',  ( 40.00000000000000000, -7.564790863224926554, 897.6604670114604687 ) ) ;
#17619 = CYLINDRICAL_SURFACE ( 'NONE', #32913, 1.750000000000001554 ) ;
#17620 = LINE ( 'NONE', #44293, #9783 ) ;
#17621 = ORIENTED_EDGE ( 'NONE', *, *, #39119, .T. ) ;
#17622 = ORIENTED_EDGE ( 'NONE', *, *, #24988, .T. ) ;
#17623 = EDGE_LOOP ( 'NONE', ( #21089, #47045, #21870, #39460 ) ) ;
#17624 = CYLINDRICAL_SURFACE ( 'NONE', #38569, 1.750000000000008438 ) ;
#17625 =( BOUNDED_CURVE ( )  B_SPLINE_CURVE ( 3, ( #23859, #27956, #31821, #20501 ),
 .UNSPECIFIED., .F., .F. ) 
 B_SPLINE_CURVE_WITH_KNOTS ( ( 4, 4 ),
 ( 4.712388980384689674, 6.283185307179586232 ),
 .UNSPECIFIED. ) 
 CURVE ( )  GEOMETRIC_REPRESENTATION_ITEM ( )  RATIONAL_B_SPLINE_CURVE ( ( 1.000000000000000000, 0.8047378541243649375, 0.8047378541243649375, 1.000000000000000000 ) ) 
 REPRESENTATION_ITEM ( '' )  );
#17626 = DIRECTION ( 'NONE',  ( 1.000000000000000000, 0.000000000000000000, 0.000000000000000000 ) ) ;
#17627 = EDGE_LOOP ( 'NONE', ( #10411, #47365, #13749, #6859, #29432, #12945 ) ) ;
#17628 = EDGE_CURVE ( 'NONE', #14555, #23499, #42113, .T. ) ;
#17629 = CARTESIAN_POINT ( 'NONE',  ( -4.945973446814917018, -1.025126265847096985, -37.43171244307200851 ) ) ;
#17630 = CARTESIAN_POINT ( 'NONE',  ( -50.00000000000000000, -50.00000000000000000, 900.0000000000000000 ) ) ;
#17631 = AXIS2_PLACEMENT_3D ( 'NONE', #31250, #200, #34852 ) ;
#17632 = DIRECTION ( 'NONE',  ( 0.000000000000000000, 0.000000000000000000, -1.000000000000000000 ) ) ;
#17633 = CARTESIAN_POINT ( 'NONE',  ( -8.445973446814976526, 0.000000000000000000, 79.06828755692795596 ) ) ;
#17634 = CARTESIAN_POINT ( 'NONE',  ( 135.0000000000019043, 17.00000000000000000, 90.00000000000000000 ) ) ;
#17635 = AXIS2_PLACEMENT_3D ( 'NONE', #42747, #35356, #43010 ) ;
#17636 = CARTESIAN_POINT ( 'NONE',  ( 370.7621192902014968, -97.72914955339486198, -17.31629813440246579 ) ) ;
#17637 = FACE_OUTER_BOUND ( 'NONE', #33736, .T. ) ;
#17639 = VECTOR ( 'NONE', #4715, 1000.000000000000000 ) ;
#17638 = DIRECTION ( 'NONE',  ( -0.000000000000000000, -0.000000000000000000, -1.000000000000000000 ) ) ;
#17640 =( BOUNDED_CURVE ( )  B_SPLINE_CURVE ( 3, ( #50722, #39000, #39250, #19473 ),
 .UNSPECIFIED., .F., .F. ) 
 B_SPLINE_CURVE_WITH_KNOTS ( ( 4, 4 ),
 ( 3.141592653589849515, 4.712388980384676351 ),
 .UNSPECIFIED. ) 
 CURVE ( )  GEOMETRIC_REPRESENTATION_ITEM ( )  RATIONAL_B_SPLINE_CURVE ( ( 1.000000000000000000, 0.8047378541243814798, 0.8047378541243814798, 1.000000000000000000 ) ) 
 REPRESENTATION_ITEM ( '' )  );
#17641 = CARTESIAN_POINT ( 'NONE',  ( 344.0000000000000000, -165.0000000000001137, -349.9999999999999432 ) ) ;
#17642 = CARTESIAN_POINT ( 'NONE',  ( -23.29043492822808759, 24.10797434788186067, 1.847720168420772691 ) ) ;
#17643 = VECTOR ( 'NONE', #44440, 1000.000000000000000 ) ;
#17645 = VECTOR ( 'NONE', #6391, 1000.000000000000000 ) ;
#17644 = DIRECTION ( 'NONE',  ( 0.000000000000000000, 0.000000000000000000, -1.000000000000000000 ) ) ;
#17646 = VERTEX_POINT ( 'NONE', #50020 ) ;
#17647 = LINE ( 'NONE', #26097, #47448 ) ;
#17648 = FACE_OUTER_BOUND ( 'NONE', #36293, .T. ) ;
#17649 = AXIS2_PLACEMENT_3D ( 'NONE', #7494, #15180, #46182 ) ;
#17650 = VECTOR ( 'NONE', #31677, 1000.000000000000000 ) ;
#17651 = PLANE ( 'NONE',  #36117 ) ;
#17652 = EDGE_LOOP ( 'NONE', ( #30314, #37096, #11509, #12810, #33118 ) ) ;
#17653 = CARTESIAN_POINT ( 'NONE',  ( -88.44597344681494633, 1.025126265847089657, -120.9317124430720440 ) ) ;
#17654 = DIRECTION ( 'NONE',  ( -0.000000000000000000, -1.000000000000000000, -0.000000000000000000 ) ) ;
#17655 = VERTEX_POINT ( 'NONE', #30329 ) ;
#17656 = CARTESIAN_POINT ( 'NONE',  ( 1.270883027773819229, 0.2878889193223041487, 9.961922210043287151 ) ) ;
#17657 = CARTESIAN_POINT ( 'NONE',  ( 153.3040265531850537, 0.000000000000000000, 165.0000000000000000 ) ) ;
#17658 = CARTESIAN_POINT ( 'NONE',  ( 151.5540265531850537, 1.025126265847089435, -117.4317124430720156 ) ) ;
#17659 = LINE ( 'NONE', #49421, #24204 ) ;
#17660 = ORIENTED_EDGE ( 'NONE', *, *, #41934, .T. ) ;
#17661 = CARTESIAN_POINT ( 'NONE',  ( -15.00000000000001421, 17.00000000000000000, -90.00000000000000000 ) ) ;
#17662 = VERTEX_POINT ( 'NONE', #45938 ) ;
#17663 = ORIENTED_EDGE ( 'NONE', *, *, #28332, .F. ) ;
#17664 = DIRECTION ( 'NONE',  ( -1.000000000000000000, -0.000000000000000000, -0.000000000000000000 ) ) ;
#17665 = AXIS2_PLACEMENT_3D ( 'NONE', #35756, #8790, #32131 ) ;
#17666 = EDGE_CURVE ( 'NONE', #19994, #19154, #45480, .T. ) ;
#17667 = VERTEX_POINT ( 'NONE', #49272 ) ;
#17668 = CARTESIAN_POINT ( 'NONE',  ( -7.372990760266265653, 0.000000000000000000, 0.000000000000000000 ) ) ;
#17669 = DIRECTION ( 'NONE',  ( -1.000000000000000000, -0.000000000000000000, -0.000000000000000000 ) ) ;
#17670 = VECTOR ( 'NONE', #11128, 1000.000000000000000 ) ;
#17671 = ORIENTED_EDGE ( 'NONE', *, *, #5485, .T. ) ;
#17672 = CARTESIAN_POINT ( 'NONE',  ( 357.9999999999998863, 182.1715728752540429, -357.1715728752541850 ) ) ;
#17673 = EDGE_CURVE ( 'NONE', #25022, #19653, #11076, .T. ) ;
#17674 = CARTESIAN_POINT ( 'NONE',  ( -4.945973446814903696, 2.143131898507912917E-16, -77.43171244307198720 ) ) ;
#17675 = VECTOR ( 'NONE', #23190, 1000.000000000000000 ) ;
#17676 = DIRECTION ( 'NONE',  ( 0.000000000000000000, -1.000000000000000000, 0.000000000000000000 ) ) ;
#17677 = VERTEX_POINT ( 'NONE', #38305 ) ;
#17678 = EDGE_CURVE ( 'NONE', #43135, #13514, #6976, .T. ) ;
#17679 = CARTESIAN_POINT ( 'NONE',  ( 0.000000000000000000, 17.00000000000000000, 0.000000000000000000 ) ) ;
#17680 = EDGE_CURVE ( 'NONE', #50107, #39980, #33813, .T. ) ;
#17681 = VECTOR ( 'NONE', #8166, 1000.000000000000000 ) ;
#17682 = VERTEX_POINT ( 'NONE', #14928 ) ;
#17683 = PLANE ( 'NONE',  #6253 ) ;
#17684 = FACE_OUTER_BOUND ( 'NONE', #30910, .T. ) ;
#17685 = ORIENTED_EDGE ( 'NONE', *, *, #43099, .F. ) ;
#17686 =( GEOMETRIC_REPRESENTATION_CONTEXT ( 3 ) GLOBAL_UNCERTAINTY_ASSIGNED_CONTEXT ( ( #48143 ) ) GLOBAL_UNIT_ASSIGNED_CONTEXT ( ( #34954, #10557, #38791 ) ) REPRESENTATION_CONTEXT ( 'NONE', 'WORKASPACE' ) );
#17687 = ORIENTED_EDGE ( 'NONE', *, *, #49405, .F. ) ;
#17688 = ORIENTED_EDGE ( 'NONE', *, *, #48355, .T. ) ;
#17689 = CARTESIAN_POINT ( 'NONE',  ( 339.9999999999998863, -182.9999999999999716, 343.9999999999997726 ) ) ;
#17690 = DIRECTION ( 'NONE',  ( -1.000000000000000000, -0.000000000000000000, -0.000000000000000000 ) ) ;
#17691 = ORIENTED_EDGE ( 'NONE', *, *, #50399, .F. ) ;
#17692 = AXIS2_PLACEMENT_3D ( 'NONE', #21234, #1744, #45569 ) ;
#17693 = VECTOR ( 'NONE', #46846, 1000.000000000000000 ) ;
#17694 = CARTESIAN_POINT ( 'NONE',  ( 210.0000000000000568, 0.000000000000000000, 82.56828755692799859 ) ) ;
#17695 = FACE_OUTER_BOUND ( 'NONE', #2571, .T. ) ;
#17696 = CYLINDRICAL_SURFACE ( 'NONE', #32559, 1.750000000000015543 ) ;
#17697 = ORIENTED_EDGE ( 'NONE', *, *, #18897, .T. ) ;
#17698 = DIRECTION ( 'NONE',  ( -0.000000000000000000, -0.000000000000000000, 1.000000000000000000 ) ) ;
#17699 = CARTESIAN_POINT ( 'NONE',  ( -0.8433491450857070193, 0.9182416014173486740, 9.981352469109932457 ) ) ;
#17700 = CARTESIAN_POINT ( 'NONE',  ( -32.43949840348904701, -7.871562655726274116, -9.367992836599954742 ) ) ;
#17701 = EDGE_CURVE ( 'NONE', #31600, #28309, #41622, .T. ) ;
#17702 = EDGE_CURVE ( 'NONE', #156, #3329, #2608, .T. ) ;
#17703 = ORIENTED_EDGE ( 'NONE', *, *, #15288, .F. ) ;
#17704 = CYLINDRICAL_SURFACE ( 'NONE', #50233, 5.000000000000000000 ) ;
#17705 = CARTESIAN_POINT ( 'NONE',  ( 21.58778298521313843, -25.34222074689757065, 3.199614146704519602 ) ) ;
#17706 = EDGE_CURVE ( 'NONE', #29488, #11677, #18762, .T. ) ;
#17707 = EDGE_CURVE ( 'NONE', #18077, #5399, #44265, .T. ) ;
#17708 = CIRCLE ( 'NONE', #12801, 2.000000000000001776 ) ;
#17710 = AXIS2_PLACEMENT_3D ( 'NONE', #37529, #20843, #21593 ) ;
#17709 = CARTESIAN_POINT ( 'NONE',  ( -15.00099850811941948, -7.462898891544107016, 9.403735324607438884 ) ) ;
#17711 = CARTESIAN_POINT ( 'NONE',  ( 342.8284271247462129, 183.0000000000000853, 357.9999999999998295 ) ) ;
#17712 = ORIENTED_EDGE ( 'NONE', *, *, #27489, .F. ) ;
#17713 = EDGE_CURVE ( 'NONE', #3850, #28373, #29953, .T. ) ;
#17714 = CARTESIAN_POINT ( 'NONE',  ( 112.2789002873379758, 1.749999999999997113, -80.20683870891909351 ) ) ;
#17715 = CARTESIAN_POINT ( 'NONE',  ( -164.9999999999987779, 17.00000000000000000, 5.000000000000004441 ) ) ;
#17716 = ADVANCED_FACE ( 'NONE', ( #49013 ), #50167, .T. ) ;
#17717 = CARTESIAN_POINT ( 'NONE',  ( -42.99990394833793061, 47.95759300784327905, 5.000000000000000000 ) ) ;
#17718 = FACE_OUTER_BOUND ( 'NONE', #6709, .T. ) ;
#17719 = DIRECTION ( 'NONE',  ( 1.000000000000000000, 0.000000000000000000, 0.000000000000000000 ) ) ;
#17720 = VECTOR ( 'NONE', #6575, 1000.000000000000000 ) ;
#17721 = ORIENTED_EDGE ( 'NONE', *, *, #4825, .F. ) ;
#17722 = DIRECTION ( 'NONE',  ( -0.000000000000000000, -0.000000000000000000, -1.000000000000000000 ) ) ;
#17723 = ORIENTED_EDGE ( 'NONE', *, *, #27586, .F. ) ;
#17724 = DIRECTION ( 'NONE',  ( -0.000000000000000000, 1.000000000000000000, 0.000000000000000000 ) ) ;
#17725 = VECTOR ( 'NONE', #12781, 1000.000000000000000 ) ;
#17726 = VERTEX_POINT ( 'NONE', #38042 ) ;
#17727 = LINE ( 'NONE', #30286, #45861 ) ;
#17728 = DIRECTION ( 'NONE',  ( -1.000000000000000000, -0.000000000000000000, -0.000000000000000000 ) ) ;
#17729 = LINE ( 'NONE', #10283, #44511 ) ;
#17730 = ADVANCED_FACE ( 'NONE', ( #18515 ), #49770, .F. ) ;
#17731 = VERTEX_POINT ( 'NONE', #46945 ) ;
#17732 = VECTOR ( 'NONE', #23926, 1000.000000000000000 ) ;
#17733 = EDGE_CURVE ( 'NONE', #25169, #16336, #23, .T. ) ;
#17734 = CARTESIAN_POINT ( 'NONE',  ( -119.9999999999990905, 17.00000000000000000, -24.99999999999999289 ) ) ;
#17735 = ADVANCED_FACE ( 'NONE', ( #38798 ), #23895, .T. ) ;
#17736 = VERTEX_POINT ( 'NONE', #7232 ) ;
#17737 = CARTESIAN_POINT ( 'NONE',  ( -6.880036658038867436, 222.4999999999999716, -228.6347188485896140 ) ) ;
#17738 = CARTESIAN_POINT ( 'NONE',  ( 181.0000000000000000, -9.999999999999953815, 339.9999999999998295 ) ) ;
#17739 = LINE ( 'NONE', #33405, #40 ) ;
#17740 = CARTESIAN_POINT ( 'NONE',  ( 164.9999999999999716, 16.00000000000000000, 60.00000000000000000 ) ) ;
#17741 = CARTESIAN_POINT ( 'NONE',  ( 48.33712804702526000, 13.03701565032775456, -9.367992836599954742 ) ) ;
#17742 = ORIENTED_EDGE ( 'NONE', *, *, #17354, .T. ) ;
#17743 = ORIENTED_EDGE ( 'NONE', *, *, #14632, .F. ) ;
#17744 = DIRECTION ( 'NONE',  ( 1.000000000000000000, 0.000000000000000000, 0.000000000000000000 ) ) ;
#17745 = VERTEX_POINT ( 'NONE', #19786 ) ;
#17746 = AXIS2_PLACEMENT_3D ( 'NONE', #42293, #38468, #6384 ) ;
#17747 = CARTESIAN_POINT ( 'NONE',  ( 115.0540265531850395, 2.143131898507847836E-16, 82.56828755692797017 ) ) ;
#17748 = CARTESIAN_POINT ( 'NONE',  ( 0.000000000000000000, 23.48684210526316107, 0.000000000000000000 ) ) ;
#17749 = CIRCLE ( 'NONE', #33322, 2.000000000000001776 ) ;
#17750 = ORIENTED_EDGE ( 'NONE', *, *, #17069, .F. ) ;
#17751 = CARTESIAN_POINT ( 'NONE',  ( -0.9983599181300891745, -1.124146016603549070, 9.953784399990620813 ) ) ;
#17752 = EDGE_CURVE ( 'NONE', #50186, #31279, #5452, .T. ) ;
#17753 = FACE_OUTER_BOUND ( 'NONE', #12262, .T. ) ;
#17754 = ORIENTED_EDGE ( 'NONE', *, *, #20381, .T. ) ;
#17755 = CARTESIAN_POINT ( 'NONE',  ( 1.193089574352119264, 0.2545860991493882342, 9.963925895596188909 ) ) ;
#17756 = CARTESIAN_POINT ( 'NONE',  ( -30.21887974406478250, 14.69854701517550666, -8.016098858316199838 ) ) ;
#17757 = CARTESIAN_POINT ( 'NONE',  ( 33.30402655318503946, -1.750000000000009992, 0.8182875569279768335 ) ) ;
#17758 = CARTESIAN_POINT ( 'NONE',  ( -1.211050186583223720, -0.5544523570010669866, 9.951893257060014264 ) ) ;
#17759 = ORIENTED_EDGE ( 'NONE', *, *, #36924, .F. ) ;
#17760 = ORIENTED_EDGE ( 'NONE', *, *, #39498, .F. ) ;
#17761 = EDGE_CURVE ( 'NONE', #11655, #37697, #20126, .T. ) ;
#17762 = CARTESIAN_POINT ( 'NONE',  ( -1.320835335343009787, 0.01943189458965158267, 9.943883492372876276 ) ) ;
#17763 = DIRECTION ( 'NONE',  ( 0.000000000000000000, 0.3790464617558786942, -0.9253776417389547593 ) ) ;
#17764 = CARTESIAN_POINT ( 'NONE',  ( -128.4459734468149463, -1.025126265847081442, -0.9317124430720195027 ) ) ;
#17765 = CARTESIAN_POINT ( 'NONE',  ( -44.94597344681493922, 1.025126265847089657, -80.93171244307201562 ) ) ;
#17766 = VERTEX_POINT ( 'NONE', #20044 ) ;
#17767 = AXIS2_PLACEMENT_3D ( 'NONE', #21918, #41410, #42403 ) ;
#17768 = ORIENTED_EDGE ( 'NONE', *, *, #16629, .T. ) ;
#17769 = LINE ( 'NONE', #2368, #753 ) ;
#17770 = DIRECTION ( 'NONE',  ( 0.000000000000000000, 0.000000000000000000, -1.000000000000000000 ) ) ;
#17771 = CARTESIAN_POINT ( 'NONE',  ( 113.3040265531850537, 1.749999999999997335, 80.81828755692798438 ) ) ;
#17772 = EDGE_CURVE ( 'NONE', #47173, #31887, #49489, .T. ) ;
#17773 = ADVANCED_FACE ( 'NONE', ( #26980 ), #31615, .F. ) ;
#17774 = PLANE ( 'NONE',  #19285 ) ;
#17775 = DIRECTION ( 'NONE',  ( 1.000000000000000000, 0.000000000000000000, -0.000000000000000000 ) ) ;
#17776 = VERTEX_POINT ( 'NONE', #19271 ) ;
#17777 = CARTESIAN_POINT ( 'NONE',  ( -6.880036658038818587, -197.4999999999999432, -228.6347188485896140 ) ) ;
#17778 = EDGE_CURVE ( 'NONE', #12842, #40787, #3974, .T. ) ;
#17779 = DIRECTION ( 'NONE',  ( -1.000000000000000000, 0.000000000000000000, 0.000000000000000000 ) ) ;
#17780 = DIRECTION ( 'NONE',  ( 0.000000000000000000, -1.000000000000000000, -3.186989995019654210E-49 ) ) ;
#17781 = ADVANCED_FACE ( 'NONE', ( #42618 ), #35209, .T. ) ;
#17782 = EDGE_CURVE ( 'NONE', #43683, #10540, #3367, .T. ) ;
#17783 = DIRECTION ( 'NONE',  ( -2.775557561562891844E-16, 0.7071067811865473507, -0.7071067811865477948 ) ) ;
#17784 = ORIENTED_EDGE ( 'NONE', *, *, #29412, .T. ) ;
#17785 = CARTESIAN_POINT ( 'NONE',  ( -17.43089236541806031, -28.36237856644526900, 3.199614146704519602 ) ) ;
#17786 = ORIENTED_EDGE ( 'NONE', *, *, #26806, .T. ) ;
#17787 = CARTESIAN_POINT ( 'NONE',  ( 71.55402655318505367, -1.025126265847089879, -77.43171244307200141 ) ) ;
#17788 = CARTESIAN_POINT ( 'NONE',  ( 1.011271242968688311, -0.7347315653655855927, 10.00000000000000000 ) ) ;
#17789 = ADVANCED_FACE ( 'NONE', ( #50276 ), #3881, .F. ) ;
#17790 =( BOUNDED_CURVE ( )  B_SPLINE_CURVE ( 3, ( #27138, #31500, #6872, #50682 ),
 .UNSPECIFIED., .F., .F. ) 
 B_SPLINE_CURVE_WITH_KNOTS ( ( 4, 4 ),
 ( 3.141592653589793116, 4.712388980384689674 ),
 .UNSPECIFIED. ) 
 CURVE ( )  GEOMETRIC_REPRESENTATION_ITEM ( )  RATIONAL_B_SPLINE_CURVE ( ( 1.000000000000000000, 0.8047378541243649375, 0.8047378541243649375, 1.000000000000000000 ) ) 
 REPRESENTATION_ITEM ( '' )  );
#17791 = CARTESIAN_POINT ( 'NONE',  ( 25.63461350838963071, -43.17876197216377676, -8.016098858316205167 ) ) ;
#17792 = B_SPLINE_CURVE_WITH_KNOTS ( 'NONE', 3,
 ( #29892, #25286, #37866, #45005 ),
 .UNSPECIFIED., .F., .F.,
 ( 4, 4 ),
 ( 9.129125108812345642E-16, 0.0004154657329515903247 ),
 .UNSPECIFIED. ) ;
#17793 = CARTESIAN_POINT ( 'NONE',  ( 35.00000000000122213, 17.00000000000000000, 5.000000000000004441 ) ) ;
#17794 = ORIENTED_EDGE ( 'NONE', *, *, #40659, .F. ) ;
#17795 = DIRECTION ( 'NONE',  ( -0.9928768384869219865, 0.000000000000000000, -0.1191452206184307888 ) ) ;
#17796 = CARTESIAN_POINT ( 'NONE',  ( 10.00000000000000000, 1.224646799147353256E-15, 10.00000000000000000 ) ) ;
#17797 = ORIENTED_EDGE ( 'NONE', *, *, #6467, .F. ) ;
#17798 = EDGE_LOOP ( 'NONE', ( #11289, #49239 ) ) ;
#17799 = CARTESIAN_POINT ( 'NONE',  ( -0.8282505383454070724, -1.889063466747028297, 9.894754715216727448 ) ) ;
#17800 = CARTESIAN_POINT ( 'NONE',  ( 0.000000000000000000, 0.000000000000000000, 0.000000000000000000 ) ) ;
#17801 = VERTEX_POINT ( 'NONE', #23126 ) ;
#17802 = ORIENTED_EDGE ( 'NONE', *, *, #25959, .T. ) ;
#17803 = CYLINDRICAL_SURFACE ( 'NONE', #26409, 1.750000000000015543 ) ;
#17804 = CARTESIAN_POINT ( 'NONE',  ( -0.2778388845795317086, 1.251314014313103851, 9.976582533991678048 ) ) ;
#17805 = LINE ( 'NONE', #45474, #49625 ) ;
#17806 = CARTESIAN_POINT ( 'NONE',  ( -0.6215990105957072132, 1.608617984725374983, 9.928159647716134018 ) ) ;
#17807 = ORIENTED_EDGE ( 'NONE', *, *, #16002, .T. ) ;
#17808 = EDGE_LOOP ( 'NONE', ( #46218, #13579, #664, #50489 ) ) ;
#17809 = CARTESIAN_POINT ( 'NONE',  ( 0.000000000000000000, 17.00000000000000000, 0.000000000000000000 ) ) ;
#17810 = CARTESIAN_POINT ( 'NONE',  ( 356.0000000000001137, 183.0000000000000284, 349.9999999999998295 ) ) ;
#17811 = VERTEX_POINT ( 'NONE', #15950 ) ;
#17812 = VERTEX_POINT ( 'NONE', #47202 ) ;
#17813 = DIRECTION ( 'NONE',  ( 0.000000000000000000, -1.000000000000000000, 0.000000000000000000 ) ) ;
#17814 = CARTESIAN_POINT ( 'NONE',  ( -165.0000000000000284, 16.00000000000000000, 115.0000000000000142 ) ) ;
#17815 = ORIENTED_EDGE ( 'NONE', *, *, #281, .F. ) ;
#17816 = VERTEX_POINT ( 'NONE', #3626 ) ;
#17817 = CARTESIAN_POINT ( 'NONE',  ( -165.3973046169136012, -98.56198943095992604, -17.65743994998275213 ) ) ;
#17818 = CARTESIAN_POINT ( 'NONE',  ( -30.43621780902774532, 14.03210827430580210, -8.466730184410787174 ) ) ;
#17819 = ORIENTED_EDGE ( 'NONE', *, *, #4856, .F. ) ;
#17820 = DIRECTION ( 'NONE',  ( 0.000000000000000000, -1.000000000000000000, 1.544785076050074834E-48 ) ) ;
#17821 = CARTESIAN_POINT ( 'NONE',  ( 0.000000000000000000, 181.0000000000000284, 339.9999999999997726 ) ) ;
#17822 = CARTESIAN_POINT ( 'NONE',  ( -165.3973046169136012, 103.9380105690400597, 22.84256005001721945 ) ) ;
#17823 = CARTESIAN_POINT ( 'NONE',  ( -86.69597344681494633, -1.750000000000010658, -79.18171244307201562 ) ) ;
#17824 = EDGE_CURVE ( 'NONE', #23499, #3216, #19520, .T. ) ;
#17825 = EDGE_CURVE ( 'NONE', #38528, #32226, #43139, .T. ) ;
#17826 = CARTESIAN_POINT ( 'NONE',  ( -10.49999999999999467, -46.51315789473685669, 6.315789473684212396 ) ) ;
#17827 = ORIENTED_EDGE ( 'NONE', *, *, #34684, .F. ) ;
#17828 = CARTESIAN_POINT ( 'NONE',  ( -206.6959734468149463, -1.750000000000010658, -79.18171244307201562 ) ) ;
#17829 = CARTESIAN_POINT ( 'NONE',  ( 71.55402655318505367, 0.000000000000000000, -40.93171244307205825 ) ) ;
#17830 = EDGE_CURVE ( 'NONE', #43927, #11996, #50108, .T. ) ;
#17831 = CARTESIAN_POINT ( 'NONE',  ( -8.277096487746778308, 50.00000000000000000, 7.455576670931136185 ) ) ;
#17832 = FACE_OUTER_BOUND ( 'NONE', #46282, .T. ) ;
#17833 = ADVANCED_FACE ( 'NONE', ( #4145 ), #12846, .T. ) ;
#17834 = EDGE_CURVE ( 'NONE', #16395, #16392, #9222, .T. ) ;
#17835 = CARTESIAN_POINT ( 'NONE',  ( -215.0000000000000568, -172.9999999999999716, 252.0000000000000000 ) ) ;
#17836 = CARTESIAN_POINT ( 'NONE',  ( 35.00000000000061107, 16.00000000000000000, -54.99999999999999289 ) ) ;
#17837 = ADVANCED_FACE ( 'NONE', ( #1559, #16452 ), #40806, .F. ) ;
#17838 = CARTESIAN_POINT ( 'NONE',  ( 6.174150299305392053, -33.14591993373988998, 8.807470649214879543 ) ) ;
#17839 = DIRECTION ( 'NONE',  ( -0.000000000000000000, -0.000000000000000000, -1.000000000000000000 ) ) ;
#17840 = EDGE_CURVE ( 'NONE', #34478, #8464, #32359, .T. ) ;
#17841 = DIRECTION ( 'NONE',  ( 1.000000000000000000, 0.000000000000000000, 0.000000000000000000 ) ) ;
#17842 = ORIENTED_EDGE ( 'NONE', *, *, #28204, .T. ) ;
#17843 = PLANE ( 'NONE',  #9275 ) ;
#17844 = LINE ( 'NONE', #33270, #2459 ) ;
#17845 = CARTESIAN_POINT ( 'NONE',  ( 153.3040265531850537, -1.750000000000010214, 40.81828755692798438 ) ) ;
#17846 = CARTESIAN_POINT ( 'NONE',  ( -124.9459734468149321, -1.025126265847081664, 42.56828755692797017 ) ) ;
#17847 = DIRECTION ( 'NONE',  ( -0.9908916497796512735, 0.000000000000000000, -0.1346615698592613652 ) ) ;
#17848 = EDGE_LOOP ( 'NONE', ( #20087, #16351, #7662, #28529 ) ) ;
#17849 = ORIENTED_EDGE ( 'NONE', *, *, #246, .F. ) ;
#17850 = DIRECTION ( 'NONE',  ( -0.000000000000000000, -1.000000000000000000, -0.000000000000000000 ) ) ;
#17851 = CARTESIAN_POINT ( 'NONE',  ( -46.69597344681494633, 1.750000000000009992, 0.8182875569279768335 ) ) ;
#17852 = ORIENTED_EDGE ( 'NONE', *, *, #3841, .F. ) ;
#17853 = CARTESIAN_POINT ( 'NONE',  ( -34.95136153415531766, 36.40974830873496870, 8.356839323120299312 ) ) ;
#17854 = CARTESIAN_POINT ( 'NONE',  ( 341.9999999999999432, 181.0000000000000568, -356.0000000000002274 ) ) ;
#17855 =( BOUNDED_CURVE ( )  B_SPLINE_CURVE ( 3, ( #37889, #30686, #45780, #6566 ),
 .UNSPECIFIED., .F., .F. ) 
 B_SPLINE_CURVE_WITH_KNOTS ( ( 4, 4 ),
 ( 3.141592653589793116, 4.712388980384689674 ),
 .UNSPECIFIED. ) 
 CURVE ( )  GEOMETRIC_REPRESENTATION_ITEM ( )  RATIONAL_B_SPLINE_CURVE ( ( 1.000000000000000000, 0.8047378541243649375, 0.8047378541243649375, 1.000000000000000000 ) ) 
 REPRESENTATION_ITEM ( '' )  );
#17856 = ORIENTED_EDGE ( 'NONE', *, *, #32773, .T. ) ;
#17857 = ORIENTED_EDGE ( 'NONE', *, *, #27143, .T. ) ;
#17858 = EDGE_CURVE ( 'NONE', #20963, #12440, #32102, .T. ) ;
#17859 = ORIENTED_EDGE ( 'NONE', *, *, #33389, .F. ) ;
#17860 = EDGE_CURVE ( 'NONE', #27491, #6443, #13343, .T. ) ;
#17861 = DIRECTION ( 'NONE',  ( -1.000000000000000000, -0.000000000000000000, -0.000000000000000000 ) ) ;
#17862 = CARTESIAN_POINT ( 'NONE',  ( 12.78770032058947237, 31.68259716188277864, 7.455576670931136185 ) ) ;
#17863 = ORIENTED_EDGE ( 'NONE', *, *, #14051, .F. ) ;
#17864 = DIRECTION ( 'NONE',  ( 1.132880637372608740E-16, 4.718402560806925739E-50, 1.000000000000000000 ) ) ;
#17865 = ORIENTED_EDGE ( 'NONE', *, *, #21387, .T. ) ;
#17866 = EDGE_LOOP ( 'NONE', ( #11328, #24462, #21106, #9643 ) ) ;
#17867 = DIRECTION ( 'NONE',  ( -0.000000000000000000, -0.000000000000000000, -1.000000000000000000 ) ) ;
#17868 = LINE ( 'NONE', #49637, #43926 ) ;
#17869 = CARTESIAN_POINT ( 'NONE',  ( -204.9459734468148895, 1.025126265847089213, -160.9317124430720014 ) ) ;
#17870 = VERTEX_POINT ( 'NONE', #13600 ) ;
#17871 = DIRECTION ( 'NONE',  ( 0.000000000000000000, 0.000000000000000000, 1.000000000000000000 ) ) ;
#17872 = CARTESIAN_POINT ( 'NONE',  ( -208.4459734468148611, -1.025126265847089435, 39.06828755692797728 ) ) ;
#17873 = FACE_OUTER_BOUND ( 'NONE', #1168, .T. ) ;
#17874 = CARTESIAN_POINT ( 'NONE',  ( -0.8155877869437639927, -0.9072449372115535260, 9.963925895596188909 ) ) ;
#17875 = AXIS2_PLACEMENT_3D ( 'NONE', #48516, #18005, #40624 ) ;
#17876 = CARTESIAN_POINT ( 'NONE',  ( 2.538055338523173443, 50.00000000000000000, -9.367992836599951190 ) ) ;
#17877 = CARTESIAN_POINT ( 'NONE',  ( 0.000000000000000000, 17.00000000000000000, 0.000000000000000000 ) ) ;
#17878 = CARTESIAN_POINT ( 'NONE',  ( 115.0540265531850395, 2.143131898507847836E-16, 2.568287556927950632 ) ) ;
#17879 = CARTESIAN_POINT ( 'NONE',  ( 0.9460392030551082465, 0.7922402054952416561, 9.969907203203607793 ) ) ;
#17880 = CYLINDRICAL_SURFACE ( 'NONE', #28519, 3.500000000000003109 ) ;
#17881 = CARTESIAN_POINT ( 'NONE',  ( 113.3040265531850537, 1.749999999999996891, -159.1817124430720298 ) ) ;
#17882 = CARTESIAN_POINT ( 'NONE',  ( 191.5540265531850537, -1.025126265847089213, 159.0682875569279418 ) ) ;
#17883 = ORIENTED_EDGE ( 'NONE', *, *, #38628, .F. ) ;
#17884 = ADVANCED_FACE ( 'NONE', ( #29001 ), #44621, .F. ) ;
#17885 = FACE_OUTER_BOUND ( 'NONE', #42745, .T. ) ;
#17886 = CARTESIAN_POINT ( 'NONE',  ( -14.76429217231967428, -8.192625680377590314, 9.178419661560148768 ) ) ;
#17887 = CARTESIAN_POINT ( 'NONE',  ( 0.2774838294623813151, -1.251476322270253405, 9.957892297621013356 ) ) ;
#17888 = B_SPLINE_CURVE_WITH_KNOTS ( 'NONE', 3,
 ( #25470, #48265, #29566, #21109 ),
 .UNSPECIFIED., .F., .F.,
 ( 4, 4 ),
 ( 0.0004299334430849316652, 0.0007706806524479852200 ),
 .UNSPECIFIED. ) ;
#17889 = ORIENTED_EDGE ( 'NONE', *, *, #35477, .F. ) ;
#17890 = LINE ( 'NONE', #1759, #19921 ) ;
#17891 = FACE_OUTER_BOUND ( 'NONE', #36780, .T. ) ;
#17892 = ORIENTED_EDGE ( 'NONE', *, *, #440, .F. ) ;
#17893 = CARTESIAN_POINT ( 'NONE',  ( 183.0000000000000000, -5.999999999999950262, -340.0000000000001137 ) ) ;
#17894 = CARTESIAN_POINT ( 'NONE',  ( -164.9459734468149463, 1.025126265847089657, 79.06828755692797017 ) ) ;
#17895 = DIRECTION ( 'NONE',  ( -1.000000000000000000, -0.000000000000000000, -0.000000000000000000 ) ) ;
#17896 = FACE_OUTER_BOUND ( 'NONE', #37498, .T. ) ;
#17897 = ORIENTED_EDGE ( 'NONE', *, *, #30250, .T. ) ;
#17898 = ORIENTED_EDGE ( 'NONE', *, *, #431, .T. ) ;
#17899 = ORIENTED_EDGE ( 'NONE', *, *, #50388, .F. ) ;
#17900 = CARTESIAN_POINT ( 'NONE',  ( 210.0000000000000568, 0.000000000000000000, 80.81828755692798438 ) ) ;
#17901 =( BOUNDED_CURVE ( )  B_SPLINE_CURVE ( 3, ( #32366, #1324, #33137, #5909 ),
 .UNSPECIFIED., .F., .F. ) 
 B_SPLINE_CURVE_WITH_KNOTS ( ( 4, 4 ),
 ( 4.712388980384689674, 6.283185307179586232 ),
 .UNSPECIFIED. ) 
 CURVE ( )  GEOMETRIC_REPRESENTATION_ITEM ( )  RATIONAL_B_SPLINE_CURVE ( ( 1.000000000000000000, 0.8047378541243649375, 0.8047378541243649375, 1.000000000000000000 ) ) 
 REPRESENTATION_ITEM ( '' )  );
#17902 = AXIS2_PLACEMENT_3D ( 'NONE', #36869, #48081, #32239 ) ;
#17903 = ORIENTED_EDGE ( 'NONE', *, *, #23288, .F. ) ;
#17904 = DIRECTION ( 'NONE',  ( -1.000000000000000000, 0.000000000000000000, 0.000000000000000000 ) ) ;
#17905 = CARTESIAN_POINT ( 'NONE',  ( 129.9999999999999432, 17.00000000000000000, -114.9999999999999858 ) ) ;
#17906 = VERTEX_POINT ( 'NONE', #806 ) ;
#17907 = PLANE ( 'NONE',  #1573 ) ;
#17908 = CARTESIAN_POINT ( 'NONE',  ( -165.6708471809677974, 1.750000000000010214, 81.84341382277507648 ) ) ;
#17909 =( BOUNDED_CURVE ( )  B_SPLINE_CURVE ( 3, ( #7448, #30531, #18966, #6665 ),
 .UNSPECIFIED., .F., .F. ) 
 B_SPLINE_CURVE_WITH_KNOTS ( ( 4, 4 ),
 ( 3.141592653589793116, 4.712388980384689674 ),
 .UNSPECIFIED. ) 
 CURVE ( )  GEOMETRIC_REPRESENTATION_ITEM ( )  RATIONAL_B_SPLINE_CURVE ( ( 1.000000000000000000, 0.8047378541243649375, 0.8047378541243649375, 1.000000000000000000 ) ) 
 REPRESENTATION_ITEM ( '' )  );
#17910 = CARTESIAN_POINT ( 'NONE',  ( 169.0000000000000284, 165.0000000000000000, 343.9999999999998863 ) ) ;
#17911 = VERTEX_POINT ( 'NONE', #4886 ) ;
#17913 = EDGE_CURVE ( 'NONE', #42445, #27283, #24909, .T. ) ;
#17912 = DIRECTION ( 'NONE',  ( 0.000000000000000000, 0.000000000000000000, -1.000000000000000000 ) ) ;
#17914 = CARTESIAN_POINT ( 'NONE',  ( 194.9999999999999432, -172.9999999999999716, 252.0000000000000568 ) ) ;
#17915 = CARTESIAN_POINT ( 'NONE',  ( 210.0000000000000568, 2.143131898507880377E-16, -160.9317124430720298 ) ) ;
#17916 = ORIENTED_EDGE ( 'NONE', *, *, #5845, .T. ) ;
#17917 = CARTESIAN_POINT ( 'NONE',  ( 111.5540265531850537, 1.025126265847081442, -160.9317124430720014 ) ) ;
#17918 = DIRECTION ( 'NONE',  ( -0.000000000000000000, 1.000000000000000000, 6.123233995736766036E-17 ) ) ;
#17919 = EDGE_LOOP ( 'NONE', ( #16456, #46429, #31431, #1419, #5362, #12831 ) ) ;
#17920 = ORIENTED_EDGE ( 'NONE', *, *, #35426, .F. ) ;
#17921 = ORIENTED_EDGE ( 'NONE', *, *, #33068, .F. ) ;
#17922 = LINE ( 'NONE', #22292, #41001 ) ;
#17923 = DIRECTION ( 'NONE',  ( 1.000000000000000000, 0.000000000000000000, 0.000000000000000000 ) ) ;
#17924 = B_SPLINE_SURFACE_WITH_KNOTS ( 'NONE', 3, 3, ( 
 ( #49207, #6154, #21545, #36983 ),
 ( #1805, #33121, #2056, #25662 ),
 ( #21806, #44868, #9740, #25405 ),
 ( #41053, #17700, #33370, #37479 ) ),
 .UNSPECIFIED., .F., .F., .F.,
 ( 4, 4 ),
 ( 4, 4 ),
 ( 0.000000000000000000, 1.000000000000000000 ),
 ( 0.000000000000000000, 1.000000000000000000 ),
 .UNSPECIFIED. ) ;
#17925 = EDGE_LOOP ( 'NONE', ( #49517, #279, #22847, #12680, #6972, #47225 ) ) ;
#17926 = DIRECTION ( 'NONE',  ( -1.000000000000000000, -0.000000000000000000, -0.000000000000000000 ) ) ;
#17927 = DIRECTION ( 'NONE',  ( -1.000000000000000000, 0.000000000000000000, 0.000000000000000000 ) ) ;
#17928 = CARTESIAN_POINT ( 'NONE',  ( 168.9999999999999716, -184.9999999999999716, -350.0000000000001705 ) ) ;
#17929 = CARTESIAN_POINT ( 'NONE',  ( -84.94597344681494633, 2.143131898507880377E-16, 165.0000000000000000 ) ) ;
#17930 = VERTEX_POINT ( 'NONE', #21052 ) ;
#17931 = LINE ( 'NONE', #48941, #26125 ) ;
#17932 = CARTESIAN_POINT ( 'NONE',  ( -87.72109971266203843, 1.750000000000010436, -80.20683870891910772 ) ) ;
#17933 = CARTESIAN_POINT ( 'NONE',  ( 0.000000000000000000, 17.00000000000000000, 0.000000000000000000 ) ) ;
#17934 = ORIENTED_EDGE ( 'NONE', *, *, #36206, .T. ) ;
#17935 = AXIS2_PLACEMENT_3D ( 'NONE', #1944, #37618, #48589 ) ;
#17936 = DIRECTION ( 'NONE',  ( -1.000000000000000000, 0.000000000000000000, -1.612977847700450206E-50 ) ) ;
#17937 = LINE ( 'NONE', #45874, #16883 ) ;
#17938 = CARTESIAN_POINT ( 'NONE',  ( -29.39982726364978660, -16.78152490921149109, 8.356839323120299312 ) ) ;
#17939 = CARTESIAN_POINT ( 'NONE',  ( -16.52264463346130796, 2.779753662172870232, 9.403735324607438884 ) ) ;
#17940 = ORIENTED_EDGE ( 'NONE', *, *, #25212, .T. ) ;
#17941 = VECTOR ( 'NONE', #32167, 999.9999999999998863 ) ;
#17942 = AXIS2_PLACEMENT_3D ( 'NONE', #41281, #28736, #33105 ) ;
#17943 = DIRECTION ( 'NONE',  ( -0.000000000000000000, -0.000000000000000000, -1.000000000000000000 ) ) ;
#17944 = ADVANCED_FACE ( 'NONE', ( #40555 ), #20294, .T. ) ;
#17945 = AXIS2_PLACEMENT_3D ( 'NONE', #49409, #6352, #18394 ) ;
#17946 = CARTESIAN_POINT ( 'NONE',  ( 13.35436367797824353, 31.26996044524050333, 7.906207997025717304 ) ) ;
#17947 = CARTESIAN_POINT ( 'NONE',  ( -0.3862712429686809279, -1.188820645368943163, 10.00000000000000000 ) ) ;
#17948 = CARTESIAN_POINT ( 'NONE',  ( -6.174150299305392053, 33.14591993373988998, 8.807470649214879543 ) ) ;
#17949 = ADVANCED_FACE ( 'NONE', ( #9005 ), #24659, .T. ) ;
#17950 = CARTESIAN_POINT ( 'NONE',  ( 71.55402655318505367, 0.000000000000000000, 2.568287556928006143 ) ) ;
#17951 = EDGE_CURVE ( 'NONE', #46080, #45423, #33125, .T. ) ;
#17952 = VECTOR ( 'NONE', #34975, 1000.000000000000000 ) ;
#17953 = VERTEX_POINT ( 'NONE', #47698 ) ;
#17954 = CARTESIAN_POINT ( 'NONE',  ( 210.0000000000000568, 2.143131898507880377E-16, 159.0682875569279702 ) ) ;
#17955 = ORIENTED_EDGE ( 'NONE', *, *, #13987, .T. ) ;
#17956 = CARTESIAN_POINT ( 'NONE',  ( -8.277096487746778308, 50.00000000000000711, 7.455576670931136185 ) ) ;
#17957 = ORIENTED_EDGE ( 'NONE', *, *, #49935, .F. ) ;
#17958 = DIRECTION ( 'NONE',  ( -0.000000000000000000, 0.9749645535258960605, -0.2223603367690608623 ) ) ;
#17960 = EDGE_CURVE ( 'NONE', #38152, #42864, #38176, .T. ) ;
#17959 = FACE_OUTER_BOUND ( 'NONE', #18317, .T. ) ;
#17961 = EDGE_CURVE ( 'NONE', #7778, #9118, #39987, .T. ) ;
#17962 =( NAMED_UNIT ( * ) PLANE_ANGLE_UNIT ( ) SI_UNIT ( $, .RADIAN. ) );
#17963 = ORIENTED_EDGE ( 'NONE', *, *, #37769, .T. ) ;
#17964 = EDGE_CURVE ( 'NONE', #49667, #8311, #4573, .T. ) ;
#17965 = CARTESIAN_POINT ( 'NONE',  ( -19.81499429539154278, 31.87968861126203635, -5.338708898921614043 ) ) ;
#17966 = ORIENTED_EDGE ( 'NONE', *, *, #48331, .F. ) ;
#17967 = LINE ( 'NONE', #33644, #49899 ) ;
#17968 = DIRECTION ( 'NONE',  ( -0.000000000000000000, -1.000000000000000000, -0.000000000000000000 ) ) ;
#17969 = DIRECTION ( 'NONE',  ( -1.000000000000000000, -0.000000000000000000, -0.000000000000000000 ) ) ;
#17970 = CARTESIAN_POINT ( 'NONE',  ( 44.99506233596247995, 23.32283626942318833, 7.455576670931136185 ) ) ;
#17971 = VERTEX_POINT ( 'NONE', #9249 ) ;
#17973 = EDGE_LOOP ( 'NONE', ( #15807, #20718, #48169, #15998, #38955 ) ) ;
#17972 = EDGE_CURVE ( 'NONE', #35976, #22721, #14606, .T. ) ;
#17974 = CARTESIAN_POINT ( 'NONE',  ( -0.1425549192113998442, 1.238581250503548059, 9.981352469109934233 ) ) ;
#17975 = EDGE_CURVE ( 'NONE', #29885, #44630, #26901, .T. ) ;
#17976 = CIRCLE ( 'NONE', #32758, 1.749999999999987566 ) ;
#17977 = EDGE_CURVE ( 'NONE', #22263, #46472, #6653, .T. ) ;
#17978 = EDGE_CURVE ( 'NONE', #9166, #34629, #50414, .T. ) ;
#17979 = VECTOR ( 'NONE', #47282, 1000.000000000000000 ) ;
#17980 = ORIENTED_EDGE ( 'NONE', *, *, #766, .T. ) ;
#17981 = LINE ( 'NONE', #13134, #29212 ) ;
#17982 = CARTESIAN_POINT ( 'NONE',  ( 355.9999999999999432, -183.0000000000001137, -358.0000000000003411 ) ) ;
#17983 = ORIENTED_EDGE ( 'NONE', *, *, #37210, .F. ) ;
#17984 = CARTESIAN_POINT ( 'NONE',  ( -166.6959734468149463, -1.750000000000010214, -39.18171244307202983 ) ) ;
#17985 = VECTOR ( 'NONE', #50004, 1000.000000000000000 ) ;
#17986 = EDGE_CURVE ( 'NONE', #1823, #9976, #15282, .T. ) ;
#17987 = DIRECTION ( 'NONE',  ( -1.000000000000000000, 0.000000000000000000, 0.000000000000000000 ) ) ;
#17988 = ORIENTED_EDGE ( 'NONE', *, *, #6401, .T. ) ;
#17989 = DIRECTION ( 'NONE',  ( -0.000000000000000000, -1.000000000000000000, 2.537652627714643577E-15 ) ) ;
#17990 = CARTESIAN_POINT ( 'NONE',  ( 183.0000000000000000, -256.4999999999998295, -339.9999999999998863 ) ) ;
#17991 = FACE_OUTER_BOUND ( 'NONE', #5312, .T. ) ;
#17992 = CARTESIAN_POINT ( 'NONE',  ( -7.398363427652414614, 15.19415887381139108, -9.008049429158100807 ) ) ;
#17993 = AXIS2_PLACEMENT_3D ( 'NONE', #13686, #6746, #29850 ) ;
#17994 = LINE ( 'NONE', #37532, #1803 ) ;
#17995 = ORIENTED_EDGE ( 'NONE', *, *, #8948, .F. ) ;
#17996 = ORIENTED_EDGE ( 'NONE', *, *, #246, .T. ) ;
#17997 = CARTESIAN_POINT ( 'NONE',  ( -86.69597344681494633, 1.750000000000010658, 80.81828755692798438 ) ) ;
#17998 = CARTESIAN_POINT ( 'NONE',  ( 5.551115123125782702E-14, -180.9999999999999716, 339.9999999999997726 ) ) ;
#17999 = CARTESIAN_POINT ( 'NONE',  ( 9.760995290733820440, -2.173239732351728293, 9.646707543097347681 ) ) ;
#18000 = EDGE_LOOP ( 'NONE', ( #19050, #24490, #6931, #49498 ) ) ;
#18001 = EDGE_CURVE ( 'NONE', #10758, #6007, #21994, .T. ) ;
#18002 = CARTESIAN_POINT ( 'NONE',  ( -49.75871208702130133, 40.58472229863599523, 5.000000000000000000 ) ) ;
#18003 = EDGE_LOOP ( 'NONE', ( #36499, #15609, #34989, #29187, #16162, #41360, #13652, #39623 ) ) ;
#18004 = CARTESIAN_POINT ( 'NONE',  ( -1.249999999999999778, 0.000000000000000000, 10.00000000000000000 ) ) ;
#18005 = DIRECTION ( 'NONE',  ( -1.000000000000000000, 0.000000000000000000, 0.000000000000000000 ) ) ;
#18006 = CARTESIAN_POINT ( 'NONE',  ( -13.35436367797847801, -31.26996044524040741, 7.906207997025717304 ) ) ;
#18007 = EDGE_CURVE ( 'NONE', #639, #16638, #17937, .T. ) ;
#18008 = EDGE_CURVE ( 'NONE', #9652, #50112, #45632, .T. ) ;
#18009 = CARTESIAN_POINT ( 'NONE',  ( -1.164014690938856456, 0.7287989552215266009, 9.946805383069621698 ) ) ;
#18010 = CARTESIAN_POINT ( 'NONE',  ( -164.9999999999978400, 17.00000000000000000, 95.00000000000000000 ) ) ;
#18011 = CARTESIAN_POINT ( 'NONE',  ( -44.94597344681493922, 2.143131898507880377E-16, -120.9317124430720725 ) ) ;
#18012 = ORIENTED_EDGE ( 'NONE', *, *, #28332, .T. ) ;
#18013 = CARTESIAN_POINT ( 'NONE',  ( 194.3291528190321742, -1.750000000000009548, -40.20683870891912193 ) ) ;
#18014 = EDGE_CURVE ( 'NONE', #2864, #47198, #29255, .T. ) ;
#18015 = CARTESIAN_POINT ( 'NONE',  ( 0.000000000000000000, 17.00000000000000000, 0.000000000000000000 ) ) ;
#18016 = CARTESIAN_POINT ( 'NONE',  ( 0.000000000000000000, -175.0000000000000284, -346.2500000000002274 ) ) ;
#18017 = VECTOR ( 'NONE', #32266, 1000.000000000000000 ) ;
#18018 = EDGE_CURVE ( 'NONE', #7014, #43847, #22053, .T. ) ;
#18019 = CIRCLE ( 'NONE', #20520, 4.000000000000003553 ) ;
#18020 = CIRCLE ( 'NONE', #25398, 5.000000000000000000 ) ;
#18021 = DIRECTION ( 'NONE',  ( -0.000000000000000000, -0.000000000000000000, -1.000000000000000000 ) ) ;
#18022 = ORIENTED_EDGE ( 'NONE', *, *, #6826, .T. ) ;
#18023 = FACE_OUTER_BOUND ( 'NONE', #25358, .T. ) ;
#18024 = VERTEX_POINT ( 'NONE', #26160 ) ;
#18025 = VECTOR ( 'NONE', #50714, 1000.000000000000000 ) ;
#18026 = LINE ( 'NONE', #50036, #11518 ) ;
#18027 = DIRECTION ( 'NONE',  ( -0.3090169943749515591, 0.9510565162951523099, 0.000000000000000000 ) ) ;
#18028 = VECTOR ( 'NONE', #13081, 1000.000000000000000 ) ;
#18029 = EDGE_CURVE ( 'NONE', #36234, #33463, #2553, .T. ) ;
#18030 = ORIENTED_EDGE ( 'NONE', *, *, #20042, .F. ) ;
#18031 = AXIS2_PLACEMENT_3D ( 'NONE', #47665, #16932, #4621 ) ;
#18032 = B_SPLINE_CURVE_WITH_KNOTS ( 'NONE', 3,
 ( #48746, #13636, #25447, #21585, #10542, #19244 ),
 .UNSPECIFIED., .F., .F.,
 ( 4, 2, 4 ),
 ( 9.965227682168975268E-18, 0.009877169331704831884, 0.01975433866340965683 ),
 .UNSPECIFIED. ) ;
#18033 = CARTESIAN_POINT ( 'NONE',  ( 6.508636631827673824, 15.75743548351451295, 8.953103998512858652 ) ) ;
#18034 = EDGE_LOOP ( 'NONE', ( #39584, #4149, #43426, #1017, #48351 ) ) ;
#18035 = DIRECTION ( 'NONE',  ( -1.000000000000000000, 0.000000000000000000, 0.000000000000000000 ) ) ;
#18036 = EDGE_CURVE ( 'NONE', #12513, #9595, #8812, .T. ) ;
#18037 = CARTESIAN_POINT ( 'NONE',  ( 0.3862712429686894211, -1.188820645368940276, 9.972675548442463622 ) ) ;
#18038 = VERTEX_POINT ( 'NONE', #44872 ) ;
#18039 = ORIENTED_EDGE ( 'NONE', *, *, #30939, .F. ) ;
#18040 = FACE_OUTER_BOUND ( 'NONE', #24214, .T. ) ;
#18041 = CARTESIAN_POINT ( 'NONE',  ( -177.4999999999999716, -112.5000000000000000, -9.999999999999973355 ) ) ;
#18042 = ADVANCED_FACE ( 'NONE', ( #41056 ), #19504, .T. ) ;
#18043 = B_SPLINE_CURVE_WITH_KNOTS ( 'NONE', 3,
 ( #6507, #22917, #26774, #2890 ),
 .UNSPECIFIED., .F., .F.,
 ( 4, 4 ),
 ( 0.0004299334430849581197, 0.0007706806524480063619 ),
 .UNSPECIFIED. ) ;
#18044 = EDGE_CURVE ( 'NONE', #25202, #10490, #6404, .T. ) ;
#18045 = ORIENTED_EDGE ( 'NONE', *, *, #49269, .T. ) ;
#18046 = ORIENTED_EDGE ( 'NONE', *, *, #16175, .F. ) ;
#18047 = DIRECTION ( 'NONE',  ( -0.000000000000000000, -1.000000000000000000, -0.000000000000000000 ) ) ;
#18048 = CARTESIAN_POINT ( 'NONE',  ( -206.6959734468149463, 1.750000000000010658, 120.8182875569279702 ) ) ;
#18049 = DIRECTION ( 'NONE',  ( 0.000000000000000000, 0.000000000000000000, 1.000000000000000000 ) ) ;
#18050 = ORIENTED_EDGE ( 'NONE', *, *, #29937, .F. ) ;
#18051 = EDGE_CURVE ( 'NONE', #49743, #46654, #49463, .T. ) ;
#18052 = EDGE_LOOP ( 'NONE', ( #11532, #895, #33028, #10074 ) ) ;
#18053 = ADVANCED_FACE ( 'NONE', ( #39244 ), #38734, .F. ) ;
#18054 = EDGE_CURVE ( 'NONE', #16946, #18861, #27431, .T. ) ;
#18055 = LINE ( 'NONE', #17562, #4567 ) ;
#18056 = CIRCLE ( 'NONE', #43476, 4.000000000000003553 ) ;
#18057 =( BOUNDED_CURVE ( )  B_SPLINE_CURVE ( 3, ( #30713, #50141, #42244, #34299 ),
 .UNSPECIFIED., .F., .F. ) 
 B_SPLINE_CURVE_WITH_KNOTS ( ( 4, 4 ),
 ( 3.141592653589793116, 4.712388980384689674 ),
 .UNSPECIFIED. ) 
 CURVE ( )  GEOMETRIC_REPRESENTATION_ITEM ( )  RATIONAL_B_SPLINE_CURVE ( ( 1.000000000000000000, 0.8047378541243649375, 0.8047378541243649375, 1.000000000000000000 ) ) 
 REPRESENTATION_ITEM ( '' )  );
#18058 = CARTESIAN_POINT ( 'NONE',  ( 210.0000000000000568, 0.000000000000000000, 0.8182875569279768335 ) ) ;
#18059 = ORIENTED_EDGE ( 'NONE', *, *, #22742, .T. ) ;
#18060 = VERTEX_POINT ( 'NONE', #249 ) ;
#18061 = VECTOR ( 'NONE', #36076, 1000.000000000000000 ) ;
#18062 = DIRECTION ( 'NONE',  ( 0.000000000000000000, 0.000000000000000000, 1.000000000000000000 ) ) ;
#18063 = VECTOR ( 'NONE', #3994, 1000.000000000000000 ) ;
#18064 = CARTESIAN_POINT ( 'NONE',  ( 339.9999999999999432, 169.0000000000000000, -340.0000000000001705 ) ) ;
#18065 = EDGE_LOOP ( 'NONE', ( #3418, #46354, #28542, #24928 ) ) ;
#18066 = CARTESIAN_POINT ( 'NONE',  ( 168.9999999999999716, -174.9999999999999716, -360.0000000000001705 ) ) ;
#18067 = CIRCLE ( 'NONE', #36973, 3.500000000000003109 ) ;
#18068 = VERTEX_POINT ( 'NONE', #19730 ) ;
#18069 = CARTESIAN_POINT ( 'NONE',  ( 0.000000000000000000, 17.00000000000000000, 0.000000000000000000 ) ) ;
#18070 = VERTEX_POINT ( 'NONE', #43318 ) ;
#18071 = CARTESIAN_POINT ( 'NONE',  ( 181.0000000000000000, -180.9999999999999716, -340.0000000000001137 ) ) ;
#18072 = PLANE ( 'NONE',  #21129 ) ;
#18073 = CARTESIAN_POINT ( 'NONE',  ( 30.00000000000187228, 17.00000000000000000, 65.00000000000000000 ) ) ;
#18074 = CARTESIAN_POINT ( 'NONE',  ( 350.0000000000001137, 165.0000000000000000, 355.9999999999997726 ) ) ;
#18075 = EDGE_CURVE ( 'NONE', #47399, #9715, #12392, .T. ) ;
#18076 = LINE ( 'NONE', #6787, #30722 ) ;
#18077 = VERTEX_POINT ( 'NONE', #8193 ) ;
#18078 = CARTESIAN_POINT ( 'NONE',  ( 36.08557433729230013, -35.58569447144767395, 7.455576670931136185 ) ) ;
#18079 = CARTESIAN_POINT ( 'NONE',  ( 73.30402655318508209, -1.750000000000009992, 160.8182875569279702 ) ) ;
#18080 =( BOUNDED_CURVE ( )  B_SPLINE_CURVE ( 3, ( #16551, #16298, #47552, #16048 ),
 .UNSPECIFIED., .F., .F. ) 
 B_SPLINE_CURVE_WITH_KNOTS ( ( 4, 4 ),
 ( 4.712388980384689674, 6.283185307179586232 ),
 .UNSPECIFIED. ) 
 CURVE ( )  GEOMETRIC_REPRESENTATION_ITEM ( )  RATIONAL_B_SPLINE_CURVE ( ( 1.000000000000000000, 0.8047378541243649375, 0.8047378541243649375, 1.000000000000000000 ) ) 
 REPRESENTATION_ITEM ( '' )  );
#18081 = PRODUCT_RELATED_PRODUCT_CATEGORY ( 'part', '', ( #26565 ) ) ;
#18082 = CARTESIAN_POINT ( 'NONE',  ( 73.30402655318508209, 1.750000000000010214, -39.18171244307202983 ) ) ;
#18083 = DIRECTION ( 'NONE',  ( -1.000000000000000000, 0.000000000000000000, 0.000000000000000000 ) ) ;
#18084 = LINE ( 'NONE', #17460, #24642 ) ;
#18085 = CARTESIAN_POINT ( 'NONE',  ( 111.5540265531850679, 0.000000000000000000, 119.0682875569279844 ) ) ;
#18086 = EDGE_CURVE ( 'NONE', #42215, #35501, #33545, .T. ) ;
#18087 = DIRECTION ( 'NONE',  ( -1.000000000000000000, -0.000000000000000000, -0.000000000000000000 ) ) ;
#18088 = LINE ( 'NONE', #21686, #4998 ) ;
#18089 = VECTOR ( 'NONE', #24811, 1000.000000000000000 ) ;
#18090 = VERTEX_POINT ( 'NONE', #34896 ) ;
#18091 = PRESENTATION_STYLE_ASSIGNMENT (( #31375 ) ) ;
#18092 = AXIS2_PLACEMENT_3D ( 'NONE', #21762, #49669, #3008 ) ;
#18093 = CARTESIAN_POINT ( 'NONE',  ( -126.6959734468149321, 1.749999999999997335, 80.81828755692798438 ) ) ;
#18094 = APPLICATION_CONTEXT ( 'automotive_design' ) ;
#18095 = CARTESIAN_POINT ( 'NONE',  ( 169.0000000000000000, -9.999999999999953815, -97.00000000000014211 ) ) ;
#18096 = FACE_OUTER_BOUND ( 'NONE', #23563, .T. ) ;
#18097 = PLANE ( 'NONE',  #22534 ) ;
#18098 = VERTEX_POINT ( 'NONE', #7171 ) ;
#18099 = VECTOR ( 'NONE', #24797, 1000.000000000000000 ) ;
#18100 = EDGE_LOOP ( 'NONE', ( #7576, #15484, #8157, #25003, #7472, #12154 ) ) ;
#18101 = FACE_OUTER_BOUND ( 'NONE', #5286, .T. ) ;
#18102 = CARTESIAN_POINT ( 'NONE',  ( -47.72109971266203132, 1.750000000000009548, -0.2068387089191121020 ) ) ;
#18103 = EDGE_CURVE ( 'NONE', #47413, #20395, #35664, .T. ) ;
#18104 = ADVANCED_FACE ( 'NONE', ( #19205 ), #7765, .T. ) ;
#18105 = EDGE_LOOP ( 'NONE', ( #23898, #31101, #40640, #35582 ) ) ;
#18106 = CARTESIAN_POINT ( 'NONE',  ( -164.4973046169135955, -61.66198943095990614, -17.65743994998277699 ) ) ;
#18107 = LINE ( 'NONE', #3201, #49466 ) ;
#18108 = ORIENTED_EDGE ( 'NONE', *, *, #29071, .F. ) ;
#18109 = ORIENTED_EDGE ( 'NONE', *, *, #24146, .F. ) ;
#18110 = ORIENTED_EDGE ( 'NONE', *, *, #12416, .F. ) ;
#18111 = EDGE_CURVE ( 'NONE', #13008, #42500, #15883, .T. ) ;
#18113 = EDGE_CURVE ( 'NONE', #39055, #36017, #18951, .T. ) ;
#18112 = CARTESIAN_POINT ( 'NONE',  ( 210.0000000000000568, 2.143131898507880377E-16, -160.9317124430720298 ) ) ;
#18114 = CARTESIAN_POINT ( 'NONE',  ( -207.7210997126620384, 1.750000000000010436, -120.2068387089191219 ) ) ;
#18115 = EDGE_CURVE ( 'NONE', #10975, #49733, #47138, .T. ) ;
#18116 = CARTESIAN_POINT ( 'NONE',  ( 10.30302290646030627, 13.08520913973580058, -9.683996418299976483 ) ) ;
#18117 = ORIENTED_EDGE ( 'NONE', *, *, #43450, .T. ) ;
#18118 = CARTESIAN_POINT ( 'NONE',  ( 75.05402655318509630, 2.143131898507880377E-16, 119.0682875569279560 ) ) ;
#18119 = DIRECTION ( 'NONE',  ( -1.000000000000000000, -0.000000000000000000, -0.000000000000000000 ) ) ;
#18120 = DIRECTION ( 'NONE',  ( 0.000000000000000000, 0.000000000000000000, -1.000000000000000000 ) ) ;
#18121 = ORIENTED_EDGE ( 'NONE', *, *, #18380, .T. ) ;
#18122 = ORIENTED_EDGE ( 'NONE', *, *, #15701, .F. ) ;
#18123 = CYLINDRICAL_SURFACE ( 'NONE', #13122, 2.000000000000001776 ) ;
#18124 = DIRECTION ( 'NONE',  ( 0.2599384441937558354, 0.8000082703740967194, -0.5407575913134976542 ) ) ;
#18125 = EDGE_CURVE ( 'NONE', #30761, #2414, #22814, .T. ) ;
#18126 = CARTESIAN_POINT ( 'NONE',  ( 168.9999999999999716, -77.49999999999997158, -340.0000000000001137 ) ) ;
#18127 = EDGE_LOOP ( 'NONE', ( #49945, #12261, #32407, #15101 ) ) ;
#18128 = VECTOR ( 'NONE', #39112, 1000.000000000000000 ) ;
#18129 = DIRECTION ( 'NONE',  ( -1.000000000000000000, -0.000000000000000000, -0.000000000000000000 ) ) ;
#18130 = FACE_BOUND ( 'NONE', #46494, .T. ) ;
#18131 = LINE ( 'NONE', #41995, #19678 ) ;
#18132 = ORIENTED_EDGE ( 'NONE', *, *, #23160, .T. ) ;
#18133 = AXIS2_PLACEMENT_3D ( 'NONE', #45980, #31399, #27549 ) ;
#18134 = CARTESIAN_POINT ( 'NONE',  ( 30.22736451279166658, 39.84193304692632154, -2.408242355805840784 ) ) ;
#18135 = LINE ( 'NONE', #15055, #24003 ) ;
#18136 = AXIS2_PLACEMENT_3D ( 'NONE', #34211, #6485, #2627 ) ;
#18137 = DIRECTION ( 'NONE',  ( -0.000000000000000000, -0.000000000000000000, 1.000000000000000000 ) ) ;
#18138 = CARTESIAN_POINT ( 'NONE',  ( 17.23491422248386584, -0.5912720620000816441, 8.727788335465566760 ) ) ;
#18139 = B_SPLINE_CURVE_WITH_KNOTS ( 'NONE', 3,
 ( #39470, #24818, #40470, #16106 ),
 .UNSPECIFIED., .F., .F.,
 ( 4, 4 ),
 ( 0.0003309173790299507799, 0.0006447147193715880220 ),
 .UNSPECIFIED. ) ;
#18140 = CARTESIAN_POINT ( 'NONE',  ( -44.94597344681497475, 0.000000000000000000, 162.5682875569279702 ) ) ;
#18141 = VERTEX_POINT ( 'NONE', #11783 ) ;
#18142 = CARTESIAN_POINT ( 'NONE',  ( -206.6959734468149463, 0.000000000000000000, 165.0000000000000000 ) ) ;
#18143 = CARTESIAN_POINT ( 'NONE',  ( 50.24128791297869867, -41.04536285977715693, 5.000000000000000000 ) ) ;
#18144 = CARTESIAN_POINT ( 'NONE',  ( 224.9999999999999716, -164.9999999999999716, 474.9999999999998863 ) ) ;
#18145 = EDGE_CURVE ( 'NONE', #6771, #16019, #21235, .T. ) ;
#18146 = ORIENTED_EDGE ( 'NONE', *, *, #37334, .T. ) ;
#18147 = DIRECTION ( 'NONE',  ( -1.000000000000000000, 0.000000000000000000, 0.000000000000000000 ) ) ;
#18148 = CARTESIAN_POINT ( 'NONE',  ( -165.0000000000000284, 15.00000000000000000, 115.0000000000000142 ) ) ;
#18149 =( BOUNDED_CURVE ( )  B_SPLINE_CURVE ( 3, ( #26118, #18418, #50173, #37951 ),
 .UNSPECIFIED., .F., .F. ) 
 B_SPLINE_CURVE_WITH_KNOTS ( ( 4, 4 ),
 ( 1.570796326794889897, 3.141592653589793116 ),
 .UNSPECIFIED. ) 
 CURVE ( )  GEOMETRIC_REPRESENTATION_ITEM ( )  RATIONAL_B_SPLINE_CURVE ( ( 1.000000000000000000, 0.8047378541243634942, 0.8047378541243634942, 1.000000000000000000 ) ) 
 REPRESENTATION_ITEM ( '' )  );
#18150 = EDGE_LOOP ( 'NONE', ( #33835, #32380, #22089 ) ) ;
#18151 = DIRECTION ( 'NONE',  ( 1.000000000000000000, 0.000000000000000000, 0.000000000000000000 ) ) ;
#18152 = FACE_OUTER_BOUND ( 'NONE', #31568, .T. ) ;
#18153 = CYLINDRICAL_SURFACE ( 'NONE', #33048, 1.750000000000015543 ) ;
#18154 = CARTESIAN_POINT ( 'NONE',  ( 356.0000000000003411, -165.0000000000001137, -92.00000000000019895 ) ) ;
#18155 = CIRCLE ( 'NONE', #11621, 2.000000000000001776 ) ;
#18156 = ORIENTED_EDGE ( 'NONE', *, *, #33987, .F. ) ;
#18157 = CYLINDRICAL_SURFACE ( 'NONE', #28182, 1.750000000000008438 ) ;
#18158 = EDGE_LOOP ( 'NONE', ( #49997, #14694, #35173, #16416 ) ) ;
#18159 = ORIENTED_EDGE ( 'NONE', *, *, #8185, .T. ) ;
#18160 = EDGE_CURVE ( 'NONE', #37586, #9366, #15119, .T. ) ;
#18161 = ORIENTED_EDGE ( 'NONE', *, *, #12112, .F. ) ;
#18162 = VECTOR ( 'NONE', #19850, 1000.000000000000000 ) ;
#18163 = CYLINDRICAL_SURFACE ( 'NONE', #24591, 4.000000000000003553 ) ;
#18164 = CARTESIAN_POINT ( 'NONE',  ( -16.16402646813540755, 4.033894069732547827, -3.546734833711462365 ) ) ;
#18165 = CARTESIAN_POINT ( 'NONE',  ( 389.0218519071287346, 0.000000000000000000, 192.5658166940287970 ) ) ;
#18166 = CARTESIAN_POINT ( 'NONE',  ( 74.32915281903215998, -1.750000000000009548, -0.2068387089191121020 ) ) ;
#18167 = CARTESIAN_POINT ( 'NONE',  ( 344.0000000000000568, 185.0000000000000284, 359.9999999999998295 ) ) ;
#18168 = EDGE_LOOP ( 'NONE', ( #27393, #16300 ) ) ;
#18169 = CARTESIAN_POINT ( 'NONE',  ( 34.38425513258721367, -36.82177522737821107, 8.807470649214879543 ) ) ;
#18171 = EDGE_CURVE ( 'NONE', #23604, #37534, #3823, .T. ) ;
#18170 = DIRECTION ( 'NONE',  ( -1.000000000000000000, -0.000000000000000000, -0.000000000000000000 ) ) ;
#18172 = EDGE_CURVE ( 'NONE', #1473, #22181, #23841, .T. ) ;
#18173 = DIRECTION ( 'NONE',  ( 1.000000000000000000, 0.000000000000000000, 0.000000000000000000 ) ) ;
#18174 = ORIENTED_EDGE ( 'NONE', *, *, #12716, .F. ) ;
#18175 = CARTESIAN_POINT ( 'NONE',  ( 73.30402655318508209, 1.750000000000010214, -39.18171244307202983 ) ) ;
#18176 = DIRECTION ( 'NONE',  ( -1.000000000000000000, 7.930164457481157120E-16, -1.587271980518778491E-16 ) ) ;
#18177 = VERTEX_POINT ( 'NONE', #39500 ) ;
#18178 = ORIENTED_EDGE ( 'NONE', *, *, #21838, .F. ) ;
#18179 = ORIENTED_EDGE ( 'NONE', *, *, #36620, .T. ) ;
#18180 = LINE ( 'NONE', #45851, #34424 ) ;
#18181 = EDGE_CURVE ( 'NONE', #4421, #28864, #7943, .T. ) ;
#18182 = CARTESIAN_POINT ( 'NONE',  ( -1.011271242968693862, 0.7347315653655780432, -3.333333333333333481 ) ) ;
#18183 = EDGE_LOOP ( 'NONE', ( #49518, #16196, #5510, #13317, #31465, #14381 ) ) ;
#18184 = FACE_OUTER_BOUND ( 'NONE', #27669, .T. ) ;
#18185 = CARTESIAN_POINT ( 'NONE',  ( -6.174150299305392053, 50.00000000000000711, 8.807470649214879543 ) ) ;
#18186 = FACE_BOUND ( 'NONE', #11350, .T. ) ;
#18187 = DIRECTION ( 'NONE',  ( 0.000000000000000000, 0.000000000000000000, 1.000000000000000000 ) ) ;
#18188 = EDGE_LOOP ( 'NONE', ( #2959, #6438, #12611, #27559 ) ) ;
#18189 = DIRECTION ( 'NONE',  ( 0.000000000000000000, 0.000000000000000000, 1.000000000000000000 ) ) ;
#18190 = VECTOR ( 'NONE', #13332, 1000.000000000000000 ) ;
#18191 = CARTESIAN_POINT ( 'NONE',  ( 1.011271242968688311, -0.7347315653655855927, 10.00000000000000000 ) ) ;
#18192 = EDGE_LOOP ( 'NONE', ( #48822, #35842, #7582 ) ) ;
#18193 = DIRECTION ( 'NONE',  ( 0.000000000000000000, 0.000000000000000000, 1.000000000000000000 ) ) ;
#18194 = CARTESIAN_POINT ( 'NONE',  ( 24.47767542868285062, -23.18653802921781448, 8.807470649214879543 ) ) ;
#18195 = VECTOR ( 'NONE', #41146, 1000.000000000000227 ) ;
#18196 = CARTESIAN_POINT ( 'NONE',  ( -1.011271242968683426, -0.7347315653655928092, 3.333333333333333481 ) ) ;
#18197 = DIRECTION ( 'NONE',  ( 1.000000000000000000, -4.758098676964957447E-16, 2.958228394578795584E-31 ) ) ;
#18198 = VERTEX_POINT ( 'NONE', #9881 ) ;
#18199 = CARTESIAN_POINT ( 'NONE',  ( -64.99999999999877787, 17.00000000000000000, 30.00000000000000000 ) ) ;
#18200 = CARTESIAN_POINT ( 'NONE',  ( 7.129058724844953510, 15.30620660340485095, 9.178419661560148768 ) ) ;
#18201 = DIRECTION ( 'NONE',  ( 0.000000000000000000, 0.000000000000000000, 1.000000000000000000 ) ) ;
#18202 = CARTESIAN_POINT ( 'NONE',  ( 0.8283411193307036458, 1.889045124114310026, 9.891980816043068003 ) ) ;
#18203 = CARTESIAN_POINT ( 'NONE',  ( -4.945973446814903696, 2.143131898507912917E-16, 165.0000000000000000 ) ) ;
#18204 = EDGE_CURVE ( 'NONE', #13812, #8942, #27454, .T. ) ;
#18205 =( BOUNDED_CURVE ( )  B_SPLINE_CURVE ( 3, ( #447, #47088, #35612, #7898 ),
 .UNSPECIFIED., .F., .F. ) 
 B_SPLINE_CURVE_WITH_KNOTS ( ( 4, 4 ),
 ( 3.141592653589793116, 4.712388980384689674 ),
 .UNSPECIFIED. ) 
 CURVE ( )  GEOMETRIC_REPRESENTATION_ITEM ( )  RATIONAL_B_SPLINE_CURVE ( ( 1.000000000000000000, 0.8047378541243649375, 0.8047378541243649375, 1.000000000000000000 ) ) 
 REPRESENTATION_ITEM ( '' )  );
#18206 = ORIENTED_EDGE ( 'NONE', *, *, #33064, .T. ) ;
#18207 = FACE_OUTER_BOUND ( 'NONE', #17059, .T. ) ;
#18208 = VERTEX_POINT ( 'NONE', #17332 ) ;
#18209 = CARTESIAN_POINT ( 'NONE',  ( 0.4166666666666669072, 0.000000000000000000, 10.00000000000000000 ) ) ;
#18210 = ORIENTED_EDGE ( 'NONE', *, *, #34701, .T. ) ;
#18211 = DIRECTION ( 'NONE',  ( 0.000000000000000000, 0.000000000000000000, 1.000000000000000000 ) ) ;
#18212 = FACE_OUTER_BOUND ( 'NONE', #20286, .T. ) ;
#18213 =( BOUNDED_CURVE ( )  B_SPLINE_CURVE ( 3, ( #19745, #31569, #43336, #38509 ),
 .UNSPECIFIED., .F., .F. ) 
 B_SPLINE_CURVE_WITH_KNOTS ( ( 4, 4 ),
 ( 4.712388980384689674, 6.283185307179586232 ),
 .UNSPECIFIED. ) 
 CURVE ( )  GEOMETRIC_REPRESENTATION_ITEM ( )  RATIONAL_B_SPLINE_CURVE ( ( 1.000000000000000000, 0.8047378541243649375, 0.8047378541243649375, 1.000000000000000000 ) ) 
 REPRESENTATION_ITEM ( '' )  );
#18214 = VECTOR ( 'NONE', #88, 1000.000000000000000 ) ;
#18215 = CARTESIAN_POINT ( 'NONE',  ( 35.05402655318504657, 1.025126265847089657, 79.06828755692797017 ) ) ;
#18216 = ORIENTED_EDGE ( 'NONE', *, *, #27908, .F. ) ;
#18217 = DIRECTION ( 'NONE',  ( 1.000000000000000000, 0.000000000000000000, 0.000000000000000000 ) ) ;
#18218 = VERTEX_POINT ( 'NONE', #13731 ) ;
#18219 = CARTESIAN_POINT ( 'NONE',  ( -45.64490844644706158, -21.32281559348763977, 8.807470649214879543 ) ) ;
#18220 = CARTESIAN_POINT ( 'NONE',  ( -164.4973046169135955, -98.56198943095992604, -17.65743994998277699 ) ) ;
#18221 = VECTOR ( 'NONE', #36403, 1000.000000000000000 ) ;
#18222 = CARTESIAN_POINT ( 'NONE',  ( -12.35406723005387875, 11.51001571518090039, 9.178419661560148768 ) ) ;
#18223 = CARTESIAN_POINT ( 'NONE',  ( 165.0000000000000284, 175.0000000000000284, 343.9999999999998863 ) ) ;
#18224 = VECTOR ( 'NONE', #3875, 1000.000000000000000 ) ;
#18225 = LINE ( 'NONE', #18725, #19170 ) ;
#18226 = ORIENTED_EDGE ( 'NONE', *, *, #5823, .F. ) ;
#18227 = ORIENTED_EDGE ( 'NONE', *, *, #5417, .F. ) ;
#18228 = CARTESIAN_POINT ( 'NONE',  ( -16.52264463346130796, 2.779753662172870232, 9.403735324607438884 ) ) ;
#18229 = VECTOR ( 'NONE', #24924, 1000.000000000000000 ) ;
#18230 = ORIENTED_EDGE ( 'NONE', *, *, #42205, .F. ) ;
#18231 = AXIS2_PLACEMENT_3D ( 'NONE', #27816, #43205, #36033 ) ;
#18232 = LINE ( 'NONE', #14648, #30833 ) ;
#18233 = DIRECTION ( 'NONE',  ( 0.000000000000000000, 0.000000000000000000, -1.000000000000000000 ) ) ;
#18234 = ORIENTED_EDGE ( 'NONE', *, *, #13012, .F. ) ;
#18235 = CARTESIAN_POINT ( 'NONE',  ( -46.69597344681494633, -1.750000000000009992, -159.1817124430720298 ) ) ;
#18236 = EDGE_CURVE ( 'NONE', #9153, #23786, #46406, .T. ) ;
#18237 = CARTESIAN_POINT ( 'NONE',  ( -168.4459734468149747, 1.025126265847089657, 79.06828755692797017 ) ) ;
#18238 = B_SPLINE_SURFACE_WITH_KNOTS ( 'NONE', 3, 3, ( 
 ( #42361, #46435, #38790, #19776 ),
 ( #22615, #42609, #7224, #23379 ),
 ( #34953, #39049, #26970, #298 ),
 ( #31347, #35457, #15427, #39292 ) ),
 .UNSPECIFIED., .F., .F., .F.,
 ( 4, 4 ),
 ( 4, 4 ),
 ( 0.000000000000000000, 1.000000000000000000 ),
 ( 0.000000000000000000, 1.000000000000000000 ),
 .UNSPECIFIED. ) ;
#18239 = ORIENTED_EDGE ( 'NONE', *, *, #31292, .T. ) ;
#18240 = DIRECTION ( 'NONE',  ( -1.000000000000000000, 0.000000000000000000, 0.000000000000000000 ) ) ;
#18241 = CARTESIAN_POINT ( 'NONE',  ( 33.30402655318503946, 1.750000000000010658, -119.1817124430720440 ) ) ;
#18242 = CARTESIAN_POINT ( 'NONE',  ( -24.47767542868268364, 23.18653802921800278, 8.807470649214879543 ) ) ;
#18243 = DIRECTION ( 'NONE',  ( -1.000000000000000000, -0.000000000000000000, -0.000000000000000000 ) ) ;
#18244 = EDGE_LOOP ( 'NONE', ( #20347, #521, #48370, #857 ) ) ;
#18245 = ORIENTED_EDGE ( 'NONE', *, *, #22024, .T. ) ;
#18246 = CARTESIAN_POINT ( 'NONE',  ( -86.69597344681494633, -1.750000000000010214, -39.18171244307202983 ) ) ;
#18247 = ADVANCED_FACE ( 'NONE', ( #2194 ), #36617, .T. ) ;
#18248 = ORIENTED_EDGE ( 'NONE', *, *, #539, .T. ) ;
#18249 = EDGE_CURVE ( 'NONE', #4473, #31718, #10738, .T. ) ;
#18250 = ORIENTED_EDGE ( 'NONE', *, *, #16749, .T. ) ;
#18251 = SHAPE_REPRESENTATION_RELATIONSHIP ( 'NONE' , 'NONE' ,  #39915, #21546 ) ;
#18252 = PLANE ( 'NONE',  #13838 ) ;
#18253 = LINE ( 'NONE', #6975, #19486 ) ;
#18254 = DIRECTION ( 'NONE',  ( -1.612977847700450206E-50, 0.000000000000000000, -1.000000000000000000 ) ) ;
#18255 = FACE_OUTER_BOUND ( 'NONE', #22595, .T. ) ;
#18256 = CARTESIAN_POINT ( 'NONE',  ( -6.695973446814940111, -1.750000000000024203, -119.1817124430720440 ) ) ;
#18257 = DIRECTION ( 'NONE',  ( 8.673617379884028076E-17, -1.000000000000000000, 0.000000000000000000 ) ) ;
#18258 = ORIENTED_EDGE ( 'NONE', *, *, #27728, .F. ) ;
#18259 = DIRECTION ( 'NONE',  ( -1.445602896647339410E-16, -1.000000000000000000, 0.000000000000000000 ) ) ;
#18260 = AXIS2_PLACEMENT_3D ( 'NONE', #17933, #41303, #5896 ) ;
#18261 = CARTESIAN_POINT ( 'NONE',  ( 34.32915281903212446, -1.750000000000009548, -40.20683870891912193 ) ) ;
#18262 = CARTESIAN_POINT ( 'NONE',  ( -69.99999999999972999, 16.00000000000000000, -84.99999999999998579 ) ) ;
#18263 = ADVANCED_FACE ( 'NONE', ( #40440 ), #25793, .F. ) ;
#18264 = VECTOR ( 'NONE', #43523, 1000.000000000000000 ) ;
#18265 = ADVANCED_FACE ( 'NONE', ( #17832 ), #21942, .F. ) ;
#18266 = CARTESIAN_POINT ( 'NONE',  ( -0.7248414106044189786, 1.181973560820994917, 9.960027343378008879 ) ) ;
#18267 = ORIENTED_EDGE ( 'NONE', *, *, #27406, .F. ) ;
#18268 = AXIS2_PLACEMENT_3D ( 'NONE', #15629, #31555, #35408 ) ;
#18269 = CARTESIAN_POINT ( 'NONE',  ( 115.0540265531850395, 2.143131898507847836E-16, 82.56828755692797017 ) ) ;
#18270 = ORIENTED_EDGE ( 'NONE', *, *, #32849, .F. ) ;
#18271 = LINE ( 'NONE', #6246, #17195 ) ;
#18272 = CARTESIAN_POINT ( 'NONE',  ( 339.9999999999999432, -181.0000000000001421, 356.0000000000000000 ) ) ;
#18273 = CARTESIAN_POINT ( 'NONE',  ( -225.0000000000000568, -175.0000000000000000, 0.000000000000000000 ) ) ;
#18274 = ORIENTED_EDGE ( 'NONE', *, *, #440, .T. ) ;
#18275 = CARTESIAN_POINT ( 'NONE',  ( 191.5540265531851105, 0.000000000000000000, 165.0000000000000000 ) ) ;
#18276 = ORIENTED_EDGE ( 'NONE', *, *, #3989, .T. ) ;
#18277 = CARTESIAN_POINT ( 'NONE',  ( -239.0000000000000853, -153.6999999999999602, 250.3600000000000136 ) ) ;
#18278 = CARTESIAN_POINT ( 'NONE',  ( -88.44597344681494633, -1.025126265847089879, 122.5682875569280128 ) ) ;
#18279 = EDGE_LOOP ( 'NONE', ( #27661, #1893, #11564, #11, #45107, #31263 ) ) ;
#18280 = EDGE_LOOP ( 'NONE', ( #23476, #24501, #24783 ) ) ;
#18281 = ADVANCED_FACE ( 'NONE', ( #13975 ), #33503, .T. ) ;
#18282 = PLANE ( 'NONE',  #48012 ) ;
#18283 = CARTESIAN_POINT ( 'NONE',  ( -8.445973446814976526, 0.000000000000000000, -37.43171244307200141 ) ) ;
#18284 = ADVANCED_FACE ( 'NONE', ( #28886 ), #5280, .F. ) ;
#18285 = VERTEX_POINT ( 'NONE', #48335 ) ;
#18286 = ADVANCED_FACE ( 'NONE', ( #1445 ), #36452, .T. ) ;
#18287 = ORIENTED_EDGE ( 'NONE', *, *, #23972, .F. ) ;
#18288 = CARTESIAN_POINT ( 'NONE',  ( 1.019713130072856355, 3.848720492505100843, 4.370690007832189750E-16 ) ) ;
#18289 = CARTESIAN_POINT ( 'NONE',  ( 168.9999999999999716, -268.5000000000000000, -114.9999999999999147 ) ) ;
#18290 = AXIS2_PLACEMENT_3D ( 'NONE', #33404, #45147, #28781 ) ;
#18291 = CARTESIAN_POINT ( 'NONE',  ( 0.000000000000000000, 175.0000000000000284, -350.0000000000002274 ) ) ;
#18292 = VERTEX_POINT ( 'NONE', #44764 ) ;
#18293 = DIRECTION ( 'NONE',  ( 0.000000000000000000, 0.000000000000000000, 1.000000000000000000 ) ) ;
#18294 = EDGE_CURVE ( 'NONE', #37965, #27105, #44260, .T. ) ;
#18295 = VECTOR ( 'NONE', #40063, 1000.000000000000000 ) ;
#18296 = ORIENTED_EDGE ( 'NONE', *, *, #29276, .F. ) ;
#18297 = AXIS2_PLACEMENT_3D ( 'NONE', #15966, #24932, #16712 ) ;
#18298 = EDGE_CURVE ( 'NONE', #20787, #13604, #36870, .T. ) ;
#18299 = CARTESIAN_POINT ( 'NONE',  ( 85.00000000000123634, 17.00000000000000000, 30.00000000000000000 ) ) ;
#18300 = CARTESIAN_POINT ( 'NONE',  ( -14.99999999999782041, 16.00000000000000000, 95.00000000000000000 ) ) ;
#18301 = PRESENTATION_LAYER_ASSIGNMENT (  '', '', ( #39544 ) ) ;
#18302 = VERTEX_POINT ( 'NONE', #29141 ) ;
#18303 = VERTEX_POINT ( 'NONE', #40938 ) ;
#18304 = CARTESIAN_POINT ( 'NONE',  ( 80.00000000000153477, 17.00000000000000000, 35.00000000000000000 ) ) ;
#18305 = FACE_OUTER_BOUND ( 'NONE', #14653, .T. ) ;
#18306 = ORIENTED_EDGE ( 'NONE', *, *, #23846, .T. ) ;
#18307 = CARTESIAN_POINT ( 'NONE',  ( 14.49999999999999822, 12.87566193687862715, 19.86060803177194600 ) ) ;
#18308 = VERTEX_POINT ( 'NONE', #5783 ) ;
#18309 = CARTESIAN_POINT ( 'NONE',  ( -6.695973446814940111, 0.000000000000000000, 165.0000000000000000 ) ) ;
#18310 = LINE ( 'NONE', #41932, #24000 ) ;
#18311 = ORIENTED_EDGE ( 'NONE', *, *, #50627, .F. ) ;
#18312 = CARTESIAN_POINT ( 'NONE',  ( -46.69597344681494633, -1.750000000000010658, -79.18171244307201562 ) ) ;
#18313 = CARTESIAN_POINT ( 'NONE',  ( 114.3291528190321173, -1.749999999999997113, 119.7931612910809065 ) ) ;
#18314 = CARTESIAN_POINT ( 'NONE',  ( 9.998889670239195837, 0.1490146381531976816, 9.282506307616472441 ) ) ;
#18315 = DIRECTION ( 'NONE',  ( -1.000000000000000000, 0.000000000000000000, -1.612977847700450206E-50 ) ) ;
#18316 = VECTOR ( 'NONE', #37593, 1000.000000000000000 ) ;
#18317 = EDGE_LOOP ( 'NONE', ( #36156, #25998, #398 ) ) ;
#18318 = DIRECTION ( 'NONE',  ( 1.000000000000000000, 0.000000000000000000, 0.000000000000000000 ) ) ;
#18319 = CARTESIAN_POINT ( 'NONE',  ( -2.052581215100349521, 0.2042358160481012597, 9.886433018048073507 ) ) ;
#18320 = CARTESIAN_POINT ( 'NONE',  ( 0.000000000000000000, 165.2000000000000171, 359.7999999999997840 ) ) ;
#18321 = CARTESIAN_POINT ( 'NONE',  ( 0.3862712429686810944, 1.188820645368943607, 10.00000000000000000 ) ) ;
#18322 = EDGE_CURVE ( 'NONE', #40029, #38870, #17584, .T. ) ;
#18323 = EDGE_CURVE ( 'NONE', #8111, #48485, #14491, .T. ) ;
#18324 = EDGE_CURVE ( 'NONE', #18292, #50400, #7297, .T. ) ;
#18325 = EDGE_CURVE ( 'NONE', #12576, #36969, #45404, .T. ) ;
#18326 = DIRECTION ( 'NONE',  ( -1.000000000000000000, -0.000000000000000000, -0.000000000000000000 ) ) ;
#18327 = CARTESIAN_POINT ( 'NONE',  ( 195.9526953830863079, -154.8119894309599260, 472.5992458228020610 ) ) ;
#18328 = EDGE_CURVE ( 'NONE', #31501, #18070, #2442, .T. ) ;
#18329 = VECTOR ( 'NONE', #36417, 1000.000000000000000 ) ;
#18330 = CARTESIAN_POINT ( 'NONE',  ( 135.0000000000009663, 16.00000000000000000, 0.000000000000000000 ) ) ;
#18331 = EDGE_CURVE ( 'NONE', #38661, #7012, #20865, .T. ) ;
#18332 = CARTESIAN_POINT ( 'NONE',  ( 0.000000000000000000, 0.000000000000000000, 800.0000000000000000 ) ) ;
#18333 = AXIS2_PLACEMENT_3D ( 'NONE', #19466, #35151, #42313 ) ;
#18334 = EDGE_LOOP ( 'NONE', ( #33869, #40052, #27854, #2517 ) ) ;
#18335 = LINE ( 'NONE', #49842, #36360 ) ;
#18336 = CARTESIAN_POINT ( 'NONE',  ( -16.73672383626882976, -2.341008440547994063, -9.008049429158100807 ) ) ;
#18337 = CARTESIAN_POINT ( 'NONE',  ( -5.888214538810513154, -16.20866436362413410, 8.727788335465566760 ) ) ;
#18338 = CARTESIAN_POINT ( 'NONE',  ( 1.011271242968677653, 0.7347315653656002477, -10.00000000000000000 ) ) ;
#18339 = DIRECTION ( 'NONE',  ( -1.000000000000000000, -0.000000000000000000, -0.000000000000000000 ) ) ;
#18340 = ORIENTED_EDGE ( 'NONE', *, *, #16899, .F. ) ;
#18341 = PRODUCT_DEFINITION_SHAPE ( 'NONE', 'NONE',  #47817 ) ;
#18342 = ORIENTED_EDGE ( 'NONE', *, *, #15787, .F. ) ;
#18343 = ADVANCED_FACE ( 'NONE', ( #46009 ), #10895, .T. ) ;
#18344 = CARTESIAN_POINT ( 'NONE',  ( 35.00000000000122213, 17.00000000000000000, 30.00000000000000000 ) ) ;
#18345 = DIRECTION ( 'NONE',  ( 1.000000000000000000, -0.000000000000000000, 0.000000000000000000 ) ) ;
#18346 =( BOUNDED_CURVE ( )  B_SPLINE_CURVE ( 3, ( #16292, #31709, #47546, #48044 ),
 .UNSPECIFIED., .F., .F. ) 
 B_SPLINE_CURVE_WITH_KNOTS ( ( 4, 4 ),
 ( 0.000000000000000000, 1.570796326794896558 ),
 .UNSPECIFIED. ) 
 CURVE ( )  GEOMETRIC_REPRESENTATION_ITEM ( )  RATIONAL_B_SPLINE_CURVE ( ( 1.000000000000000000, 0.8047378541243649375, 0.8047378541243649375, 1.000000000000000000 ) ) 
 REPRESENTATION_ITEM ( '' )  );
#18347 = VECTOR ( 'NONE', #29197, 1000.000000000000000 ) ;
#18348 = EDGE_CURVE ( 'NONE', #40036, #17662, #6540, .T. ) ;
#18349 = ORIENTED_EDGE ( 'NONE', *, *, #37885, .T. ) ;
#18350 = EDGE_CURVE ( 'NONE', #35947, #13085, #50715, .T. ) ;
#18351 = DIRECTION ( 'NONE',  ( -0.000000000000000000, -0.000000000000000000, -1.000000000000000000 ) ) ;
#18352 = CARTESIAN_POINT ( 'NONE',  ( 192.2789002873380184, -1.750000000000009548, 1.843413822775065825 ) ) ;
#18353 = LINE ( 'NONE', #28724, #47150 ) ;
#18354 = VERTEX_POINT ( 'NONE', #26549 ) ;
#18355 = VERTEX_POINT ( 'NONE', #42186 ) ;
#18356 =( BOUNDED_CURVE ( )  B_SPLINE_CURVE ( 3, ( #2476, #48621, #45792, #49380 ),
 .UNSPECIFIED., .F., .F. ) 
 B_SPLINE_CURVE_WITH_KNOTS ( ( 4, 4 ),
 ( 3.141592653589793116, 4.712388980384689674 ),
 .UNSPECIFIED. ) 
 CURVE ( )  GEOMETRIC_REPRESENTATION_ITEM ( )  RATIONAL_B_SPLINE_CURVE ( ( 1.000000000000000000, 0.8047378541243649375, 0.8047378541243649375, 1.000000000000000000 ) ) 
 REPRESENTATION_ITEM ( '' )  );
#18357 = ORIENTED_EDGE ( 'NONE', *, *, #3989, .F. ) ;
#18358 = CARTESIAN_POINT ( 'NONE',  ( -4.999999999999997335, 204.9999999999999716, -234.7500000000000000 ) ) ;
#18359 = DIRECTION ( 'NONE',  ( 0.000000000000000000, 0.000000000000000000, 1.000000000000000000 ) ) ;
#18360 = CARTESIAN_POINT ( 'NONE',  ( 15.73090589902275482, 29.60029367929053024, 1.847720168420772691 ) ) ;
#18361 = EDGE_LOOP ( 'NONE', ( #9632, #6107 ) ) ;
#18362 = CARTESIAN_POINT ( 'NONE',  ( -208.4459734468148611, -1.025126265847089879, 82.56828755692798438 ) ) ;
#18363 = FACE_OUTER_BOUND ( 'NONE', #22260, .T. ) ;
#18364 = CARTESIAN_POINT ( 'NONE',  ( 130.0000000000012221, 17.00000000000000000, 5.000000000000004441 ) ) ;
#18365 = AXIS2_PLACEMENT_3D ( 'NONE', #20962, #32766, #37141 ) ;
#18366 = VERTEX_POINT ( 'NONE', #33755 ) ;
#18367 = VERTEX_POINT ( 'NONE', #34005 ) ;
#18368 = CARTESIAN_POINT ( 'NONE',  ( 169.0000000000000000, -174.9999999999999716, -99.00000000000014211 ) ) ;
#18369 = AXIS2_PLACEMENT_3D ( 'NONE', #68, #20061, #825 ) ;
#18370 = EDGE_CURVE ( 'NONE', #46071, #12379, #41687, .T. ) ;
#18371 = CARTESIAN_POINT ( 'NONE',  ( -6.695973446814940111, -1.750000000000023759, -39.18171244307202983 ) ) ;
#18372 =( BOUNDED_CURVE ( )  B_SPLINE_CURVE ( 3, ( #5067, #1741, #6087, #16628 ),
 .UNSPECIFIED., .F., .F. ) 
 B_SPLINE_CURVE_WITH_KNOTS ( ( 4, 4 ),
 ( 4.712388980384689674, 6.283185307179586232 ),
 .UNSPECIFIED. ) 
 CURVE ( )  GEOMETRIC_REPRESENTATION_ITEM ( )  RATIONAL_B_SPLINE_CURVE ( ( 1.000000000000000000, 0.8047378541243649375, 0.8047378541243649375, 1.000000000000000000 ) ) 
 REPRESENTATION_ITEM ( '' )  );
#18373 = CARTESIAN_POINT ( 'NONE',  ( 0.3910393408562611861, 3.877122853646846945, 9.741991644046958498 ) ) ;
#18374 = EDGE_LOOP ( 'NONE', ( #39664, #12948, #43163, #4105 ) ) ;
#18375 = AXIS2_PLACEMENT_3D ( 'NONE', #40606, #4935, #48755 ) ;
#18376 = LINE ( 'NONE', #10436, #23332 ) ;
#18377 = DIRECTION ( 'NONE',  ( -1.000000000000000000, 0.000000000000000000, 0.000000000000000000 ) ) ;
#18378 = CARTESIAN_POINT ( 'NONE',  ( -124.9459734468149463, 2.143131898507842906E-16, -165.0000000000000000 ) ) ;
#18379 = CARTESIAN_POINT ( 'NONE',  ( 340.0000000000000568, 169.0000000000000000, 355.9999999999997726 ) ) ;
#18380 = EDGE_CURVE ( 'NONE', #30787, #40281, #18830, .T. ) ;
#18381 = CARTESIAN_POINT ( 'NONE',  ( 2.569099690548740877, -33.19126772784019153, 3.199614146704519602 ) ) ;
#18382 = EDGE_LOOP ( 'NONE', ( #28224, #20442, #16921, #19203, #30320, #26377 ) ) ;
#18383 = FILL_AREA_STYLE_COLOUR ( '', #36497 ) ;
#18384 = CARTESIAN_POINT ( 'NONE',  ( -84.94597344681494633, 2.143131898507880377E-16, 42.56828755692798438 ) ) ;
#18385 = LINE ( 'NONE', #10195, #8477 ) ;
#18386 = CARTESIAN_POINT ( 'NONE',  ( -164.9459734468149463, 2.143131898507880377E-16, -160.9317124430720014 ) ) ;
#18387 = CARTESIAN_POINT ( 'NONE',  ( -17.51065725283106289, 28.41934970907792746, -9.367992836599954742 ) ) ;
#18388 = ADVANCED_FACE ( 'NONE', ( #14227 ), #38364, .T. ) ;
#18389 = VECTOR ( 'NONE', #2610, 1000.000000000000000 ) ;
#18390 = EDGE_CURVE ( 'NONE', #36453, #33652, #5290, .T. ) ;
#18391 = FACE_OUTER_BOUND ( 'NONE', #37850, .T. ) ;
#18392 = AXIS2_PLACEMENT_3D ( 'NONE', #34778, #50352, #30146 ) ;
#18393 = ORIENTED_EDGE ( 'NONE', *, *, #3975, .T. ) ;
#18394 = DIRECTION ( 'NONE',  ( 1.000000000000000000, 0.000000000000000000, 0.000000000000000000 ) ) ;
#18395 = ADVANCED_FACE ( 'NONE', ( #3437 ), #19087, .T. ) ;
#18396 = LINE ( 'NONE', #34077, #38127 ) ;
#18397 = LINE ( 'NONE', #18144, #5843 ) ;
#18398 = EDGE_CURVE ( 'NONE', #36524, #21893, #6627, .T. ) ;
#18399 = EDGE_CURVE ( 'NONE', #45613, #49664, #45752, .T. ) ;
#18400 = EDGE_LOOP ( 'NONE', ( #35592, #11030, #9767, #22688 ) ) ;
#18401 = CARTESIAN_POINT ( 'NONE',  ( -177.4999999999999716, 57.49999999999996447, -9.999999999999973355 ) ) ;
#18402 = CARTESIAN_POINT ( 'NONE',  ( -4.339432828817248122, -37.24807810779213213, -8.192531242611266862 ) ) ;
#18403 = VECTOR ( 'NONE', #40153, 1000.000000000000000 ) ;
#18404 = ORIENTED_EDGE ( 'NONE', *, *, #9852, .F. ) ;
#18405 = CARTESIAN_POINT ( 'NONE',  ( -0.6215990105957072132, 1.608617984725374983, 9.928159647716134018 ) ) ;
#18406 = PLANE ( 'NONE',  #18092 ) ;
#18407 = CARTESIAN_POINT ( 'NONE',  ( 7.203307948779654524, -6.979912421814508328, 9.516222621873129839 ) ) ;
#18408 = DIRECTION ( 'NONE',  ( 0.000000000000000000, 0.000000000000000000, 1.000000000000000000 ) ) ;
#18409 = ADVANCED_FACE ( 'NONE', ( #12169 ), #39386, .T. ) ;
#18410 = ORIENTED_EDGE ( 'NONE', *, *, #4360, .T. ) ;
#18411 = LINE ( 'NONE', #46588, #33136 ) ;
#18412 = VERTEX_POINT ( 'NONE', #31687 ) ;
#18413 = ORIENTED_EDGE ( 'NONE', *, *, #4974, .F. ) ;
#18414 = AXIS2_PLACEMENT_3D ( 'NONE', #49576, #48574, #48823 ) ;
#18415 = CARTESIAN_POINT ( 'NONE',  ( -4.945973446814916130, -1.025126265847097429, -120.9317124430720440 ) ) ;
#18416 = ORIENTED_EDGE ( 'NONE', *, *, #48342, .T. ) ;
#18417 = DIRECTION ( 'NONE',  ( 0.000000000000000000, 0.000000000000000000, -1.000000000000000000 ) ) ;
#18418 = CARTESIAN_POINT ( 'NONE',  ( 359.9999999999998863, -183.3431457505077447, -358.3431457505079152 ) ) ;
#18419 = FACE_OUTER_BOUND ( 'NONE', #171, .T. ) ;
#18420 = LINE ( 'NONE', #41772, #4322 ) ;
#18421 = DIRECTION ( 'NONE',  ( -0.000000000000000000, -0.000000000000000000, -1.000000000000000000 ) ) ;
#18422 = VERTEX_POINT ( 'NONE', #28322 ) ;
#18423 = DIRECTION ( 'NONE',  ( -0.000000000000000000, -1.000000000000000000, -0.000000000000000000 ) ) ;
#18424 = LINE ( 'NONE', #30489, #15974 ) ;
#18425 = PLANE ( 'NONE',  #21783 ) ;
#18426 = EDGE_LOOP ( 'NONE', ( #43406, #2233, #27806, #44434 ) ) ;
#18427 = CARTESIAN_POINT ( 'NONE',  ( 1.365263087672787590, -0.5437404457008400138, 9.958264684458717042 ) ) ;
#18428 = CARTESIAN_POINT ( 'NONE',  ( 165.0000000000000284, 165.0000000000000000, 343.9999999999998863 ) ) ;
#18429 = EDGE_LOOP ( 'NONE', ( #2341, #36627, #46675, #39223 ) ) ;
#18430 = CIRCLE ( 'NONE', #48683, 2.000000000000001776 ) ;
#18431 = EDGE_LOOP ( 'NONE', ( #17721, #48812 ) ) ;
#18432 = ORIENTED_EDGE ( 'NONE', *, *, #11462, .F. ) ;
#18433 = CARTESIAN_POINT ( 'NONE',  ( -1.231028901681122445, -0.08486789822041165832, 9.969907203203806745 ) ) ;
#18434 = CARTESIAN_POINT ( 'NONE',  ( 33.47329838550567160, -31.99020508012700148, 7.455576670931137073 ) ) ;
#18435 = VERTEX_POINT ( 'NONE', #42944 ) ;
#18436 = EDGE_CURVE ( 'NONE', #8682, #42453, #48766, .T. ) ;
#18437 = CYLINDRICAL_SURFACE ( 'NONE', #50353, 1.750000000000001554 ) ;
#18438 = FILL_AREA_STYLE_COLOUR ( '', #882 ) ;
#18439 = FACE_BOUND ( 'NONE', #33715, .T. ) ;
#18440 =( GEOMETRIC_REPRESENTATION_CONTEXT ( 3 ) GLOBAL_UNCERTAINTY_ASSIGNED_CONTEXT ( ( #28691 ) ) GLOBAL_UNIT_ASSIGNED_CONTEXT ( ( #22748, #2491, #49397 ) ) REPRESENTATION_CONTEXT ( 'NONE', 'WORKASPACE' ) );
#18441 = CARTESIAN_POINT ( 'NONE',  ( -128.4459734468149463, -1.025126265847082108, 42.56828755692797017 ) ) ;
#18442 = DIRECTION ( 'NONE',  ( -0.000000000000000000, -0.000000000000000000, -1.000000000000000000 ) ) ;
#18443 = ORIENTED_EDGE ( 'NONE', *, *, #11250, .T. ) ;
#18444 = AXIS2_PLACEMENT_3D ( 'NONE', #43292, #8164, #24069 ) ;
#18445 = CARTESIAN_POINT ( 'NONE',  ( 168.9999999999999716, -9.999999999999953815, 339.9999999999998295 ) ) ;
#18446 = CARTESIAN_POINT ( 'NONE',  ( 344.0000000000001705, 165.0000000000000000, -340.0000000000001137 ) ) ;
#18447 = CARTESIAN_POINT ( 'NONE',  ( -42.07173315646050327, 18.54977254542426124, -8.016098858316205167 ) ) ;
#18448 = AXIS2_PLACEMENT_3D ( 'NONE', #28191, #20472, #16895 ) ;
#18449 = ORIENTED_EDGE ( 'NONE', *, *, #20507, .T. ) ;
#18450 = LINE ( 'NONE', #21299, #49439 ) ;
#18451 = DIRECTION ( 'NONE',  ( -1.586032880504786307E-16, 1.654361225106055350E-24, -1.000000000000000000 ) ) ;
#18452 = EDGE_CURVE ( 'NONE', #48180, #35326, #4723, .T. ) ;
#18453 = ADVANCED_FACE ( 'NONE', ( #31936 ), #35039, .T. ) ;
#18454 =( BOUNDED_CURVE ( )  B_SPLINE_CURVE ( 3, ( #12119, #20565, #23910, #47221 ),
 .UNSPECIFIED., .F., .F. ) 
 B_SPLINE_CURVE_WITH_KNOTS ( ( 4, 4 ),
 ( 0.000000000000000000, 1.570796326794896558 ),
 .UNSPECIFIED. ) 
 CURVE ( )  GEOMETRIC_REPRESENTATION_ITEM ( )  RATIONAL_B_SPLINE_CURVE ( ( 1.000000000000000000, 0.8047378541243649375, 0.8047378541243649375, 1.000000000000000000 ) ) 
 REPRESENTATION_ITEM ( '' )  );
#18455 = LINE ( 'NONE', #37984, #40484 ) ;
#18456 = CARTESIAN_POINT ( 'NONE',  ( -44.94597344681493922, -1.025126265847089435, 39.06828755692797728 ) ) ;
#18457 = VERTEX_POINT ( 'NONE', #47277 ) ;
#18458 = CARTESIAN_POINT ( 'NONE',  ( -33.14391172085785797, -37.72293746533095060, -8.016098858316199838 ) ) ;
#18459 = CARTESIAN_POINT ( 'NONE',  ( 210.0000000000000568, 0.000000000000000000, 40.81828755692798438 ) ) ;
#18460 = CARTESIAN_POINT ( 'NONE',  ( 0.3862712429686727678, 1.188820645368945605, 3.333333333333333481 ) ) ;
#18461 = CARTESIAN_POINT ( 'NONE',  ( -3.229232847726260403, 16.57333684275945629, 9.178419661560148768 ) ) ;
#18462 = CARTESIAN_POINT ( 'NONE',  ( 130.0000000000018474, 17.00000000000000000, 65.00000000000000000 ) ) ;
#18463 = ADVANCED_FACE ( 'NONE', ( #4466 ), #50608, .F. ) ;
#18464 = ADVANCED_FACE ( 'NONE', ( #4219 ), #15755, .T. ) ;
#18465 = ORIENTED_EDGE ( 'NONE', *, *, #17951, .F. ) ;
#18466 = VECTOR ( 'NONE', #33460, 1000.000000000000000 ) ;
#18467 = CARTESIAN_POINT ( 'NONE',  ( -46.69597344681494633, -1.750000000000010658, 120.8182875569279702 ) ) ;
#18468 = ORIENTED_EDGE ( 'NONE', *, *, #24988, .F. ) ;
#18469 = CARTESIAN_POINT ( 'NONE',  ( -86.69597344681494633, 1.750000000000010214, 40.81828755692798438 ) ) ;
#18470 = AXIS2_PLACEMENT_3D ( 'NONE', #3496, #15064, #31491 ) ;
#18471 = ORIENTED_EDGE ( 'NONE', *, *, #2761, .F. ) ;
#18472 = EDGE_CURVE ( 'NONE', #18302, #25384, #7155, .T. ) ;
#18473 = CARTESIAN_POINT ( 'NONE',  ( 0.000000000000000000, 0.000000000000000000, 900.0000000000000000 ) ) ;
#18474 = AXIS2_PLACEMENT_3D ( 'NONE', #48702, #44131, #24415 ) ;
#18475 = VERTEX_POINT ( 'NONE', #20362 ) ;
#18476 = FACE_OUTER_BOUND ( 'NONE', #39803, .T. ) ;
#18477 = ORIENTED_EDGE ( 'NONE', *, *, #21582, .F. ) ;
#18478 = AXIS2_PLACEMENT_3D ( 'NONE', #42869, #31093, #6721 ) ;
#18479 = CARTESIAN_POINT ( 'NONE',  ( -84.94597344681493212, -1.025126265847089213, -0.9317124430720324924 ) ) ;
#18480 = ORIENTED_EDGE ( 'NONE', *, *, #6034, .F. ) ;
#18481 = CARTESIAN_POINT ( 'NONE',  ( 80.00000000000061107, 17.00000000000000000, -54.99999999999999289 ) ) ;
#18482 = AXIS2_PLACEMENT_3D ( 'NONE', #47121, #27925, #27416 ) ;
#18483 = DIRECTION ( 'NONE',  ( 0.000000000000000000, 0.000000000000000000, 1.000000000000000000 ) ) ;
#18484 = DIRECTION ( 'NONE',  ( -0.000000000000000000, -1.000000000000000000, -0.000000000000000000 ) ) ;
#18485 = DIRECTION ( 'NONE',  ( 0.000000000000000000, 0.000000000000000000, 1.000000000000000000 ) ) ;
#18486 = ORIENTED_EDGE ( 'NONE', *, *, #47449, .F. ) ;
#18487 = CARTESIAN_POINT ( 'NONE',  ( 4.339432828817248122, 37.24807810779213213, -8.192531242611266862 ) ) ;
#18488 = ORIENTED_EDGE ( 'NONE', *, *, #47983, .T. ) ;
#18489 = DIRECTION ( 'NONE',  ( 0.000000000000000000, 0.000000000000000000, 1.000000000000000000 ) ) ;
#18490 = VECTOR ( 'NONE', #5276, 1000.000000000000000 ) ;
#18491 = CIRCLE ( 'NONE', #20144, 2.000000000000001776 ) ;
#18492 = EDGE_LOOP ( 'NONE', ( #16560, #41039, #10040, #37727, #45294, #45449 ) ) ;
#18493 = CARTESIAN_POINT ( 'NONE',  ( -225.0000000000000284, 175.0000000000000000, 500.0000000000000000 ) ) ;
#18494 = ORIENTED_EDGE ( 'NONE', *, *, #27024, .T. ) ;
#18495 = CARTESIAN_POINT ( 'NONE',  ( 0.3139796262078408673, -1.230474926876621078, 9.975314328424616406 ) ) ;
#18496 = ADVANCED_FACE ( 'NONE', ( #379 ), #36037, .T. ) ;
#18497 = CARTESIAN_POINT ( 'NONE',  ( -15.00199999999999712, -34.54492135858216528, 0.000000000000000000 ) ) ;
#18498 = ORIENTED_EDGE ( 'NONE', *, *, #44681, .F. ) ;
#18499 = ADVANCED_FACE ( 'NONE', ( #19600 ), #16024, .T. ) ;
#18500 = CARTESIAN_POINT ( 'NONE',  ( -1.448406091252275818, 0.9360325558308429938, 9.928159647716187308 ) ) ;
#18501 = CARTESIAN_POINT ( 'NONE',  ( -0.3370904143228927730, -0.2449105217885335917, 10.00000000000000000 ) ) ;
#18502 = CARTESIAN_POINT ( 'NONE',  ( 185.0000000000000000, -180.9999999999999716, -340.0000000000000000 ) ) ;
#18503 = DIRECTION ( 'NONE',  ( -0.000000000000000000, -1.000000000000000000, -0.000000000000000000 ) ) ;
#18504 = AXIS2_PLACEMENT_3D ( 'NONE', #10293, #7202, #6946 ) ;
#18505 = VERTEX_POINT ( 'NONE', #43957 ) ;
#18506 = ORIENTED_EDGE ( 'NONE', *, *, #39267, .T. ) ;
#18507 = VECTOR ( 'NONE', #19945, 1000.000000000000000 ) ;
#18508 = CARTESIAN_POINT ( 'NONE',  ( -34.38425513258695077, 36.82177522737848108, 8.807470649214879543 ) ) ;
#18509 = CARTESIAN_POINT ( 'NONE',  ( -128.4459734468149463, -1.025126265847081442, -160.9317124430720014 ) ) ;
#18510 = ORIENTED_EDGE ( 'NONE', *, *, #31244, .F. ) ;
#18511 = VERTEX_POINT ( 'NONE', #27821 ) ;
#18512 = CARTESIAN_POINT ( 'NONE',  ( 194.9999999999999432, -173.0000000000000000, 112.0000000000000284 ) ) ;
#18513 =( BOUNDED_CURVE ( )  B_SPLINE_CURVE ( 3, ( #30116, #45219, #40665, #5499 ),
 .UNSPECIFIED., .F., .F. ) 
 B_SPLINE_CURVE_WITH_KNOTS ( ( 4, 4 ),
 ( 0.000000000000000000, 1.570796326794896558 ),
 .UNSPECIFIED. ) 
 CURVE ( )  GEOMETRIC_REPRESENTATION_ITEM ( )  RATIONAL_B_SPLINE_CURVE ( ( 1.000000000000000000, 0.8047378541243649375, 0.8047378541243649375, 1.000000000000000000 ) ) 
 REPRESENTATION_ITEM ( '' )  );
#18514 = AXIS2_PLACEMENT_3D ( 'NONE', #14779, #26334, #21457 ) ;
#18515 = FACE_OUTER_BOUND ( 'NONE', #554, .T. ) ;
#18516 = DIRECTION ( 'NONE',  ( -1.000000000000000000, -0.000000000000000000, -0.000000000000000000 ) ) ;
#18517 = LINE ( 'NONE', #17520, #33190 ) ;
#18518 = VECTOR ( 'NONE', #44431, 1000.000000000000000 ) ;
#18519 = CARTESIAN_POINT ( 'NONE',  ( -4.999999999999948486, -204.9999999999999716, -234.7500000000000000 ) ) ;
#18520 = ORIENTED_EDGE ( 'NONE', *, *, #1141, .F. ) ;
#18521 =( BOUNDED_CURVE ( )  B_SPLINE_CURVE ( 3, ( #271, #46908, #11812, #27460 ),
 .UNSPECIFIED., .F., .F. ) 
 B_SPLINE_CURVE_WITH_KNOTS ( ( 4, 4 ),
 ( 0.000000000000000000, 1.570796326794896558 ),
 .UNSPECIFIED. ) 
 CURVE ( )  GEOMETRIC_REPRESENTATION_ITEM ( )  RATIONAL_B_SPLINE_CURVE ( ( 1.000000000000000000, 0.8047378541243649375, 0.8047378541243649375, 1.000000000000000000 ) ) 
 REPRESENTATION_ITEM ( '' )  );
#18522 = FACE_OUTER_BOUND ( 'NONE', #1094, .T. ) ;
#18523 = DIRECTION ( 'NONE',  ( 3.172065784643302499E-16, 1.000000000000000000, 0.000000000000000000 ) ) ;
#18524 = VECTOR ( 'NONE', #46468, 1000.000000000000000 ) ;
#18525 = ORIENTED_EDGE ( 'NONE', *, *, #19048, .F. ) ;
#18526 = CARTESIAN_POINT ( 'NONE',  ( 114.3291528190321173, 1.749999999999996891, 81.84341382277506227 ) ) ;
#18527 = ORIENTED_EDGE ( 'NONE', *, *, #8043, .F. ) ;
#18528 = ADVANCED_FACE ( 'NONE', ( #32180 ), #30566, .T. ) ;
#18529 = PLANE ( 'NONE',  #22960 ) ;
#18530 = CARTESIAN_POINT ( 'NONE',  ( 0.000000000000000000, 181.0000000000000284, -356.0000000000002274 ) ) ;
#18531 = CARTESIAN_POINT ( 'NONE',  ( 0.000000000000000000, 23.48684210526316107, 0.000000000000000000 ) ) ;
#18532 = EDGE_LOOP ( 'NONE', ( #48537, #4391, #41619, #978 ) ) ;
#18533 = VECTOR ( 'NONE', #37771, 1000.000000000000000 ) ;
#18534 = CARTESIAN_POINT ( 'NONE',  ( -1.153670525509249423, -0.4304314044324315525, 9.975326647350897247 ) ) ;
#18535 = VERTEX_POINT ( 'NONE', #5468 ) ;
#18536 = FACE_OUTER_BOUND ( 'NONE', #28427, .T. ) ;
#18537 = AXIS2_PLACEMENT_3D ( 'NONE', #28802, #41102, #9296 ) ;
#18538 = CARTESIAN_POINT ( 'NONE',  ( -1.468713901642213493, -0.3220470327672489419, 9.927319414211227766 ) ) ;
#18539 = CARTESIAN_POINT ( 'NONE',  ( -48.44597344681495343, 0.000000000000000000, -37.43171244307200141 ) ) ;
#18540 = ORIENTED_EDGE ( 'NONE', *, *, #43072, .T. ) ;
#18541 = ORIENTED_EDGE ( 'NONE', *, *, #4808, .F. ) ;
#18542 = CARTESIAN_POINT ( 'NONE',  ( -0.8510287611193614321, -1.787020300838985110, 9.897807938190497978 ) ) ;
#18543 = B_SPLINE_CURVE_WITH_KNOTS ( 'NONE', 3,
 ( #5309, #25073, #20968, #36653 ),
 .UNSPECIFIED., .F., .F.,
 ( 4, 4 ),
 ( 0.000000000000000000, 0.0002610106747150240823 ),
 .UNSPECIFIED. ) ;
#18544 = CARTESIAN_POINT ( 'NONE',  ( 185.0000000000000284, -180.9999999999999716, -115.0000000000001563 ) ) ;
#18545 = AXIS2_PLACEMENT_3D ( 'NONE', #35, #34944, #4865 ) ;
#18546 = EDGE_LOOP ( 'NONE', ( #768, #40085, #46446, #44777 ) ) ;
#18547 = ORIENTED_EDGE ( 'NONE', *, *, #22703, .T. ) ;
#18548 = LINE ( 'NONE', #26513, #5431 ) ;
#18549 = FACE_OUTER_BOUND ( 'NONE', #45642, .T. ) ;
#18550 = VECTOR ( 'NONE', #5837, 1000.000000000000000 ) ;
#18551 = AXIS2_PLACEMENT_3D ( 'NONE', #40177, #5012, #1681 ) ;
#18552 = ORIENTED_EDGE ( 'NONE', *, *, #49599, .F. ) ;
#18553 = CARTESIAN_POINT ( 'NONE',  ( -1.011271242968688533, 0.7347315653655859258, 10.00000000000000000 ) ) ;
#18554 = ORIENTED_EDGE ( 'NONE', *, *, #47784, .T. ) ;
#18555 = VECTOR ( 'NONE', #22782, 1000.000000000000000 ) ;
#18556 = DIRECTION ( 'NONE',  ( -1.000000000000000000, -0.000000000000000000, -0.000000000000000000 ) ) ;
#18557 = CARTESIAN_POINT ( 'NONE',  ( 1.158497635116737312, -16.61944452314319420, -3.546734833711462365 ) ) ;
#18558 = VERTEX_POINT ( 'NONE', #36800 ) ;
#18559 = ORIENTED_EDGE ( 'NONE', *, *, #40872, .F. ) ;
#18560 = ORIENTED_EDGE ( 'NONE', *, *, #134, .F. ) ;
#18561 = DIRECTION ( 'NONE',  ( -7.793956916774525800E-48, 0.000000000000000000, -1.000000000000000000 ) ) ;
#18562 = DIRECTION ( 'NONE',  ( -0.000000000000000000, -0.000000000000000000, -1.000000000000000000 ) ) ;
#18563 = VERTEX_POINT ( 'NONE', #40130 ) ;
#18564 = DIRECTION ( 'NONE',  ( -0.000000000000000000, -1.000000000000000000, -0.000000000000000000 ) ) ;
#18565 = ORIENTED_EDGE ( 'NONE', *, *, #18075, .T. ) ;
#18566 = FACE_OUTER_BOUND ( 'NONE', #40691, .T. ) ;
#18567 =( NAMED_UNIT ( * ) PLANE_ANGLE_UNIT ( ) SI_UNIT ( $, .RADIAN. ) );
#18568 = EDGE_LOOP ( 'NONE', ( #771, #716, #47779, #5659 ) ) ;
#18569 = CARTESIAN_POINT ( 'NONE',  ( -34.95136153415531766, 36.40974830873496870, 8.356839323120299312 ) ) ;
#18570 = LINE ( 'NONE', #49080, #23586 ) ;
#18571 = CARTESIAN_POINT ( 'NONE',  ( 23.26005729352310425, 44.90397804740356236, 7.906207997025717304 ) ) ;
#18572 = DIRECTION ( 'NONE',  ( 0.000000000000000000, 0.000000000000000000, 1.000000000000000000 ) ) ;
#18573 = AXIS2_PLACEMENT_3D ( 'NONE', #29236, #9723, #14075 ) ;
#18574 = CARTESIAN_POINT ( 'NONE',  ( 30.00000000000187228, 17.00000000000000000, 90.00000000000000000 ) ) ;
#18575 = VERTEX_POINT ( 'NONE', #5973 ) ;
#18576 = DIRECTION ( 'NONE',  ( 0.000000000000000000, 0.000000000000000000, -1.000000000000000000 ) ) ;
#18577 = FACE_OUTER_BOUND ( 'NONE', #25989, .T. ) ;
#18578 = DIRECTION ( 'NONE',  ( -0.000000000000000000, -0.000000000000000000, -1.000000000000000000 ) ) ;
#18579 = DIRECTION ( 'NONE',  ( -0.000000000000000000, -0.000000000000000000, -1.000000000000000000 ) ) ;
#18580 = EDGE_CURVE ( 'NONE', #39210, #10318, #48786, .T. ) ;
#18581 = CARTESIAN_POINT ( 'NONE',  ( 0.1287570809895604018, 0.3962735484563146282, 10.00000000000000000 ) ) ;
#18582 = DIRECTION ( 'NONE',  ( -1.000000000000000000, -0.000000000000000000, -0.000000000000000000 ) ) ;
#18583 = EDGE_CURVE ( 'NONE', #39773, #8719, #9815, .T. ) ;
#18584 = DIRECTION ( 'NONE',  ( 0.000000000000000000, 0.000000000000000000, -1.000000000000000000 ) ) ;
#18585 = CARTESIAN_POINT ( 'NONE',  ( 0.6126904405382156416, 1.085824959725723016, 9.981352469109932457 ) ) ;
#18586 = ADVANCED_FACE ( 'NONE', ( #21623 ), #17021, .T. ) ;
#18587 = CIRCLE ( 'NONE', #31745, 2.000000000000001776 ) ;
#18588 = ORIENTED_EDGE ( 'NONE', *, *, #33547, .T. ) ;
#18589 = ADVANCED_FACE ( 'NONE', ( #48274 ), #13674, .F. ) ;
#18590 = CARTESIAN_POINT ( 'NONE',  ( 13.59579750444771307, -10.60877755095900632, 8.727788335465566760 ) ) ;
#18591 = DIRECTION ( 'NONE',  ( -0.000000000000000000, -0.000000000000000000, 1.000000000000000000 ) ) ;
#18592 = CARTESIAN_POINT ( 'NONE',  ( -14.99999999999937472, 17.00000000000000000, -54.99999999999999289 ) ) ;
#18593 = EDGE_CURVE ( 'NONE', #13052, #48164, #18885, .T. ) ;
#18594 = ORIENTED_EDGE ( 'NONE', *, *, #25665, .T. ) ;
#18595 = ORIENTED_EDGE ( 'NONE', *, *, #20982, .F. ) ;
#18596 = CARTESIAN_POINT ( 'NONE',  ( 14.49999999999999822, 12.98684210526315930, 19.37312575500900280 ) ) ;
#18597 = CARTESIAN_POINT ( 'NONE',  ( -2.961022939495062900, 16.59676755884084187, 2.590526750877053086 ) ) ;
#18598 = EDGE_CURVE ( 'NONE', #34262, #41902, #43819, .T. ) ;
#18599 = AXIS2_PLACEMENT_3D ( 'NONE', #15616, #34883, #27422 ) ;
#18600 = VERTEX_POINT ( 'NONE', #49024 ) ;
#18601 = FACE_OUTER_BOUND ( 'NONE', #31488, .T. ) ;
#18602 = CARTESIAN_POINT ( 'NONE',  ( -204.9459734468149747, 0.000000000000000000, 162.5682875569279702 ) ) ;
#18603 = CARTESIAN_POINT ( 'NONE',  ( -86.69597344681496054, 0.000000000000000000, 165.0000000000000000 ) ) ;
#18604 = ORIENTED_EDGE ( 'NONE', *, *, #12924, .T. ) ;
#18605 = ORIENTED_EDGE ( 'NONE', *, *, #23099, .T. ) ;
#18606 = ORIENTED_EDGE ( 'NONE', *, *, #29930, .F. ) ;
#18607 = ADVANCED_FACE ( 'NONE', ( #28825 ), #20900, .F. ) ;
#18608 = EDGE_CURVE ( 'NONE', #41044, #49858, #13907, .T. ) ;
#18609 = CARTESIAN_POINT ( 'NONE',  ( 181.0000000000000000, 175.0000000000000284, -358.0000000000001705 ) ) ;
#18610 = CARTESIAN_POINT ( 'NONE',  ( 358.0000000000001137, 181.0000000000000284, 349.9999999999998295 ) ) ;
#18611 = CARTESIAN_POINT ( 'NONE',  ( 339.9999999999999432, 181.0000000000000284, -340.0000000000001705 ) ) ;
#18612 = ADVANCED_FACE ( 'NONE', ( #40634 ), #9326, .T. ) ;
#18613 = ORIENTED_EDGE ( 'NONE', *, *, #18678, .F. ) ;
#18614 = EDGE_CURVE ( 'NONE', #17157, #32209, #11898, .T. ) ;
#18615 = CARTESIAN_POINT ( 'NONE',  ( -208.4459734468149463, 0.000000000000000000, 82.56828755692798438 ) ) ;
#18616 = CARTESIAN_POINT ( 'NONE',  ( 37.90972275097264088, 14.83505920947803070, 901.8832493327278144 ) ) ;
#18617 = CARTESIAN_POINT ( 'NONE',  ( -50.00000000000000000, 50.00000000000000000, 800.0000000000000000 ) ) ;
#18618 = ORIENTED_EDGE ( 'NONE', *, *, #50617, .F. ) ;
#18619 = ORIENTED_EDGE ( 'NONE', *, *, #10266, .T. ) ;
#18620 = DIRECTION ( 'NONE',  ( -0.000000000000000000, -0.000000000000000000, -1.000000000000000000 ) ) ;
#18621 = EDGE_CURVE ( 'NONE', #3854, #37848, #44201, .T. ) ;
#18622 = CARTESIAN_POINT ( 'NONE',  ( -126.6959734468149321, -1.749999999999997335, -119.1817124430720440 ) ) ;
#18623 = EDGE_CURVE ( 'NONE', #13304, #8209, #27462, .T. ) ;
#18624 = ORIENTED_EDGE ( 'NONE', *, *, #27807, .T. ) ;
#18625 = ORIENTED_EDGE ( 'NONE', *, *, #46179, .T. ) ;
#18626 = CYLINDRICAL_SURFACE ( 'NONE', #6961, 1.750000000000015543 ) ;
#18627 = LINE ( 'NONE', #22985, #28863 ) ;
#18628 = CARTESIAN_POINT ( 'NONE',  ( 339.9999999999998863, -174.9999999999999432, 359.9999999999998295 ) ) ;
#18629 = DIRECTION ( 'NONE',  ( 1.000000000000000000, 0.000000000000000000, 0.000000000000000000 ) ) ;
#18630 = LINE ( 'NONE', #37917, #43743 ) ;
#18631 = ORIENTED_EDGE ( 'NONE', *, *, #39994, .F. ) ;
#18632 = DIRECTION ( 'NONE',  ( 1.000000000000000000, 0.000000000000000000, -4.758098676964956461E-16 ) ) ;
#18633 = LINE ( 'NONE', #30454, #13586 ) ;
#18634 = CARTESIAN_POINT ( 'NONE',  ( -5.000000000000000000, -184.7999999999999545, -340.2000000000001592 ) ) ;
#18635 = CARTESIAN_POINT ( 'NONE',  ( 356.0000000000001137, 165.0000000000000000, 339.9999999999998295 ) ) ;
#18636 = EDGE_CURVE ( 'NONE', #2097, #23500, #48526, .T. ) ;
#18637 = LINE ( 'NONE', #42743, #49227 ) ;
#18638 = EDGE_CURVE ( 'NONE', #16975, #16858, #37056, .T. ) ;
#18639 = AXIS2_PLACEMENT_3D ( 'NONE', #5833, #17380, #30186 ) ;
#18640 = ADVANCED_FACE ( 'NONE', ( #18771 ), #14433, .F. ) ;
#18641 = DIRECTION ( 'NONE',  ( -3.172065784643302499E-16, -1.000000000000000000, 2.537652627714642000E-15 ) ) ;
#18642 = ORIENTED_EDGE ( 'NONE', *, *, #35450, .T. ) ;
#18643 = CARTESIAN_POINT ( 'NONE',  ( 12.15085308559846844, -11.68662139125803989, 2.590526750877053086 ) ) ;
#18644 = CARTESIAN_POINT ( 'NONE',  ( -37.27397286063865778, 4.111076158911805223, 7.697694107796192675 ) ) ;
#18645 = CARTESIAN_POINT ( 'NONE',  ( -124.9459734468149463, 2.143131898507847836E-16, 165.0000000000000000 ) ) ;
#18646 = EDGE_CURVE ( 'NONE', #44943, #49618, #13489, .T. ) ;
#18647 =( BOUNDED_CURVE ( )  B_SPLINE_CURVE ( 3, ( #37445, #49427, #42023, #14313 ),
 .UNSPECIFIED., .F., .F. ) 
 B_SPLINE_CURVE_WITH_KNOTS ( ( 4, 4 ),
 ( 1.570796326794896558, 3.141592653589793116 ),
 .UNSPECIFIED. ) 
 CURVE ( )  GEOMETRIC_REPRESENTATION_ITEM ( )  RATIONAL_B_SPLINE_CURVE ( ( 1.000000000000000000, 0.8047378541243649375, 0.8047378541243649375, 1.000000000000000000 ) ) 
 REPRESENTATION_ITEM ( '' )  );
#18648 = ORIENTED_EDGE ( 'NONE', *, *, #47288, .T. ) ;
#18649 = DIRECTION ( 'NONE',  ( 1.000000000000000000, 0.000000000000000000, 0.000000000000000000 ) ) ;
#18650 = CARTESIAN_POINT ( 'NONE',  ( 356.0000000000000000, -167.0000000000001137, -342.0000000000003411 ) ) ;
#18651 = VERTEX_POINT ( 'NONE', #34450 ) ;
#18652 = CARTESIAN_POINT ( 'NONE',  ( 166.9999999999999716, 6.000000000000060396, 339.9999999999998295 ) ) ;
#18653 = CARTESIAN_POINT ( 'NONE',  ( -19.99999999999940670, 16.00000000000000000, -30.00000000000000000 ) ) ;
#18654 = CARTESIAN_POINT ( 'NONE',  ( -0.3862712429686809279, -1.188820645368942941, 9.972675548442463622 ) ) ;
#18655 = CARTESIAN_POINT ( 'NONE',  ( 164.9999999999999716, 17.00000000000000000, 29.99999999999999289 ) ) ;
#18656 =( BOUNDED_CURVE ( )  B_SPLINE_CURVE ( 3, ( #14740, #25790, #49087, #41941 ),
 .UNSPECIFIED., .F., .F. ) 
 B_SPLINE_CURVE_WITH_KNOTS ( ( 4, 4 ),
 ( 3.141592653589793116, 4.712388980384689674 ),
 .UNSPECIFIED. ) 
 CURVE ( )  GEOMETRIC_REPRESENTATION_ITEM ( )  RATIONAL_B_SPLINE_CURVE ( ( 1.000000000000000000, 0.8047378541243649375, 0.8047378541243649375, 1.000000000000000000 ) ) 
 REPRESENTATION_ITEM ( '' )  );
#18657 = CIRCLE ( 'NONE', #34253, 2.000000000000001776 ) ;
#18658 = ORIENTED_EDGE ( 'NONE', *, *, #35190, .F. ) ;
#18659 = DIRECTION ( 'NONE',  ( -0.000000000000000000, -1.000000000000000000, -0.000000000000000000 ) ) ;
#18660 = ORIENTED_EDGE ( 'NONE', *, *, #9375, .F. ) ;
#18661 = ORIENTED_EDGE ( 'NONE', *, *, #48203, .T. ) ;
#18662 = ADVANCED_FACE ( 'NONE', ( #33693 ), #10341, .T. ) ;
#18663 = CARTESIAN_POINT ( 'NONE',  ( -210.0000000000000568, 0.000000000000000000, -37.43171244307202272 ) ) ;
#18664 = ORIENTED_EDGE ( 'NONE', *, *, #21142, .T. ) ;
#18665 = DIRECTION ( 'NONE',  ( 0.000000000000000000, 0.000000000000000000, 1.000000000000000000 ) ) ;
#18666 = EDGE_CURVE ( 'NONE', #25205, #28949, #45764, .T. ) ;
#18667 = LINE ( 'NONE', #26637, #20419 ) ;
#18668 = LINE ( 'NONE', #150, #6763 ) ;
#18669 =( BOUNDED_CURVE ( )  B_SPLINE_CURVE ( 3, ( #22785, #38462, #46604, #27152 ),
 .UNSPECIFIED., .F., .F. ) 
 B_SPLINE_CURVE_WITH_KNOTS ( ( 4, 4 ),
 ( 4.712388980384689674, 6.283185307179586232 ),
 .UNSPECIFIED. ) 
 CURVE ( )  GEOMETRIC_REPRESENTATION_ITEM ( )  RATIONAL_B_SPLINE_CURVE ( ( 1.000000000000000000, 0.8047378541243649375, 0.8047378541243649375, 1.000000000000000000 ) ) 
 REPRESENTATION_ITEM ( '' )  );
#18670 = PLANE ( 'NONE',  #16967 ) ;
#18671 = ORIENTED_EDGE ( 'NONE', *, *, #12661, .F. ) ;
#18672 = CARTESIAN_POINT ( 'NONE',  ( 85.00000000000090949, 16.00000000000000000, -24.99999999999999289 ) ) ;
#18673 = CARTESIAN_POINT ( 'NONE',  ( 0.000000000000000000, 13.98684210526316107, -4.250000000000000000 ) ) ;
#18674 = DIRECTION ( 'NONE',  ( 0.000000000000000000, -0.000000000000000000, 1.000000000000000000 ) ) ;
#18675 = LINE ( 'NONE', #41534, #2898 ) ;
#18676 = EDGE_CURVE ( 'NONE', #46047, #27092, #18430, .T. ) ;
#18677 = EDGE_LOOP ( 'NONE', ( #38077, #22774, #31187, #33069, #50211 ) ) ;
#18678 = EDGE_CURVE ( 'NONE', #45390, #44283, #6728, .T. ) ;
#18679 = AXIS2_PLACEMENT_3D ( 'NONE', #41237, #45061, #33811 ) ;
#18680 = CARTESIAN_POINT ( 'NONE',  ( 357.1715728752537871, -167.0000000000001137, -342.0000000000003411 ) ) ;
#18681 = DIRECTION ( 'NONE',  ( -1.000000000000000000, -0.000000000000000000, -0.000000000000000000 ) ) ;
#18682 = ORIENTED_EDGE ( 'NONE', *, *, #23609, .T. ) ;
#18683 = ORIENTED_EDGE ( 'NONE', *, *, #4497, .T. ) ;
#18684 = EDGE_LOOP ( 'NONE', ( #31146, #8954, #30393, #14014 ) ) ;
#18685 = CARTESIAN_POINT ( 'NONE',  ( -14.99999999999906919, 17.00000000000000000, -24.99999999999999289 ) ) ;
#18686 = EDGE_CURVE ( 'NONE', #21143, #48323, #38049, .T. ) ;
#18687 = CARTESIAN_POINT ( 'NONE',  ( -1.011271242968693862, 0.7347315653655780432, 3.333333333333333481 ) ) ;
#18688 = ORIENTED_EDGE ( 'NONE', *, *, #13180, .T. ) ;
#18689 = EDGE_CURVE ( 'NONE', #29366, #47482, #8515, .T. ) ;
#18690 = CARTESIAN_POINT ( 'NONE',  ( 111.5540265531850679, 0.000000000000000000, 79.06828755692798438 ) ) ;
#18691 = DIRECTION ( 'NONE',  ( -1.000000000000000000, -0.000000000000000000, -0.000000000000000000 ) ) ;
#18692 = DIRECTION ( 'NONE',  ( -1.000000000000000000, 0.000000000000000000, 0.000000000000000000 ) ) ;
#18693 = FACE_OUTER_BOUND ( 'NONE', #12754, .T. ) ;
#18694 = CARTESIAN_POINT ( 'NONE',  ( 1.011271242968688311, -0.7347315653655855927, 10.00000000000000000 ) ) ;
#18695 = FACE_OUTER_BOUND ( 'NONE', #25645, .T. ) ;
#18696 = EDGE_LOOP ( 'NONE', ( #27776, #16706, #26604, #30803, #11569, #47783 ) ) ;
#18697 = FACE_OUTER_BOUND ( 'NONE', #30629, .T. ) ;
#18698 = DIRECTION ( 'NONE',  ( 0.000000000000000000, -2.265761274745217480E-16, 1.000000000000000000 ) ) ;
#18699 = EDGE_CURVE ( 'NONE', #17766, #46997, #16354, .T. ) ;
#18700 = CARTESIAN_POINT ( 'NONE',  ( -69.99999999999847944, 17.00000000000000000, 35.00000000000000000 ) ) ;
#18701 = CARTESIAN_POINT ( 'NONE',  ( 343.9999999999999432, -174.9999999999999432, 357.9999999999998295 ) ) ;
#18702 = ORIENTED_EDGE ( 'NONE', *, *, #38119, .T. ) ;
#18703 = CARTESIAN_POINT ( 'NONE',  ( 343.9999999999999432, -174.9999999999999716, 355.9999999999998295 ) ) ;
#18704 = CARTESIAN_POINT ( 'NONE',  ( 1.769963848780946369, -9.842115015280432644, 0.000000000000000000 ) ) ;
#18705 = CARTESIAN_POINT ( 'NONE',  ( 0.4166666666666669072, 0.000000000000000000, 10.00000000000000000 ) ) ;
#18706 = ORIENTED_EDGE ( 'NONE', *, *, #31217, .F. ) ;
#18707 = LINE ( 'NONE', #30280, #27265 ) ;
#18709 = ORIENTED_EDGE ( 'NONE', *, *, #27069, .F. ) ;
#18708 = VECTOR ( 'NONE', #19599, 1000.000000000000114 ) ;
#18710 = DIRECTION ( 'NONE',  ( 1.000000000000000000, 0.000000000000000000, -1.860490536778032451E-50 ) ) ;
#18711 = VERTEX_POINT ( 'NONE', #6238 ) ;
#18712 = CARTESIAN_POINT ( 'NONE',  ( -85.67084718096784002, -1.750000000000009548, -38.15658617722494483 ) ) ;
#18713 = DIRECTION ( 'NONE',  ( -1.000000000000000000, -0.000000000000000000, -0.000000000000000000 ) ) ;
#18714 = ORIENTED_EDGE ( 'NONE', *, *, #44095, .F. ) ;
#18715 = DIRECTION ( 'NONE',  ( 0.000000000000000000, 0.000000000000000000, 1.000000000000000000 ) ) ;
#18716 = ORIENTED_EDGE ( 'NONE', *, *, #9412, .F. ) ;
#18717 = CARTESIAN_POINT ( 'NONE',  ( -8.445973446814976526, 0.000000000000000000, -157.4317124430720014 ) ) ;
#18718 = ORIENTED_EDGE ( 'NONE', *, *, #3120, .F. ) ;
#18719 = CARTESIAN_POINT ( 'NONE',  ( 73.30402655318508209, 1.750000000000010658, -79.18171244307201562 ) ) ;
#18720 = PLANE ( 'NONE',  #19139 ) ;
#18721 = ORIENTED_EDGE ( 'NONE', *, *, #25549, .F. ) ;
#18722 = LINE ( 'NONE', #42339, #22107 ) ;
#18723 = CARTESIAN_POINT ( 'NONE',  ( -6.695973446814940111, 1.750000000000023759, -39.18171244307202983 ) ) ;
#18724 = B_SPLINE_CURVE_WITH_KNOTS ( 'NONE', 3,
 ( #20721, #33040, #47879, #44057 ),
 .UNSPECIFIED., .F., .F.,
 ( 4, 4 ),
 ( 0.9688112071879397824, 0.9724175925769218409 ),
 .UNSPECIFIED. ) ;
#18725 = CARTESIAN_POINT ( 'NONE',  ( -164.9999999999987779, 17.00000000000000000, 5.000000000000004441 ) ) ;
#18726 = ORIENTED_EDGE ( 'NONE', *, *, #5008, .F. ) ;
#18727 = VERTEX_POINT ( 'NONE', #45446 ) ;
#18728 = DIRECTION ( 'NONE',  ( 0.000000000000000000, 1.000000000000000000, 0.000000000000000000 ) ) ;
#18729 = DIRECTION ( 'NONE',  ( 0.000000000000000000, 0.000000000000000000, -1.000000000000000000 ) ) ;
#18730 = ADVANCED_FACE ( 'NONE', ( #15195 ), #2377, .F. ) ;
#18731 = VERTEX_POINT ( 'NONE', #18262 ) ;
#18732 = EDGE_CURVE ( 'NONE', #46541, #48958, #29782, .T. ) ;
#18733 = DIRECTION ( 'NONE',  ( -0.4740998230350175202, 0.3386427307392980146, -0.8127425537743157014 ) ) ;
#18734 = CARTESIAN_POINT ( 'NONE',  ( -9.386495789655715072, -3.489743738556220443, 6.429802539306306741 ) ) ;
#18735 = VERTEX_POINT ( 'NONE', #14162 ) ;
#18736 = CARTESIAN_POINT ( 'NONE',  ( 0.3862712429686894211, -1.188820645368940276, 9.972675548442463622 ) ) ;
#18737 = EDGE_CURVE ( 'NONE', #49396, #19482, #15717, .T. ) ;
#18738 = PLANE ( 'NONE',  #14455 ) ;
#18739 = VERTEX_POINT ( 'NONE', #18016 ) ;
#18740 = FACE_BOUND ( 'NONE', #25421, .T. ) ;
#18741 = ADVANCED_FACE ( 'NONE', ( #22131 ), #37805, .T. ) ;
#18742 = VECTOR ( 'NONE', #39182, 1000.000000000000000 ) ;
#18743 = DIRECTION ( 'NONE',  ( -0.000000000000000000, -0.000000000000000000, -1.000000000000000000 ) ) ;
#18744 = CARTESIAN_POINT ( 'NONE',  ( 155.0540265531850537, 2.143131898507880377E-16, -117.4317124430720725 ) ) ;
#18745 = EDGE_CURVE ( 'NONE', #9366, #24608, #34204, .T. ) ;
#18746 = DIRECTION ( 'NONE',  ( -1.000000000000000000, 0.000000000000000000, 0.000000000000000000 ) ) ;
#18747 = VECTOR ( 'NONE', #8772, 1000.000000000000000 ) ;
#18748 = EDGE_LOOP ( 'NONE', ( #41457, #35199, #12238, #18554 ) ) ;
#18749 =( BOUNDED_CURVE ( )  B_SPLINE_CURVE ( 3, ( #12153, #43438, #44188, #28052 ),
 .UNSPECIFIED., .F., .F. ) 
 B_SPLINE_CURVE_WITH_KNOTS ( ( 4, 4 ),
 ( 1.586958686267291678E-16, 1.570796326794889675 ),
 .UNSPECIFIED. ) 
 CURVE ( )  GEOMETRIC_REPRESENTATION_ITEM ( )  RATIONAL_B_SPLINE_CURVE ( ( 1.000000000000000000, 0.8047378541243667138, 0.8047378541243667138, 1.000000000000000000 ) ) 
 REPRESENTATION_ITEM ( '' )  );
#18750 = FACE_OUTER_BOUND ( 'NONE', #6355, .T. ) ;
#18751 = CIRCLE ( 'NONE', #38457, 1.750000000000008438 ) ;
#18752 = CARTESIAN_POINT ( 'NONE',  ( -26.18032376592659105, 21.95228666728381128, 7.455576670931136185 ) ) ;
#18753 = ADVANCED_FACE ( 'NONE', ( #570 ), #47210, .F. ) ;
#18754 = CARTESIAN_POINT ( 'NONE',  ( 1.011271242968677653, 0.7347315653656002477, -10.00000000000000000 ) ) ;
#18755 = AXIS2_PLACEMENT_3D ( 'NONE', #23886, #27983, #36208 ) ;
#18756 = ORIENTED_EDGE ( 'NONE', *, *, #37053, .F. ) ;
#18757 = EDGE_LOOP ( 'NONE', ( #43717, #33894, #24806 ) ) ;
#18758 =( LENGTH_UNIT ( ) NAMED_UNIT ( * ) SI_UNIT ( .MILLI., .METRE. ) );
#18760 = LINE ( 'NONE', #10330, #17125 ) ;
#18759 = VECTOR ( 'NONE', #332, 1000.000000000000000 ) ;
#18761 = CARTESIAN_POINT ( 'NONE',  ( 168.9999999999997158, -164.9999999999999432, 359.9999999999997726 ) ) ;
#18762 = LINE ( 'NONE', #6465, #29149 ) ;
#18763 = LINE ( 'NONE', #34444, #37381 ) ;
#18764 = FACE_OUTER_BOUND ( 'NONE', #30410, .T. ) ;
#18765 =( REPRESENTATION_RELATIONSHIP ('NONE','NONE', #3157, #35275 ) REPRESENTATION_RELATIONSHIP_WITH_TRANSFORMATION ( #30265 )SHAPE_REPRESENTATION_RELATIONSHIP( ) );
#18766 = PLANE ( 'NONE',  #42012 ) ;
#18767 = ORIENTED_EDGE ( 'NONE', *, *, #6251, .T. ) ;
#18768 = CARTESIAN_POINT ( 'NONE',  ( 30.21887974406487487, -14.69854701517530060, -8.016098858316199838 ) ) ;
#18769 = B_SPLINE_SURFACE_WITH_KNOTS ( 'NONE', 3, 3, ( 
 ( #23016, #34585, #3259, #30739 ),
 ( #46346, #30999, #11240, #42513 ),
 ( #34090, #49916, #3011, #7391 ),
 ( #2758, #11486, #7133, #14820 ) ),
 .UNSPECIFIED., .F., .F., .F.,
 ( 4, 4 ),
 ( 4, 4 ),
 ( 0.000000000000000000, 1.000000000000000000 ),
 ( 0.000000000000000000, 1.000000000000000000 ),
 .UNSPECIFIED. ) ;
#18770 = CARTESIAN_POINT ( 'NONE',  ( -48.99656738986512039, 11.00747004110376182, 1.847720168420772691 ) ) ;
#18771 = FACE_OUTER_BOUND ( 'NONE', #27969, .T. ) ;
#18772 = ORIENTED_EDGE ( 'NONE', *, *, #32419, .F. ) ;
#18773 = LINE ( 'NONE', #38315, #48238 ) ;
#18774 = ORIENTED_EDGE ( 'NONE', *, *, #12370, .F. ) ;
#18775 = CYLINDRICAL_SURFACE ( 'NONE', #8194, 1.750000000000001554 ) ;
#18776 = LINE ( 'NONE', #2625, #24953 ) ;
#18777 = FACE_OUTER_BOUND ( 'NONE', #23858, .T. ) ;
#18778 = EDGE_LOOP ( 'NONE', ( #23293, #43419, #34879, #36645 ) ) ;
#18779 = EDGE_CURVE ( 'NONE', #20500, #43501, #817, .T. ) ;
#18780 = AXIS2_PLACEMENT_3D ( 'NONE', #28521, #8522, #44636 ) ;
#18781 = VECTOR ( 'NONE', #10578, 1000.000000000000114 ) ;
#18782 = CARTESIAN_POINT ( 'NONE',  ( 151.5540265531850537, 1.025126265847089213, -0.9317124430720324924 ) ) ;
#18783 = EDGE_LOOP ( 'NONE', ( #32107, #7019, #3751, #23623, #35278, #36588, #37252, #33726 ) ) ;
#18784 = CARTESIAN_POINT ( 'NONE',  ( -0.3862712429686977478, 1.188820645368937390, -10.00000000000000000 ) ) ;
#18785 = DIRECTION ( 'NONE',  ( 1.000000000000000000, -0.000000000000000000, -0.000000000000000000 ) ) ;
#18786 = MECHANICAL_DESIGN_GEOMETRIC_PRESENTATION_REPRESENTATION (  '', ( #12248 ), #4048 ) ;
#18787 = CARTESIAN_POINT ( 'NONE',  ( -10.00000000000000000, 0.000000000000000000, 10.00000000000000000 ) ) ;
#18788 = ORIENTED_EDGE ( 'NONE', *, *, #41944, .F. ) ;
#18789 = EDGE_LOOP ( 'NONE', ( #39896, #44286, #29870, #31967, #28496, #24131, #31095, #50347 ) ) ;
#18790 = DIRECTION ( 'NONE',  ( 0.000000000000000000, 0.000000000000000000, 1.000000000000000000 ) ) ;
#18791 = CARTESIAN_POINT ( 'NONE',  ( 0.04754753503591857555, -0.8311582663284580175, 9.985686052694763504 ) ) ;
#18792 = VECTOR ( 'NONE', #18591, 1000.000000000000000 ) ;
#18793 = VERTEX_POINT ( 'NONE', #23399 ) ;
#18794 = ORIENTED_EDGE ( 'NONE', *, *, #10461, .F. ) ;
#18795 = CARTESIAN_POINT ( 'NONE',  ( 165.0000000000000000, -174.9999999999999716, -99.00000000000014211 ) ) ;
#18796 = LINE ( 'NONE', #34480, #38243 ) ;
#18797 = DIRECTION ( 'NONE',  ( 0.000000000000000000, 1.000000000000000000, 1.387778780781444413E-14 ) ) ;
#18798 = ORIENTED_EDGE ( 'NONE', *, *, #22749, .F. ) ;
#18799 = CARTESIAN_POINT ( 'NONE',  ( 185.0000000000000000, -268.4999999999999432, -349.9999999999999432 ) ) ;
#18800 = EDGE_LOOP ( 'NONE', ( #44279, #31453, #49755 ) ) ;
#18801 = CARTESIAN_POINT ( 'NONE',  ( -14.29087950072019098, -9.652079258044555132, 8.727788335465566760 ) ) ;
#18802 = CARTESIAN_POINT ( 'NONE',  ( -568.6915979970481203, -62.49999999999998579, -173.6700166912652890 ) ) ;
#18803 =( BOUNDED_CURVE ( )  B_SPLINE_CURVE ( 3, ( #43265, #36100, #39442, #24535 ),
 .UNSPECIFIED., .F., .F. ) 
 B_SPLINE_CURVE_WITH_KNOTS ( ( 4, 4 ),
 ( 3.141592653589793116, 4.712388980384689674 ),
 .UNSPECIFIED. ) 
 CURVE ( )  GEOMETRIC_REPRESENTATION_ITEM ( )  RATIONAL_B_SPLINE_CURVE ( ( 1.000000000000000000, 0.8047378541243649375, 0.8047378541243649375, 1.000000000000000000 ) ) 
 REPRESENTATION_ITEM ( '' )  );
#18804 = DIRECTION ( 'NONE',  ( 0.000000000000000000, 0.2223603367690619725, -0.9749645535258958384 ) ) ;
#18805 = ORIENTED_EDGE ( 'NONE', *, *, #6195, .F. ) ;
#18806 = ORIENTED_EDGE ( 'NONE', *, *, #43586, .T. ) ;
#18807 = VERTEX_POINT ( 'NONE', #42626 ) ;
#18808 = EDGE_CURVE ( 'NONE', #20022, #42350, #12094, .T. ) ;
#18809 =( BOUNDED_CURVE ( )  B_SPLINE_CURVE ( 3, ( #13253, #21213, #28918, #1727 ),
 .UNSPECIFIED., .F., .F. ) 
 B_SPLINE_CURVE_WITH_KNOTS ( ( 4, 4 ),
 ( 4.712388980384689674, 6.283185307179586232 ),
 .UNSPECIFIED. ) 
 CURVE ( )  GEOMETRIC_REPRESENTATION_ITEM ( )  RATIONAL_B_SPLINE_CURVE ( ( 1.000000000000000000, 0.8047378541243649375, 0.8047378541243649375, 1.000000000000000000 ) ) 
 REPRESENTATION_ITEM ( '' )  );
#18810 = CARTESIAN_POINT ( 'NONE',  ( -168.4459734468149463, 0.000000000000000000, -120.9317124430720156 ) ) ;
#18811 = VERTEX_POINT ( 'NONE', #43637 ) ;
#18812 = CARTESIAN_POINT ( 'NONE',  ( 168.9999999999999716, -81.49999999999995737, -115.0000000000001563 ) ) ;
#18814 = EDGE_LOOP ( 'NONE', ( #12432, #29874, #47875, #15530 ) ) ;
#18813 = VECTOR ( 'NONE', #24129, 1000.000000000000000 ) ;
#18815 = CARTESIAN_POINT ( 'NONE',  ( -44.94597344681493922, 2.143131898507880377E-16, -157.4317124430720014 ) ) ;
#18816 = SURFACE_STYLE_FILL_AREA ( #2912 ) ;
#18818 = ORIENTED_EDGE ( 'NONE', *, *, #46631, .F. ) ;
#18817 = AXIS2_PLACEMENT_3D ( 'NONE', #43840, #20249, #21007 ) ;
#18819 = CARTESIAN_POINT ( 'NONE',  ( -13.59579750444763668, 10.60877755095910935, 8.727788335465566760 ) ) ;
#18820 = CARTESIAN_POINT ( 'NONE',  ( -14.99999999999906919, 17.00000000000000000, -24.99999999999999289 ) ) ;
#18821 = CARTESIAN_POINT ( 'NONE',  ( -0.3862712429686809279, -1.188820645368943163, 3.333333333333333481 ) ) ;
#18822 = CARTESIAN_POINT ( 'NONE',  ( -4.945973446814903696, 2.143131898507912917E-16, 79.06828755692795596 ) ) ;
#18823 = VECTOR ( 'NONE', #34010, 1000.000000000000000 ) ;
#18824 = DIRECTION ( 'NONE',  ( 0.9908916497796512735, -0.000000000000000000, 0.1346615698592613375 ) ) ;
#18825 = ORIENTED_EDGE ( 'NONE', *, *, #4241, .F. ) ;
#18827 = VECTOR ( 'NONE', #2285, 1000.000000000000000 ) ;
#18826 = CARTESIAN_POINT ( 'NONE',  ( 14.49999999999999822, -3.557843729863134463, -15.59977635401528850 ) ) ;
#18828 = CARTESIAN_POINT ( 'NONE',  ( -46.69597344681494633, 0.000000000000000000, 165.0000000000000000 ) ) ;
#18829 = PLANE ( 'NONE',  #32657 ) ;
#18830 = LINE ( 'NONE', #49338, #23312 ) ;
#18831 = AXIS2_PLACEMENT_3D ( 'NONE', #38326, #10358, #3135 ) ;
#18832 = DIRECTION ( 'NONE',  ( 0.000000000000000000, 0.000000000000000000, 1.000000000000000000 ) ) ;
#18833 = DIRECTION ( 'NONE',  ( 1.000000000000000000, 0.000000000000000000, 0.000000000000000000 ) ) ;
#18834 = DIRECTION ( 'NONE',  ( 0.000000000000000000, -0.000000000000000000, -1.000000000000000000 ) ) ;
#18835 = CARTESIAN_POINT ( 'NONE',  ( 355.9999999999999432, -185.0000000000001421, -349.9999999999998863 ) ) ;
#18836 = EDGE_CURVE ( 'NONE', #40222, #21159, #5205, .T. ) ;
#18837 = EDGE_LOOP ( 'NONE', ( #2409, #35066, #18410, #49634, #22596, #39867 ) ) ;
#18838 = CARTESIAN_POINT ( 'NONE',  ( 23.29043492822826167, -24.10797434788167948, 1.847720168420772691 ) ) ;
#18839 = CARTESIAN_POINT ( 'NONE',  ( 151.5540265531850537, 0.000000000000000000, 42.56828755692798438 ) ) ;
#18840 = DIRECTION ( 'NONE',  ( 0.4740998230350171871, 0.3386427307392981256, -0.8127425537743158124 ) ) ;
#18841 = EDGE_LOOP ( 'NONE', ( #39643, #21962, #28396, #42865, #30363, #38225 ) ) ;
#18842 = ORIENTED_EDGE ( 'NONE', *, *, #18115, .T. ) ;
#18843 = VECTOR ( 'NONE', #4306, 1000.000000000000000 ) ;
#18844 = DIRECTION ( 'NONE',  ( -1.000000000000000000, -0.000000000000000000, -0.000000000000000000 ) ) ;
#18845 = CARTESIAN_POINT ( 'NONE',  ( 2.538055338523177440, 50.00000000000000711, -9.367992836599954742 ) ) ;
#18846 = AXIS2_PLACEMENT_3D ( 'NONE', #44022, #36364, #8886 ) ;
#18847 = AXIS2_PLACEMENT_3D ( 'NONE', #47972, #17469, #40575 ) ;
#18848 = EDGE_LOOP ( 'NONE', ( #28893, #45077, #49841, #34553, #12957, #30670 ) ) ;
#18849 = ORIENTED_EDGE ( 'NONE', *, *, #35288, .F. ) ;
#18850 = LINE ( 'NONE', #399, #3441 ) ;
#18851 = FACE_OUTER_BOUND ( 'NONE', #18150, .T. ) ;
#18852 = CARTESIAN_POINT ( 'NONE',  ( 210.0000000000000568, 0.000000000000000000, -157.4317124430720298 ) ) ;
#18853 = ORIENTED_EDGE ( 'NONE', *, *, #10198, .T. ) ;
#18854 = ORIENTED_EDGE ( 'NONE', *, *, #8255, .T. ) ;
#18855 = ORIENTED_EDGE ( 'NONE', *, *, #21435, .T. ) ;
#18856 = VECTOR ( 'NONE', #45858, 1000.000000000000227 ) ;
#18857 = VECTOR ( 'NONE', #29209, 1000.000000000000000 ) ;
#18858 = PLANE ( 'NONE',  #33203 ) ;
#18859 = DIRECTION ( 'NONE',  ( -1.586032880504786307E-16, 1.654361225106055350E-24, -1.000000000000000000 ) ) ;
#18860 = CARTESIAN_POINT ( 'NONE',  ( 1.370084944437007568, 0.09457992852872378065, 9.946805383069623474 ) ) ;
#18861 = VERTEX_POINT ( 'NONE', #46449 ) ;
#18862 = PLANE ( 'NONE',  #16139 ) ;
#18863 = CARTESIAN_POINT ( 'NONE',  ( 75.05402655318509630, 1.025126265847089435, -40.93171244307204404 ) ) ;
#18864 = CARTESIAN_POINT ( 'NONE',  ( -3.808200756227646089, -0.8261963378076270237, 9.741991644047246268 ) ) ;
#18865 = ORIENTED_EDGE ( 'NONE', *, *, #32958, .F. ) ;
#18866 = ORIENTED_EDGE ( 'NONE', *, *, #12308, .F. ) ;
#18867 = DIRECTION ( 'NONE',  ( -0.000000000000000000, 0.000000000000000000, 1.000000000000000000 ) ) ;
#18868 = EDGE_CURVE ( 'NONE', #715, #48113, #32271, .T. ) ;
#18869 = CARTESIAN_POINT ( 'NONE',  ( -48.44597344681495343, 0.000000000000000000, 159.0682875569279702 ) ) ;
#18870 = B_SPLINE_CURVE_WITH_KNOTS ( 'NONE', 3,
 ( #24440, #48230, #47981, #13120 ),
 .UNSPECIFIED., .F., .F.,
 ( 4, 4 ),
 ( 5.641302087653063738E-05, 0.0003272669002613203459 ),
 .UNSPECIFIED. ) ;
#18871 = CARTESIAN_POINT ( 'NONE',  ( 355.9999999999999432, -183.0000000000000000, 357.9999999999998295 ) ) ;
#18872 = VERTEX_POINT ( 'NONE', #11341 ) ;
#18873 = ORIENTED_EDGE ( 'NONE', *, *, #42429, .F. ) ;
#18874 = CARTESIAN_POINT ( 'NONE',  ( 30.12518629743562926, 14.70074613238908157, 1.847720168420772691 ) ) ;
#18875 = DIRECTION ( 'NONE',  ( -1.000000000000000000, 0.000000000000000000, 1.860490536778032451E-50 ) ) ;
#18876 = DIRECTION ( 'NONE',  ( -0.000000000000000000, 0.000000000000000000, 1.000000000000000000 ) ) ;
#18877 = DIRECTION ( 'NONE',  ( 0.000000000000000000, 0.000000000000000000, -1.000000000000000000 ) ) ;
#18878 = CARTESIAN_POINT ( 'NONE',  ( 339.9999999999999432, -181.0000000000001421, 356.0000000000000000 ) ) ;
#18879 = EDGE_LOOP ( 'NONE', ( #34853, #6116, #5968, #33037 ) ) ;
#18880 = CARTESIAN_POINT ( 'NONE',  ( 135.0000000000019043, 17.00000000000000000, 65.00000000000000000 ) ) ;
#18881 = EDGE_CURVE ( 'NONE', #22379, #48473, #31138, .T. ) ;
#18882 = LINE ( 'NONE', #46818, #48787 ) ;
#18883 = LINE ( 'NONE', #45570, #43645 ) ;
#18884 = EDGE_CURVE ( 'NONE', #29224, #48126, #39824, .T. ) ;
#18885 = B_SPLINE_CURVE_WITH_KNOTS ( 'NONE', 3,
 ( #44446, #33447, #33198, #8828 ),
 .UNSPECIFIED., .F., .F.,
 ( 4, 4 ),
 ( 0.000000000000000000, 2.647279941188469089E-05 ),
 .UNSPECIFIED. ) ;
#18886 = CARTESIAN_POINT ( 'NONE',  ( -4.353119224255007857, -9.002796955359011477, 0.000000000000000000 ) ) ;
#18887 = EDGE_CURVE ( 'NONE', #1058, #42210, #29802, .T. ) ;
#18888 = EDGE_CURVE ( 'NONE', #1022, #40841, #20051, .T. ) ;
#18889 = CARTESIAN_POINT ( 'NONE',  ( 0.3862712429686727678, 1.188820645368945605, -3.333333333333333481 ) ) ;
#18890 = VECTOR ( 'NONE', #32318, 1000.000000000000000 ) ;
#18891 = CARTESIAN_POINT ( 'NONE',  ( 341.9999999999999432, -167.8284271247463266, 342.8284271247462129 ) ) ;
#18892 = ORIENTED_EDGE ( 'NONE', *, *, #12, .T. ) ;
#18893 = CARTESIAN_POINT ( 'NONE',  ( 169.0000000000000000, -9.999999999999953815, -115.0000000000001563 ) ) ;
#18894 = CARTESIAN_POINT ( 'NONE',  ( 4.641001526964560142, 33.28196331604080171, -8.016098858316199838 ) ) ;
#18895 = CIRCLE ( 'NONE', #6644, 4.000000000000003553 ) ;
#18896 = ADVANCED_FACE ( 'NONE', ( #27505 ), #19282, .T. ) ;
#18897 = EDGE_CURVE ( 'NONE', #7763, #18861, #11043, .T. ) ;
#18898 = DIRECTION ( 'NONE',  ( 1.000000000000000000, 0.000000000000000000, 0.000000000000000000 ) ) ;
#18900 = ORIENTED_EDGE ( 'NONE', *, *, #28320, .T. ) ;
#18899 = EDGE_CURVE ( 'NONE', #19563, #34472, #35216, .T. ) ;
#18901 = DIRECTION ( 'NONE',  ( 0.000000000000000000, 0.000000000000000000, 1.000000000000000000 ) ) ;
#18902 = ADVANCED_FACE ( 'NONE', ( #8012 ), #12110, .T. ) ;
#18903 = CARTESIAN_POINT ( 'NONE',  ( -164.9459734468149463, 2.143131898507880377E-16, 122.5682875569279702 ) ) ;
#18904 = EDGE_LOOP ( 'NONE', ( #34791, #32999, #4315, #28176 ) ) ;
#18905 = CARTESIAN_POINT ( 'NONE',  ( 181.0000000000000284, -174.9999999999999716, -95.00000000000014211 ) ) ;
#18906 = CARTESIAN_POINT ( 'NONE',  ( 0.4166666666666669072, 0.000000000000000000, -10.00000000000000000 ) ) ;
#18907 = DIRECTION ( 'NONE',  ( 0.000000000000000000, 0.000000000000000000, -1.000000000000000000 ) ) ;
#18908 = CARTESIAN_POINT ( 'NONE',  ( 0.6108107228405675881, -1.056024183042613140, 9.963925895596188909 ) ) ;
#18909 = ADVANCED_FACE ( 'NONE', ( #27752 ), #318, .F. ) ;
#18910 = ORIENTED_EDGE ( 'NONE', *, *, #2270, .T. ) ;
#18911 = DIRECTION ( 'NONE',  ( -1.000000000000000000, -0.000000000000000000, -0.000000000000000000 ) ) ;
#18912 = ORIENTED_EDGE ( 'NONE', *, *, #46773, .F. ) ;
#18913 = ORIENTED_EDGE ( 'NONE', *, *, #50536, .T. ) ;
#18914 = CARTESIAN_POINT ( 'NONE',  ( -88.44597344681494633, -1.025126265847089435, -40.93171244307204404 ) ) ;
#18915 = VERTEX_POINT ( 'NONE', #9261 ) ;
#18916 = DIRECTION ( 'NONE',  ( -1.000000000000000000, -0.000000000000000000, -0.000000000000000000 ) ) ;
#18917 = DIRECTION ( 'NONE',  ( 0.000000000000000000, 1.000000000000000000, -0.000000000000000000 ) ) ;
#18918 = CARTESIAN_POINT ( 'NONE',  ( -210.0000000000000568, 2.143131898507884075E-16, 39.06828755692797728 ) ) ;
#18919 = CARTESIAN_POINT ( 'NONE',  ( 74.32915281903215998, -1.750000000000010436, 79.79316129108087807 ) ) ;
#18920 = ADVANCED_FACE ( 'NONE', ( #37249 ), #1819, .T. ) ;
#18921 = ORIENTED_EDGE ( 'NONE', *, *, #7076, .T. ) ;
#18922 = VECTOR ( 'NONE', #18442, 1000.000000000000000 ) ;
#18923 = DIRECTION ( 'NONE',  ( 1.000000000000000000, 0.000000000000000000, 0.000000000000000000 ) ) ;
#18924 = CARTESIAN_POINT ( 'NONE',  ( -225.0000000000000568, -165.6999999999999602, 250.3600000000000136 ) ) ;
#18925 = EDGE_CURVE ( 'NONE', #15814, #22226, #5148, .T. ) ;
#18926 = ORIENTED_EDGE ( 'NONE', *, *, #19528, .F. ) ;
#18927 = ADVANCED_FACE ( 'NONE', ( #32112, #8773 ), #21308, .F. ) ;
#18928 = DIRECTION ( 'NONE',  ( 0.000000000000000000, 0.000000000000000000, 1.000000000000000000 ) ) ;
#18929 = CARTESIAN_POINT ( 'NONE',  ( -3.566525152643847285, 1.569997364305458776, 9.741991644046965604 ) ) ;
#18930 = VERTEX_POINT ( 'NONE', #9012 ) ;
#18931 = ORIENTED_EDGE ( 'NONE', *, *, #41962, .F. ) ;
#18932 = ORIENTED_EDGE ( 'NONE', *, *, #46186, .T. ) ;
#18933 = CARTESIAN_POINT ( 'NONE',  ( 17.43089236541784359, 28.36237856644539690, 3.199614146704519602 ) ) ;
#18934 = EDGE_CURVE ( 'NONE', #20319, #49361, #47120, .T. ) ;
#18935 = VECTOR ( 'NONE', #22665, 1000.000000000000000 ) ;
#18936 = DIRECTION ( 'NONE',  ( -1.000000000000000000, -0.000000000000000000, -0.000000000000000000 ) ) ;
#18937 = ORIENTED_EDGE ( 'NONE', *, *, #31719, .F. ) ;
#18938 = EDGE_CURVE ( 'NONE', #35427, #30532, #9504, .T. ) ;
#18939 = CARTESIAN_POINT ( 'NONE',  ( -214.9999999999999432, -173.0000000000000000, 112.0000000000000284 ) ) ;
#18940 = DIRECTION ( 'NONE',  ( -1.000000000000000000, 0.000000000000000000, -0.000000000000000000 ) ) ;
#18941 = CARTESIAN_POINT ( 'NONE',  ( 2.052549611693792464, -0.2039603569406628347, 9.894754715216725671 ) ) ;
#18942 = CARTESIAN_POINT ( 'NONE',  ( -8.277096487746778308, 33.14818118907697198, 7.455576670931136185 ) ) ;
#18943 = CARTESIAN_POINT ( 'NONE',  ( 153.3040265531850537, -1.750000000000010658, -79.18171244307201562 ) ) ;
#18944 = DIRECTION ( 'NONE',  ( 0.000000000000000000, 0.000000000000000000, -1.000000000000000000 ) ) ;
#18945 = CARTESIAN_POINT ( 'NONE',  ( 31.46770792452135268, -38.94077080897339727, 3.199614146704519602 ) ) ;
#18946 = DIRECTION ( 'NONE',  ( 0.000000000000000000, 8.021842663476564905E-17, 1.000000000000000000 ) ) ;
#18947 = LINE ( 'NONE', #30779, #1880 ) ;
#18948 = VERTEX_POINT ( 'NONE', #43894 ) ;
#18949 = DIRECTION ( 'NONE',  ( -0.000000000000000000, 0.000000000000000000, 1.000000000000000000 ) ) ;
#18950 =( BOUNDED_CURVE ( )  B_SPLINE_CURVE ( 3, ( #38258, #45137, #44888, #30283 ),
 .UNSPECIFIED., .F., .F. ) 
 B_SPLINE_CURVE_WITH_KNOTS ( ( 4, 4 ),
 ( 1.570796326794896558, 3.141592653589793116 ),
 .UNSPECIFIED. ) 
 CURVE ( )  GEOMETRIC_REPRESENTATION_ITEM ( )  RATIONAL_B_SPLINE_CURVE ( ( 1.000000000000000000, 0.8047378541243649375, 0.8047378541243649375, 1.000000000000000000 ) ) 
 REPRESENTATION_ITEM ( '' )  );
#18951 = LINE ( 'NONE', #50474, #41444 ) ;
#18952 = EDGE_CURVE ( 'NONE', #48473, #8241, #36480, .T. ) ;
#18953 = CARTESIAN_POINT ( 'NONE',  ( 2.707743684961791075, 37.43817128298309882, -5.338708898921614043 ) ) ;
#18954 = PLANE ( 'NONE',  #36330 ) ;
#18955 = ORIENTED_EDGE ( 'NONE', *, *, #47606, .T. ) ;
#18956 = DIRECTION ( 'NONE',  ( -0.000000000000000000, -0.000000000000000000, 1.000000000000000000 ) ) ;
#18957 = DIRECTION ( 'NONE',  ( -1.000000000000000000, -0.000000000000000000, -0.000000000000000000 ) ) ;
#18958 =( BOUNDED_CURVE ( )  B_SPLINE_CURVE ( 3, ( #6393, #26144, #6904, #41791 ),
 .UNSPECIFIED., .F., .F. ) 
 B_SPLINE_CURVE_WITH_KNOTS ( ( 4, 4 ),
 ( 3.141592653589793116, 4.712388980384689674 ),
 .UNSPECIFIED. ) 
 CURVE ( )  GEOMETRIC_REPRESENTATION_ITEM ( )  RATIONAL_B_SPLINE_CURVE ( ( 1.000000000000000000, 0.8047378541243649375, 0.8047378541243649375, 1.000000000000000000 ) ) 
 REPRESENTATION_ITEM ( '' )  );
#18959 = VECTOR ( 'NONE', #45636, 1000.000000000000114 ) ;
#18960 = CARTESIAN_POINT ( 'NONE',  ( -1.424818880981866931, 0.8247269902860274726, 9.936700280135957186 ) ) ;
#18961 = CARTESIAN_POINT ( 'NONE',  ( 195.0540265531851105, 2.143131898507880377E-16, -120.9317124430720156 ) ) ;
#18962 = ADVANCED_FACE ( 'NONE', ( #48713 ), #47963, .T. ) ;
#18963 = SURFACE_STYLE_FILL_AREA ( #49971 ) ;
#18965 = ORIENTED_EDGE ( 'NONE', *, *, #35302, .F. ) ;
#18964 = EDGE_CURVE ( 'NONE', #37517, #28949, #35378, .T. ) ;
#18966 = CARTESIAN_POINT ( 'NONE',  ( 34.32915281903212446, -1.750000000000009548, 81.84341382277507648 ) ) ;
#18967 = ADVANCED_FACE ( 'NONE', ( #44385 ), #40564, .F. ) ;
#18968 = VERTEX_POINT ( 'NONE', #41064 ) ;
#18969 = AXIS2_PLACEMENT_3D ( 'NONE', #23131, #19278, #22881 ) ;
#18970 = CARTESIAN_POINT ( 'NONE',  ( 193.3040265531851105, -1.750000000000010214, 40.81828755692798438 ) ) ;
#18971 = ORIENTED_EDGE ( 'NONE', *, *, #1470, .F. ) ;
#18972 = ADVANCED_FACE ( 'NONE', ( #40811 ), #21058, .F. ) ;
#18973 = CARTESIAN_POINT ( 'NONE',  ( -86.69597344681494633, 1.750000000000009992, 0.8182875569279768335 ) ) ;
#18974 = CARTESIAN_POINT ( 'NONE',  ( 360.0000000000001137, 181.0000000000000568, 355.9999999999998863 ) ) ;
#18975 = EDGE_CURVE ( 'NONE', #30427, #23545, #10243, .T. ) ;
#18976 =( BOUNDED_CURVE ( )  B_SPLINE_CURVE ( 3, ( #48085, #16332, #24301, #5284 ),
 .UNSPECIFIED., .F., .F. ) 
 B_SPLINE_CURVE_WITH_KNOTS ( ( 4, 4 ),
 ( 1.570796326794896558, 3.141592653589793116 ),
 .UNSPECIFIED. ) 
 CURVE ( )  GEOMETRIC_REPRESENTATION_ITEM ( )  RATIONAL_B_SPLINE_CURVE ( ( 1.000000000000000000, 0.8047378541243649375, 0.8047378541243649375, 1.000000000000000000 ) ) 
 REPRESENTATION_ITEM ( '' )  );
#18977 = ORIENTED_EDGE ( 'NONE', *, *, #1090, .F. ) ;
#18978 = LINE ( 'NONE', #19483, #38004 ) ;
#18979 = ORIENTED_EDGE ( 'NONE', *, *, #11462, .T. ) ;
#18980 = ORIENTED_EDGE ( 'NONE', *, *, #43808, .T. ) ;
#18981 = CARTESIAN_POINT ( 'NONE',  ( 210.0000000000000568, 0.000000000000000000, 80.81828755692798438 ) ) ;
#18982 = EDGE_LOOP ( 'NONE', ( #8752, #27047, #16209, #28166, #48123, #41083 ) ) ;
#18983 = CARTESIAN_POINT ( 'NONE',  ( -9.260964247899874380, 13.84230907185616744, -9.683996418299976483 ) ) ;
#18984 = CARTESIAN_POINT ( 'NONE',  ( 195.0540265531851105, 2.143131898507880377E-16, -40.93171244307202983 ) ) ;
#18985 = CARTESIAN_POINT ( 'NONE',  ( -46.69597344681494633, -1.750000000000010658, -79.18171244307201562 ) ) ;
#18986 = EDGE_LOOP ( 'NONE', ( #46496, #2379, #40893, #34735 ) ) ;
#18987 = ORIENTED_EDGE ( 'NONE', *, *, #19527, .F. ) ;
#18988 = LINE ( 'NONE', #42345, #42302 ) ;
#18989 = LINE ( 'NONE', #17555, #18195 ) ;
#18990 = EDGE_LOOP ( 'NONE', ( #30796, #20039, #40016, #38350, #15460, #47466 ) ) ;
#18991 = EDGE_CURVE ( 'NONE', #22723, #2845, #16805, .T. ) ;
#18992 = PLANE ( 'NONE',  #36609 ) ;
#18993 = CARTESIAN_POINT ( 'NONE',  ( -27.73884755486766096, 25.23502201956265978, 7.697694107796191787 ) ) ;
#18994 = ORIENTED_EDGE ( 'NONE', *, *, #41864, .F. ) ;
#18995 = CARTESIAN_POINT ( 'NONE',  ( -22.69295089195507131, -45.31600496604688999, 7.455576670931136185 ) ) ;
#18996 = AXIS2_PLACEMENT_3D ( 'NONE', #3612, #7991, #8240 ) ;
#18997 = DIRECTION ( 'NONE',  ( -1.000000000000000000, 0.000000000000000000, 0.000000000000000000 ) ) ;
#18998 = ORIENTED_EDGE ( 'NONE', *, *, #25509, .T. ) ;
#18999 = CARTESIAN_POINT ( 'NONE',  ( 6.123233995736766282E-16, 23.48684210526316107, 5.000000000000000000 ) ) ;
#19000 = CYLINDRICAL_SURFACE ( 'NONE', #34790, 1.750000000000001554 ) ;
#19001 = LINE ( 'NONE', #11320, #17276 ) ;
#19002 = CARTESIAN_POINT ( 'NONE',  ( -88.44597344681494633, 1.025126265847089435, 39.06828755692797728 ) ) ;
#19003 = VECTOR ( 'NONE', #27970, 1000.000000000000000 ) ;
#19004 = ORIENTED_EDGE ( 'NONE', *, *, #28164, .T. ) ;
#19005 = DIRECTION ( 'NONE',  ( -1.000000000000000000, 3.172065799423185948E-16, -1.587271980518778491E-16 ) ) ;
#19006 = DIRECTION ( 'NONE',  ( 0.000000000000000000, 0.000000000000000000, -1.000000000000000000 ) ) ;
#19007 = EDGE_CURVE ( 'NONE', #37345, #44491, #32881, .T. ) ;
#19008 = CARTESIAN_POINT ( 'NONE',  ( 45.64490844644691236, 21.32281559348795952, 8.807470649214879543 ) ) ;
#19009 = ORIENTED_EDGE ( 'NONE', *, *, #6200, .T. ) ;
#19010 = EDGE_LOOP ( 'NONE', ( #26034, #48808 ) ) ;
#19011 = CARTESIAN_POINT ( 'NONE',  ( 115.0540265531850395, -1.025126265847081664, 122.5682875569279702 ) ) ;
#19012 = CARTESIAN_POINT ( 'NONE',  ( 1.780619886013945052, 1.041246721325614466, 9.886433018048068178 ) ) ;
#19013 = CARTESIAN_POINT ( 'NONE',  ( -5.880994916442842779, -0.9650022442184716942, 5.692061405548898279E-16 ) ) ;
#19014 = CARTESIAN_POINT ( 'NONE',  ( -4.999999999999995559, 197.4999999999999432, -228.6347188485896140 ) ) ;
#19015 = DIRECTION ( 'NONE',  ( 0.000000000000000000, 0.000000000000000000, -1.000000000000000000 ) ) ;
#19016 = ADVANCED_FACE ( 'NONE', ( #25166 ), #1063, .F. ) ;
#19017 = CARTESIAN_POINT ( 'NONE',  ( 113.3040265531850537, 0.000000000000000000, 165.0000000000000000 ) ) ;
#19018 = VERTEX_POINT ( 'NONE', #13350 ) ;
#19019 = CARTESIAN_POINT ( 'NONE',  ( 14.91630425054810161, -7.943683830272122215, -9.008049429158100807 ) ) ;
#19020 = AXIS2_PLACEMENT_3D ( 'NONE', #34481, #23167, #42401 ) ;
#19021 = CARTESIAN_POINT ( 'NONE',  ( -30.87089393895367095, 12.69923079256638587, -9.367992836599954742 ) ) ;
#19022 = CARTESIAN_POINT ( 'NONE',  ( -166.6959734468149463, -1.750000000000010658, -79.18171244307201562 ) ) ;
#19023 = ADVANCED_FACE ( 'NONE', ( #29013 ), #11737, .T. ) ;
#19024 = CARTESIAN_POINT ( 'NONE',  ( -168.4459734468149463, 0.000000000000000000, 82.56828755692798438 ) ) ;
#19025 = EDGE_CURVE ( 'NONE', #16759, #40675, #46309, .T. ) ;
#19026 = VERTEX_POINT ( 'NONE', #25676 ) ;
#19027 = CARTESIAN_POINT ( 'NONE',  ( -9.999626982420839028, -0.09954095390202467863, 8.968381510274571866 ) ) ;
#19028 = VECTOR ( 'NONE', #45054, 1000.000000000000000 ) ;
#19029 = FACE_OUTER_BOUND ( 'NONE', #22291, .T. ) ;
#19030 = B_SPLINE_CURVE_WITH_KNOTS ( 'NONE', 3,
 ( #18319, #46258, #10635, #34003 ),
 .UNSPECIFIED., .F., .F.,
 ( 4, 4 ),
 ( 0.001403500796105015694, 0.001586656765098967562 ),
 .UNSPECIFIED. ) ;
#19031 = ORIENTED_EDGE ( 'NONE', *, *, #34465, .F. ) ;
#19032 = DIRECTION ( 'NONE',  ( -1.000000000000000000, -0.000000000000000000, -0.000000000000000000 ) ) ;
#19033 = VECTOR ( 'NONE', #37595, 1000.000000000000000 ) ;
#19034 = CARTESIAN_POINT ( 'NONE',  ( 183.0000000000000000, 165.0000000000000000, -356.0000000000001705 ) ) ;
#19035 = EDGE_CURVE ( 'NONE', #2059, #1045, #22063, .T. ) ;
#19036 = CARTESIAN_POINT ( 'NONE',  ( -44.94597344681493922, 1.025126265847089435, 159.0682875569279418 ) ) ;
#19037 = EDGE_LOOP ( 'NONE', ( #49117, #3508, #10419 ) ) ;
#19038 =( GEOMETRIC_REPRESENTATION_CONTEXT ( 3 ) GLOBAL_UNCERTAINTY_ASSIGNED_CONTEXT ( ( #19398 ) ) GLOBAL_UNIT_ASSIGNED_CONTEXT ( ( #22317, #46400, #26419 ) ) REPRESENTATION_CONTEXT ( 'NONE', 'WORKASPACE' ) );
#19039 = ADVANCED_FACE ( 'NONE', ( #10763 ), #25932, .T. ) ;
#19040 = EDGE_CURVE ( 'NONE', #25169, #12217, #31648, .T. ) ;
#19041 = CYLINDRICAL_SURFACE ( 'NONE', #40109, 2.000000000000001776 ) ;
#19042 = AXIS2_PLACEMENT_3D ( 'NONE', #26710, #29106, #44726 ) ;
#19043 = DIRECTION ( 'NONE',  ( 0.000000000000000000, 0.000000000000000000, -1.000000000000000000 ) ) ;
#19044 = ORIENTED_EDGE ( 'NONE', *, *, #30270, .F. ) ;
#19045 = CARTESIAN_POINT ( 'NONE',  ( 210.0000000000000568, 0.000000000000000000, -37.43171244307202272 ) ) ;
#19046 = CARTESIAN_POINT ( 'NONE',  ( 168.9999999999999716, 175.0000000000000284, -340.0000000000001137 ) ) ;
#19047 = CARTESIAN_POINT ( 'NONE',  ( -44.25629667545849344, -43.33333333333336412, 790.0000000000000000 ) ) ;
#19048 = EDGE_CURVE ( 'NONE', #18915, #9595, #13736, .T. ) ;
#19049 = VERTEX_POINT ( 'NONE', #26680 ) ;
#19050 = ORIENTED_EDGE ( 'NONE', *, *, #23298, .F. ) ;
#19051 = LINE ( 'NONE', #34737, #15285 ) ;
#19052 = CARTESIAN_POINT ( 'NONE',  ( -124.9459734468149463, 2.143131898507847836E-16, -80.93171244307201562 ) ) ;
#19053 = VERTEX_POINT ( 'NONE', #45885 ) ;
#19054 = ORIENTED_EDGE ( 'NONE', *, *, #30867, .F. ) ;
#19055 = CARTESIAN_POINT ( 'NONE',  ( -204.9459734468149463, 2.143131898507880377E-16, 119.0682875569279702 ) ) ;
#19056 = DIRECTION ( 'NONE',  ( -0.000000000000000000, -0.000000000000000000, -1.000000000000000000 ) ) ;
#19057 = CARTESIAN_POINT ( 'NONE',  ( -166.6959734468149463, -1.750000000000009992, -159.1817124430720298 ) ) ;
#19058 = VERTEX_POINT ( 'NONE', #14367 ) ;
#19059 = CARTESIAN_POINT ( 'NONE',  ( -64.99999999999783995, 16.00000000000000000, 95.00000000000000000 ) ) ;
#19060 = EDGE_LOOP ( 'NONE', ( #28434, #29559, #39359, #11246, #13205, #8217, #16236, #2909, #35908, #4434 ) ) ;
#19061 = AXIS2_PLACEMENT_3D ( 'NONE', #17748, #21858, #6204 ) ;
#19062 = CARTESIAN_POINT ( 'NONE',  ( 71.55402655318506788, 0.000000000000000000, 162.5682875569279702 ) ) ;
#19063 = CARTESIAN_POINT ( 'NONE',  ( -25.63461350838931097, 43.17876197216396150, -8.016098858316205167 ) ) ;
#19064 = CARTESIAN_POINT ( 'NONE',  ( 183.0000000000000568, 165.0000000000000000, 343.9999999999998863 ) ) ;
#19065 = ORIENTED_EDGE ( 'NONE', *, *, #44400, .F. ) ;
#19066 = ORIENTED_EDGE ( 'NONE', *, *, #27908, .T. ) ;
#19067 = VERTEX_POINT ( 'NONE', #41318 ) ;
#19068 = CARTESIAN_POINT ( 'NONE',  ( 10.00000000000000000, 249.9999999999999716, 225.0000000000000000 ) ) ;
#19069 = LINE ( 'NONE', #42926, #34111 ) ;
#19070 = LINE ( 'NONE', #42416, #41250 ) ;
#19071 = EDGE_LOOP ( 'NONE', ( #35562, #43340, #44295, #13552 ) ) ;
#19072 = CARTESIAN_POINT ( 'NONE',  ( 193.3040265531851105, 1.750000000000010214, 40.81828755692798438 ) ) ;
#19073 = ORIENTED_EDGE ( 'NONE', *, *, #27060, .F. ) ;
#19075 = EDGE_CURVE ( 'NONE', #40327, #38220, #30035, .T. ) ;
#19074 = VECTOR ( 'NONE', #28397, 1000.000000000000000 ) ;
#19076 = FACE_OUTER_BOUND ( 'NONE', #30529, .T. ) ;
#19077 = ORIENTED_EDGE ( 'NONE', *, *, #23146, .F. ) ;
#19078 = CARTESIAN_POINT ( 'NONE',  ( 344.0000000000000000, 175.0000000000000284, -90.00000000000018474 ) ) ;
#19079 = CARTESIAN_POINT ( 'NONE',  ( 340.0000000000000000, -178.0000000000000284, 2.999999999999891642 ) ) ;
#19080 = CARTESIAN_POINT ( 'NONE',  ( -87.72109971266203843, 1.750000000000009548, -38.15658617722494483 ) ) ;
#19081 = DIRECTION ( 'NONE',  ( 1.000000000000000000, 0.000000000000000000, -1.132880637372608740E-16 ) ) ;
#19082 = VERTEX_POINT ( 'NONE', #10273 ) ;
#19083 = DIRECTION ( 'NONE',  ( 1.000000000000000000, 0.000000000000000000, 0.000000000000000000 ) ) ;
#19084 = DIRECTION ( 'NONE',  ( 0.000000000000000000, 1.000000000000000000, 1.544785076050074834E-48 ) ) ;
#19085 = B_SPLINE_SURFACE_WITH_KNOTS ( 'NONE', 3, 3, ( 
 ( #25416, #40563, #44384, #48953 ),
 ( #25675, #41317, #6167, #33630 ),
 ( #49217, #1567, #9260, #24916 ),
 ( #5401, #32880, #29012, #44626 ) ),
 .UNSPECIFIED., .F., .F., .F.,
 ( 4, 4 ),
 ( 4, 4 ),
 ( 0.000000000000000000, 1.000000000000000000 ),
 ( 0.000000000000000000, 1.000000000000000000 ),
 .UNSPECIFIED. ) ;
#19086 = PLANE ( 'NONE',  #48165 ) ;
#19087 = CYLINDRICAL_SURFACE ( 'NONE', #18392, 1.749999999999987566 ) ;
#19088 = ADVANCED_FACE ( 'NONE', ( #17718 ), #3063, .F. ) ;
#19089 = CARTESIAN_POINT ( 'NONE',  ( -49.89397392339119364, 8.245536726717011433, 7.906207997025717304 ) ) ;
#19090 = EDGE_CURVE ( 'NONE', #24017, #7557, #45387, .T. ) ;
#19091 = DIRECTION ( 'NONE',  ( 0.000000000000000000, -0.000000000000000000, 1.000000000000000000 ) ) ;
#19092 = ORIENTED_EDGE ( 'NONE', *, *, #11882, .F. ) ;
#19093 = CARTESIAN_POINT ( 'NONE',  ( -4.945973446814903696, 2.143131898507912917E-16, -120.9317124430720725 ) ) ;
#19094 = CYLINDRICAL_SURFACE ( 'NONE', #29575, 4.000000000000003553 ) ;
#19095 = EDGE_CURVE ( 'NONE', #44210, #2259, #1915, .T. ) ;
#19096 = ADVANCED_FACE ( 'NONE', ( #49722 ), #42065, .F. ) ;
#19097 = VERTEX_POINT ( 'NONE', #23848 ) ;
#19098 = LINE ( 'NONE', #19616, #49948 ) ;
#19099 = VECTOR ( 'NONE', #955, 999.9999999999998863 ) ;
#19100 = CARTESIAN_POINT ( 'NONE',  ( 155.0540265531850537, 2.143131898507880377E-16, 122.5682875569279702 ) ) ;
#19101 = EDGE_CURVE ( 'NONE', #5291, #18354, #257, .T. ) ;
#19102 = LINE ( 'NONE', #18592, #38123 ) ;
#19103 = AXIS2_PLACEMENT_3D ( 'NONE', #20415, #16076, #8635 ) ;
#19104 = ORIENTED_EDGE ( 'NONE', *, *, #33616, .F. ) ;
#19105 = ORIENTED_EDGE ( 'NONE', *, *, #46186, .F. ) ;
#19106 = CARTESIAN_POINT ( 'NONE',  ( 73.30402655318508209, 1.750000000000010214, 40.81828755692798438 ) ) ;
#19107 = PRESENTATION_LAYER_ASSIGNMENT (  '', '', ( #12560 ) ) ;
#19108 = CARTESIAN_POINT ( 'NONE',  ( -1.249999999999999778, 0.000000000000000000, 3.333333333333333481 ) ) ;
#19109 =( BOUNDED_CURVE ( )  B_SPLINE_CURVE ( 3, ( #22364, #22623, #29565, #41370 ),
 .UNSPECIFIED., .F., .F. ) 
 B_SPLINE_CURVE_WITH_KNOTS ( ( 4, 4 ),
 ( 3.141592653589793116, 4.712388980384689674 ),
 .UNSPECIFIED. ) 
 CURVE ( )  GEOMETRIC_REPRESENTATION_ITEM ( )  RATIONAL_B_SPLINE_CURVE ( ( 1.000000000000000000, 0.8047378541243649375, 0.8047378541243649375, 1.000000000000000000 ) ) 
 REPRESENTATION_ITEM ( '' )  );
#19110 = VERTEX_POINT ( 'NONE', #27438 ) ;
#19111 = ORIENTED_EDGE ( 'NONE', *, *, #18676, .F. ) ;
#19112 = PLANE ( 'NONE',  #4115 ) ;
#19113 = CARTESIAN_POINT ( 'NONE',  ( 13.59579750444771307, -10.60877755095900632, 8.727788335465566760 ) ) ;
#19114 = DIRECTION ( 'NONE',  ( -1.000000000000000000, -0.000000000000000000, -0.000000000000000000 ) ) ;
#19115 = VERTEX_POINT ( 'NONE', #15891 ) ;
#19116 = ORIENTED_EDGE ( 'NONE', *, *, #19075, .T. ) ;
#19117 = ORIENTED_EDGE ( 'NONE', *, *, #23784, .T. ) ;
#19118 =( BOUNDED_CURVE ( )  B_SPLINE_CURVE ( 3, ( #49147, #10693, #14032, #22252 ),
 .UNSPECIFIED., .F., .F. ) 
 B_SPLINE_CURVE_WITH_KNOTS ( ( 4, 4 ),
 ( 4.712388980384689674, 6.283185307179586232 ),
 .UNSPECIFIED. ) 
 CURVE ( )  GEOMETRIC_REPRESENTATION_ITEM ( )  RATIONAL_B_SPLINE_CURVE ( ( 1.000000000000000000, 0.8047378541243649375, 0.8047378541243649375, 1.000000000000000000 ) ) 
 REPRESENTATION_ITEM ( '' )  );
#19119 = DIRECTION ( 'NONE',  ( -0.000000000000000000, -0.000000000000000000, -1.000000000000000000 ) ) ;
#19120 = CARTESIAN_POINT ( 'NONE',  ( -124.9459734468149463, 2.143131898507847836E-16, 165.0000000000000000 ) ) ;
#19121 = B_SPLINE_CURVE_WITH_KNOTS ( 'NONE', 3,
 ( #39552, #16444, #12839, #46938 ),
 .UNSPECIFIED., .F., .F.,
 ( 4, 4 ),
 ( 1.735570302229820823E-18, 8.326314924661348653E-06 ),
 .UNSPECIFIED. ) ;
#19122 = VERTEX_POINT ( 'NONE', #50483 ) ;
#19123 = AXIS2_PLACEMENT_3D ( 'NONE', #31409, #7281, #22927 ) ;
#19124 = CARTESIAN_POINT ( 'NONE',  ( -2.538055338523177440, -33.28424297489108596, -9.367992836599954742 ) ) ;
#19125 = CARTESIAN_POINT ( 'NONE',  ( 113.3040265531850537, 0.000000000000000000, 165.0000000000000000 ) ) ;
#19126 = DIRECTION ( 'NONE',  ( -1.586032892321652236E-16, -1.000000000000000000, -2.288264760618012091E-48 ) ) ;
#19127 = VERTEX_POINT ( 'NONE', #27946 ) ;
#19128 = ORIENTED_EDGE ( 'NONE', *, *, #7987, .T. ) ;
#19129 = CARTESIAN_POINT ( 'NONE',  ( 34.32915281903212446, 1.750000000000009548, -38.15658617722494483 ) ) ;
#19130 = CARTESIAN_POINT ( 'NONE',  ( -128.4459734468149179, 0.000000000000000000, 162.5682875569279702 ) ) ;
#19131 = CARTESIAN_POINT ( 'NONE',  ( 210.0000000000000568, 0.000000000000000000, 0.8182875569279768335 ) ) ;
#19132 = EDGE_LOOP ( 'NONE', ( #27644, #24467, #41922, #50593, #34918, #10232 ) ) ;
#19133 = ORIENTED_EDGE ( 'NONE', *, *, #42278, .T. ) ;
#19134 = EDGE_CURVE ( 'NONE', #14725, #44231, #10799, .T. ) ;
#19135 = CARTESIAN_POINT ( 'NONE',  ( -210.0000000000000568, 0.000000000000000000, -119.1817124430720440 ) ) ;
#19136 = FACE_BOUND ( 'NONE', #18800, .T. ) ;
#19137 = CARTESIAN_POINT ( 'NONE',  ( 73.30402655318508209, -1.750000000000009992, -159.1817124430720298 ) ) ;
#19138 = DIRECTION ( 'NONE',  ( -0.000000000000000000, -0.000000000000000000, -1.000000000000000000 ) ) ;
#19139 = AXIS2_PLACEMENT_3D ( 'NONE', #3331, #14894, #49738 ) ;
#19140 = DIRECTION ( 'NONE',  ( -1.000000000000000000, -0.000000000000000000, -0.000000000000000000 ) ) ;
#19141 = ORIENTED_EDGE ( 'NONE', *, *, #33491, .F. ) ;
#19142 = DIRECTION ( 'NONE',  ( -1.000000000000000000, -0.000000000000000000, -0.000000000000000000 ) ) ;
#19143 = VECTOR ( 'NONE', #25104, 1000.000000000000000 ) ;
#19144 = CARTESIAN_POINT ( 'NONE',  ( -6.646097924775362209, 4.355953743238499598, 9.432811472610049819 ) ) ;
#19145 = LINE ( 'NONE', #21993, #39575 ) ;
#19146 = CARTESIAN_POINT ( 'NONE',  ( -14.99999999999937472, 16.00000000000000000, -30.00000000000000000 ) ) ;
#19147 = VECTOR ( 'NONE', #18659, 1000.000000000000000 ) ;
#19148 = AXIS2_PLACEMENT_3D ( 'NONE', #34630, #7681, #15380 ) ;
#19149 = CARTESIAN_POINT ( 'NONE',  ( 0.3862712429686727678, 1.188820645368945605, -10.00000000000000000 ) ) ;
#19150 = VERTEX_POINT ( 'NONE', #19986 ) ;
#19151 = CARTESIAN_POINT ( 'NONE',  ( 30.00000000000123279, 17.00000000000000000, 5.000000000000004441 ) ) ;
#19152 = CARTESIAN_POINT ( 'NONE',  ( 1.035950918207909632, 50.00000000000000711, -2.408242355805840784 ) ) ;
#19153 = CARTESIAN_POINT ( 'NONE',  ( 0.000000000000000000, 0.000000000000000000, 0.000000000000000000 ) ) ;
#19154 = VERTEX_POINT ( 'NONE', #23331 ) ;
#19155 = CARTESIAN_POINT ( 'NONE',  ( 112.2789002873379758, 1.749999999999996669, -78.15658617722492352 ) ) ;
#19156 = AXIS2_PLACEMENT_3D ( 'NONE', #13724, #40180, #8868 ) ;
#19157 = ORIENTED_EDGE ( 'NONE', *, *, #28787, .F. ) ;
#19158 = CARTESIAN_POINT ( 'NONE',  ( 35.00000000000122213, 17.00000000000000000, 5.000000000000004441 ) ) ;
#19159 = LINE ( 'NONE', #30994, #34490 ) ;
#19160 = EDGE_CURVE ( 'NONE', #16392, #49806, #28136, .T. ) ;
#19161 = FACE_BOUND ( 'NONE', #21587, .T. ) ;
#19162 = CARTESIAN_POINT ( 'NONE',  ( 135.0000000000019043, 17.00000000000000000, 90.00000000000000000 ) ) ;
#19163 = VERTEX_POINT ( 'NONE', #43325 ) ;
#19164 = CARTESIAN_POINT ( 'NONE',  ( -1.377509002708424468, 0.6027468487255034368, 9.927319414211229542 ) ) ;
#19165 = ORIENTED_EDGE ( 'NONE', *, *, #17752, .T. ) ;
#19166 = ORIENTED_EDGE ( 'NONE', *, *, #24632, .F. ) ;
#19167 = DIRECTION ( 'NONE',  ( 0.000000000000000000, -0.000000000000000000, 1.000000000000000000 ) ) ;
#19168 = ORIENTED_EDGE ( 'NONE', *, *, #38399, .F. ) ;
#19170 = VECTOR ( 'NONE', #49496, 1000.000000000000000 ) ;
#19169 = CARTESIAN_POINT ( 'NONE',  ( 3.231548175622897645, -9.463461120997347820, 9.282506307616472441 ) ) ;
#19171 = DIRECTION ( 'NONE',  ( -1.000000000000000000, -0.000000000000000000, -0.000000000000000000 ) ) ;
#19172 = AXIS2_PLACEMENT_3D ( 'NONE', #29660, #38389, #50115 ) ;
#19173 = UNCERTAINTY_MEASURE_WITH_UNIT (LENGTH_MEASURE( 1.000000000000000082E-05 ), #49131, 'distance_accuracy_value', 'NONE');
#19174 = CARTESIAN_POINT ( 'NONE',  ( 80.00000000000153477, 16.00000000000000000, 35.00000000000000000 ) ) ;
#19175 = VECTOR ( 'NONE', #43906, 1000.000000000000000 ) ;
#19176 = CARTESIAN_POINT ( 'NONE',  ( -177.4999999999999716, -72.50000000000001421, -130.5992382549688671 ) ) ;
#19177 = VERTEX_POINT ( 'NONE', #3831 ) ;
#19178 = AXIS2_PLACEMENT_3D ( 'NONE', #8990, #5630, #13080 ) ;
#19179 = CARTESIAN_POINT ( 'NONE',  ( -50.11058929355264979, 7.578863168071929834, 7.455576670931136185 ) ) ;
#19180 = FACE_OUTER_BOUND ( 'NONE', #8082, .T. ) ;
#19181 = CARTESIAN_POINT ( 'NONE',  ( -207.7210997126620384, -1.750000000000010214, 79.79316129108087807 ) ) ;
#19182 = ORIENTED_EDGE ( 'NONE', *, *, #28383, .T. ) ;
#19183 = CARTESIAN_POINT ( 'NONE',  ( 1.275994128725544741, -0.1230186051320594776, 9.948547179989619238 ) ) ;
#19184 = LINE ( 'NONE', #45612, #13043 ) ;
#19185 = VERTEX_POINT ( 'NONE', #30791 ) ;
#19186 = ORIENTED_EDGE ( 'NONE', *, *, #43464, .T. ) ;
#19187 = ORIENTED_EDGE ( 'NONE', *, *, #18593, .F. ) ;
#19188 = CARTESIAN_POINT ( 'NONE',  ( -10.49999999999999467, -46.12433806312137108, -6.404467680894765813 ) ) ;
#19189 = PLANE ( 'NONE',  #44650 ) ;
#19190 = ORIENTED_EDGE ( 'NONE', *, *, #4534, .T. ) ;
#19191 = CARTESIAN_POINT ( 'NONE',  ( 33.30402655318503946, -1.750000000000009992, 160.8182875569279702 ) ) ;
#19192 = LINE ( 'NONE', #43814, #6736 ) ;
#19193 = AXIS2_PLACEMENT_3D ( 'NONE', #29570, #6232, #44935 ) ;
#19194 = CARTESIAN_POINT ( 'NONE',  ( 0.4266413953668419246, 1.250184266969606162, 9.943883492372851407 ) ) ;
#19195 = FACE_OUTER_BOUND ( 'NONE', #3023, .T. ) ;
#19196 = CARTESIAN_POINT ( 'NONE',  ( -168.4459734468149747, -1.025126265847089657, 79.06828755692797017 ) ) ;
#19197 =( BOUNDED_CURVE ( )  B_SPLINE_CURVE ( 3, ( #8182, #5519, #29129, #44752 ),
 .UNSPECIFIED., .F., .F. ) 
 B_SPLINE_CURVE_WITH_KNOTS ( ( 4, 4 ),
 ( 1.570796326794896558, 3.141592653589793116 ),
 .UNSPECIFIED. ) 
 CURVE ( )  GEOMETRIC_REPRESENTATION_ITEM ( )  RATIONAL_B_SPLINE_CURVE ( ( 1.000000000000000000, 0.8047378541243649375, 0.8047378541243649375, 1.000000000000000000 ) ) 
 REPRESENTATION_ITEM ( '' )  );
#19198 = CARTESIAN_POINT ( 'NONE',  ( -1.133908876584336367, -0.5183204401656656968, 9.981352469109934233 ) ) ;
#19199 = VECTOR ( 'NONE', #22944, 1000.000000000000000 ) ;
#19200 = SURFACE_STYLE_FILL_AREA ( #42549 ) ;
#19201 = CARTESIAN_POINT ( 'NONE',  ( -4.945973446814903696, 2.143131898507912917E-16, -0.9317124430720524764 ) ) ;
#19202 = DIRECTION ( 'NONE',  ( -1.000000000000000000, -0.000000000000000000, -0.000000000000000000 ) ) ;
#19203 = ORIENTED_EDGE ( 'NONE', *, *, #44542, .T. ) ;
#19204 = CARTESIAN_POINT ( 'NONE',  ( -8.445973446814976526, 0.000000000000000000, 82.56828755692801280 ) ) ;
#19205 = FACE_OUTER_BOUND ( 'NONE', #24695, .T. ) ;
#19206 = AXIS2_PLACEMENT_3D ( 'NONE', #23929, #42909, #50571 ) ;
#19207 = CARTESIAN_POINT ( 'NONE',  ( 166.9999999999999716, 175.0000000000000284, -344.0000000000001137 ) ) ;
#19208 = DIRECTION ( 'NONE',  ( 0.000000000000000000, 8.673617379884027583E-15, -1.000000000000000000 ) ) ;
#19209 = ORIENTED_EDGE ( 'NONE', *, *, #6410, .F. ) ;
#19210 = CARTESIAN_POINT ( 'NONE',  ( -17.43089236541806031, -28.36237856644526900, 3.199614146704519602 ) ) ;
#19211 = CARTESIAN_POINT ( 'NONE',  ( -128.4459734468149179, 0.000000000000000000, -80.93171244307201562 ) ) ;
#19212 = DIRECTION ( 'NONE',  ( 0.000000000000000000, -1.000000000000000000, 0.000000000000000000 ) ) ;
#19213 = DIRECTION ( 'NONE',  ( -1.000000000000000000, -0.000000000000000000, -0.000000000000000000 ) ) ;
#19214 = VECTOR ( 'NONE', #18129, 1000.000000000000000 ) ;
#19215 = CARTESIAN_POINT ( 'NONE',  ( 47.22310614333766665, 16.46562252335956344, -3.760136334089591248 ) ) ;
#19216 = VERTEX_POINT ( 'NONE', #8202 ) ;
#19217 = FILL_AREA_STYLE_COLOUR ( '', #46882 ) ;
#19218 = ORIENTED_EDGE ( 'NONE', *, *, #43560, .F. ) ;
#19219 = EDGE_CURVE ( 'NONE', #38220, #9715, #31306, .T. ) ;
#19220 = CARTESIAN_POINT ( 'NONE',  ( 33.43156050989131955, -4.370686678976570150, 8.807470649214879543 ) ) ;
#19221 = VERTEX_POINT ( 'NONE', #35672 ) ;
#19222 = DIRECTION ( 'NONE',  ( -1.000000000000000000, 0.000000000000000000, -1.612977847700450206E-50 ) ) ;
#19223 = EDGE_CURVE ( 'NONE', #38145, #31704, #23588, .T. ) ;
#19224 = CARTESIAN_POINT ( 'NONE',  ( -54.99999999999997868, 52.49999999999999289, -5.000000000000000000 ) ) ;
#19225 = ORIENTED_EDGE ( 'NONE', *, *, #44011, .F. ) ;
#19226 = CARTESIAN_POINT ( 'NONE',  ( 168.9999999999999716, -93.49999999999998579, -340.0000000000001137 ) ) ;
#19227 = ORIENTED_EDGE ( 'NONE', *, *, #11590, .T. ) ;
#19228 = EDGE_CURVE ( 'NONE', #9206, #34485, #35053, .T. ) ;
#19229 = ADVANCED_FACE ( 'NONE', ( #11543 ), #47389, .T. ) ;
#19230 = VECTOR ( 'NONE', #49671, 1000.000000000000000 ) ;
#19231 = EDGE_LOOP ( 'NONE', ( #7719, #38778, #7927, #16794 ) ) ;
#19232 = DIRECTION ( 'NONE',  ( -0.000000000000000000, -0.000000000000000000, -1.000000000000000000 ) ) ;
#19233 = DIRECTION ( 'NONE',  ( 1.000000000000000000, 0.000000000000000000, -2.312964634635843537E-16 ) ) ;
#19234 = AXIS2_PLACEMENT_3D ( 'NONE', #10078, #2862, #50029 ) ;
#19235 = ORIENTED_EDGE ( 'NONE', *, *, #10019, .T. ) ;
#19236 = CARTESIAN_POINT ( 'NONE',  ( -1.011271242968683426, -0.7347315653655928092, 10.00000000000000000 ) ) ;
#19237 = FACE_OUTER_BOUND ( 'NONE', #23760, .T. ) ;
#19238 = CARTESIAN_POINT ( 'NONE',  ( 0.000000000000000000, 249.9999999999999716, -224.9999999999999716 ) ) ;
#19239 = ORIENTED_EDGE ( 'NONE', *, *, #8080, .F. ) ;
#19240 = ORIENTED_EDGE ( 'NONE', *, *, #44214, .T. ) ;
#19241 = CARTESIAN_POINT ( 'NONE',  ( -32.57170742938676256, -18.58316106410400437, 7.697694107796192675 ) ) ;
#19242 = DIRECTION ( 'NONE',  ( 0.000000000000000000, -0.000000000000000000, -1.000000000000000000 ) ) ;
#19243 = EDGE_LOOP ( 'NONE', ( #49046, #22638, #44862, #8063 ) ) ;
#19244 = CARTESIAN_POINT ( 'NONE',  ( -17.34922095635781147, -33.24536858281880569, 8.914903342594564961 ) ) ;
#19245 = AXIS2_PLACEMENT_3D ( 'NONE', #19443, #35124, #20447 ) ;
#19246 = CARTESIAN_POINT ( 'NONE',  ( -128.4459734468149179, 2.143131898507880377E-16, -160.9317124430720298 ) ) ;
#19247 = ORIENTED_EDGE ( 'NONE', *, *, #20175, .F. ) ;
#19248 = CARTESIAN_POINT ( 'NONE',  ( 185.0000000000000284, -9.999999999999953815, -99.00000000000014211 ) ) ;
#19249 = AXIS2_PLACEMENT_3D ( 'NONE', #15682, #12097, #46943 ) ;
#19250 = EDGE_CURVE ( 'NONE', #7557, #21400, #7690, .T. ) ;
#19251 = VERTEX_POINT ( 'NONE', #34643 ) ;
#19252 = EDGE_CURVE ( 'NONE', #26847, #27608, #17640, .T. ) ;
#19253 = VECTOR ( 'NONE', #25465, 1000.000000000000000 ) ;
#19254 = DIRECTION ( 'NONE',  ( -1.000000000000000000, -0.000000000000000000, -0.000000000000000000 ) ) ;
#19255 = CARTESIAN_POINT ( 'NONE',  ( -48.98697415750977768, -11.03699497439218291, -8.016098858316205167 ) ) ;
#19256 = DIRECTION ( 'NONE',  ( -1.000000000000000000, 0.000000000000000000, -1.612977847700450206E-50 ) ) ;
#19257 =( BOUNDED_CURVE ( )  B_SPLINE_CURVE ( 3, ( #17395, #25348, #9947, #36935 ),
 .UNSPECIFIED., .F., .F. ) 
 B_SPLINE_CURVE_WITH_KNOTS ( ( 4, 4 ),
 ( 3.141592653589793116, 4.712388980384689674 ),
 .UNSPECIFIED. ) 
 CURVE ( )  GEOMETRIC_REPRESENTATION_ITEM ( )  RATIONAL_B_SPLINE_CURVE ( ( 1.000000000000000000, 0.8047378541243649375, 0.8047378541243649375, 1.000000000000000000 ) ) 
 REPRESENTATION_ITEM ( '' )  );
#19258 = CARTESIAN_POINT ( 'NONE',  ( -84.94597344681494633, 2.143131898507880377E-16, 2.568287556927978166 ) ) ;
#19259 = EDGE_CURVE ( 'NONE', #14478, #14555, #15126, .T. ) ;
#19260 = EDGE_CURVE ( 'NONE', #23917, #39423, #11791, .T. ) ;
#19261 = ORIENTED_EDGE ( 'NONE', *, *, #12659, .F. ) ;
#19262 = DIRECTION ( 'NONE',  ( 0.000000000000000000, 0.000000000000000000, -1.000000000000000000 ) ) ;
#19263 = ADVANCED_FACE ( 'NONE', ( #19737 ), #7444, .T. ) ;
#19264 = SURFACE_STYLE_FILL_AREA ( #38033 ) ;
#19265 =( BOUNDED_CURVE ( )  B_SPLINE_CURVE ( 3, ( #19433, #39458, #23546, #8403 ),
 .UNSPECIFIED., .F., .F. ) 
 B_SPLINE_CURVE_WITH_KNOTS ( ( 4, 4 ),
 ( 3.141592653589793116, 4.712388980384689674 ),
 .UNSPECIFIED. ) 
 CURVE ( )  GEOMETRIC_REPRESENTATION_ITEM ( )  RATIONAL_B_SPLINE_CURVE ( ( 1.000000000000000000, 0.8047378541243649375, 0.8047378541243649375, 1.000000000000000000 ) ) 
 REPRESENTATION_ITEM ( '' )  );
#19266 = EDGE_CURVE ( 'NONE', #41913, #14475, #34904, .T. ) ;
#19267 = CARTESIAN_POINT ( 'NONE',  ( 14.76429217231961566, 8.192625680377691566, 9.178419661560148768 ) ) ;
#19268 = ORIENTED_EDGE ( 'NONE', *, *, #25570, .T. ) ;
#19269 = VERTEX_POINT ( 'NONE', #7950 ) ;
#19270 = DIRECTION ( 'NONE',  ( 1.000000000000000000, -1.044997421928429067E-14, -1.754668910725352053E-14 ) ) ;
#19271 = CARTESIAN_POINT ( 'NONE',  ( -119.9999999999981668, 17.00000000000000000, 65.00000000000000000 ) ) ;
#19272 = AXIS2_PLACEMENT_3D ( 'NONE', #38892, #19369, #35052 ) ;
#19273 = CARTESIAN_POINT ( 'NONE',  ( -6.695973446814940111, 1.750000000000023315, 0.8182875569279768335 ) ) ;
#19274 = LINE ( 'NONE', #11848, #45399 ) ;
#19275 = VECTOR ( 'NONE', #11723, 1000.000000000000000 ) ;
#19276 = FACE_OUTER_BOUND ( 'NONE', #25683, .T. ) ;
#19277 = ORIENTED_EDGE ( 'NONE', *, *, #35989, .T. ) ;
#19278 = DIRECTION ( 'NONE',  ( -0.000000000000000000, -0.000000000000000000, 1.000000000000000000 ) ) ;
#19279 = VECTOR ( 'NONE', #25161, 1000.000000000000114 ) ;
#19280 =( BOUNDED_CURVE ( )  B_SPLINE_CURVE ( 3, ( #22854, #30829, #42601, #11318 ),
 .UNSPECIFIED., .F., .F. ) 
 B_SPLINE_CURVE_WITH_KNOTS ( ( 4, 4 ),
 ( 4.712388980384689674, 6.283185307179586232 ),
 .UNSPECIFIED. ) 
 CURVE ( )  GEOMETRIC_REPRESENTATION_ITEM ( )  RATIONAL_B_SPLINE_CURVE ( ( 1.000000000000000000, 0.8047378541243649375, 0.8047378541243649375, 1.000000000000000000 ) ) 
 REPRESENTATION_ITEM ( '' )  );
#19281 = DIRECTION ( 'NONE',  ( -0.000000000000000000, -0.000000000000000000, -1.000000000000000000 ) ) ;
#19282 = CYLINDRICAL_SURFACE ( 'NONE', #44596, 1.750000000000001554 ) ;
#19283 = EDGE_CURVE ( 'NONE', #47848, #18060, #47646, .T. ) ;
#19284 = CARTESIAN_POINT ( 'NONE',  ( -88.44597344681497475, 0.000000000000000000, 2.568287556928006143 ) ) ;
#19285 = AXIS2_PLACEMENT_3D ( 'NONE', #10334, #33934, #13406 ) ;
#19286 = EDGE_CURVE ( 'NONE', #10859, #23653, #37011, .T. ) ;
#19287 = ORIENTED_EDGE ( 'NONE', *, *, #32868, .T. ) ;
#19288 = EDGE_CURVE ( 'NONE', #33612, #25838, #36159, .T. ) ;
#19289 = DIRECTION ( 'NONE',  ( 0.000000000000000000, 3.186989995019654210E-49, 1.000000000000000000 ) ) ;
#19290 = VECTOR ( 'NONE', #41287, 1000.000000000000000 ) ;
#19291 = DIRECTION ( 'NONE',  ( 0.000000000000000000, -1.000000000000000000, 0.000000000000000000 ) ) ;
#19292 = EDGE_LOOP ( 'NONE', ( #626, #43737, #1800, #1833 ) ) ;
#19293 = CARTESIAN_POINT ( 'NONE',  ( -114.9999999999981526, 17.00000000000000000, 65.00000000000000000 ) ) ;
#19294 = CARTESIAN_POINT ( 'NONE',  ( 210.0000000000000568, 0.000000000000000000, 0.8182875569279768335 ) ) ;
#19295 = CARTESIAN_POINT ( 'NONE',  ( 210.0000000000000568, 0.000000000000000000, -157.4317124430720298 ) ) ;
#19296 = FACE_OUTER_BOUND ( 'NONE', #14210, .T. ) ;
#19297 = VECTOR ( 'NONE', #12465, 1000.000000000000000 ) ;
#19298 = ORIENTED_EDGE ( 'NONE', *, *, #15818, .T. ) ;
#19299 = LINE ( 'NONE', #19805, #33551 ) ;
#19300 = CARTESIAN_POINT ( 'NONE',  ( -48.44597344681495343, 0.000000000000000000, 82.56828755692798438 ) ) ;
#19301 = VERTEX_POINT ( 'NONE', #40756 ) ;
#19302 = CARTESIAN_POINT ( 'NONE',  ( 344.0000000000000000, -167.0000000000001137, -342.0000000000002842 ) ) ;
#19303 = CARTESIAN_POINT ( 'NONE',  ( 33.30402655318503946, 0.000000000000000000, 165.0000000000000000 ) ) ;
#19304 = UNCERTAINTY_MEASURE_WITH_UNIT (LENGTH_MEASURE( 1.000000000000000082E-05 ), #46750, 'distance_accuracy_value', 'NONE');
#19305 = DIRECTION ( 'NONE',  ( -1.000000000000000000, -0.000000000000000000, -0.000000000000000000 ) ) ;
#19306 = ADVANCED_FACE ( 'NONE', ( #17398 ), #32817, .F. ) ;
#19307 = ORIENTED_EDGE ( 'NONE', *, *, #5775, .T. ) ;
#19308 = ORIENTED_EDGE ( 'NONE', *, *, #23170, .T. ) ;
#19309 = DIRECTION ( 'NONE',  ( 0.000000000000000000, 0.000000000000000000, -1.000000000000000000 ) ) ;
#19310 = DIRECTION ( 'NONE',  ( 1.000000000000000000, 0.000000000000000000, -4.758098676964956461E-16 ) ) ;
#19311 = AXIS2_PLACEMENT_3D ( 'NONE', #25694, #41336, #48737 ) ;
#19312 = ORIENTED_EDGE ( 'NONE', *, *, #18472, .F. ) ;
#19313 = VERTEX_POINT ( 'NONE', #1509 ) ;
#19314 = PLANE ( 'NONE',  #30699 ) ;
#19315 = DIRECTION ( 'NONE',  ( 0.000000000000000000, 1.000000000000000000, 0.000000000000000000 ) ) ;
#19316 = CARTESIAN_POINT ( 'NONE',  ( 0.000000000000000000, -180.9999999999999716, -360.0000000000002274 ) ) ;
#19317 = EDGE_CURVE ( 'NONE', #48914, #21408, #36421, .T. ) ;
#19318 = AXIS2_PLACEMENT_3D ( 'NONE', #32776, #31774, #23812 ) ;
#19319 = ORIENTED_EDGE ( 'NONE', *, *, #33414, .F. ) ;
#19320 = CARTESIAN_POINT ( 'NONE',  ( 1.011271242968688311, -0.7347315653655855927, -10.00000000000000000 ) ) ;
#19321 = ORIENTED_EDGE ( 'NONE', *, *, #24513, .F. ) ;
#19322 = AXIS2_PLACEMENT_3D ( 'NONE', #47773, #3956, #886 ) ;
#19323 = LINE ( 'NONE', #27286, #9937 ) ;
#19324 = LINE ( 'NONE', #18299, #38210 ) ;
#19326 = VECTOR ( 'NONE', #48926, 1000.000000000000000 ) ;
#19325 = CARTESIAN_POINT ( 'NONE',  ( -119.9999999999987921, 17.00000000000000000, 5.000000000000004441 ) ) ;
#19327 = EDGE_CURVE ( 'NONE', #18968, #16979, #24904, .T. ) ;
#19329 = ORIENTED_EDGE ( 'NONE', *, *, #42198, .T. ) ;
#19328 = ADVANCED_FACE ( 'NONE', ( #5588 ), #13538, .T. ) ;
#19330 = ORIENTED_EDGE ( 'NONE', *, *, #18689, .T. ) ;
#19331 = COLOUR_RGB ( '',0.7921568627450980005, 0.8196078431372548767, 0.9333333333333333481 ) ;
#19332 = ORIENTED_EDGE ( 'NONE', *, *, #44836, .T. ) ;
#19333 = CARTESIAN_POINT ( 'NONE',  ( -208.4459734468149463, 0.000000000000000000, 119.0682875569279702 ) ) ;
#19334 = CARTESIAN_POINT ( 'NONE',  ( -23.79193388295331602, -28.98609808354994044, -9.422646554964178023 ) ) ;
#19335 = EDGE_CURVE ( 'NONE', #38770, #22476, #44823, .T. ) ;
#19336 = ORIENTED_EDGE ( 'NONE', *, *, #5136, .T. ) ;
#19337 = FACE_OUTER_BOUND ( 'NONE', #21688, .T. ) ;
#19338 = ORIENTED_EDGE ( 'NONE', *, *, #3312, .T. ) ;
#19339 = AXIS2_PLACEMENT_3D ( 'NONE', #33400, #25431, #41331 ) ;
#19340 = EDGE_CURVE ( 'NONE', #11545, #16553, #16641, .T. ) ;
#19341 = FACE_OUTER_BOUND ( 'NONE', #45169, .T. ) ;
#19342 = ORIENTED_EDGE ( 'NONE', *, *, #49413, .F. ) ;
#19343 = EDGE_CURVE ( 'NONE', #23653, #37708, #48400, .T. ) ;
#19344 = CARTESIAN_POINT ( 'NONE',  ( -194.9999999999999432, -173.0000000000000000, 372.0000000000000568 ) ) ;
#19345 = PLANE ( 'NONE',  #28483 ) ;
#19346 = DIRECTION ( 'NONE',  ( -1.000000000000000000, 0.000000000000000000, 0.000000000000000000 ) ) ;
#19347 = CARTESIAN_POINT ( 'NONE',  ( 4.672045878990125800, -33.19353511768168374, 1.847720168420772691 ) ) ;
#19348 = ORIENTED_EDGE ( 'NONE', *, *, #20076, .F. ) ;
#19349 = VERTEX_POINT ( 'NONE', #28947 ) ;
#19350 = DIRECTION ( 'NONE',  ( 0.000000000000000000, -0.000000000000000000, -1.000000000000000000 ) ) ;
#19351 = CARTESIAN_POINT ( 'NONE',  ( 193.3040265531851105, -1.750000000000010214, 40.81828755692798438 ) ) ;
#19352 = EDGE_CURVE ( 'NONE', #29505, #20059, #44078, .T. ) ;
#19353 = CARTESIAN_POINT ( 'NONE',  ( -114.9999999999984652, 17.00000000000000000, 35.00000000000000000 ) ) ;
#19354 = CARTESIAN_POINT ( 'NONE',  ( 113.3040265531850537, -1.749999999999997113, 40.81828755692798438 ) ) ;
#19355 = VECTOR ( 'NONE', #1908, 1000.000000000000000 ) ;
#19356 = DIRECTION ( 'NONE',  ( 0.000000000000000000, 0.000000000000000000, 1.000000000000000000 ) ) ;
#19357 = VECTOR ( 'NONE', #43924, 1000.000000000000000 ) ;
#19358 = EDGE_CURVE ( 'NONE', #5075, #297, #48150, .T. ) ;
#19359 = VECTOR ( 'NONE', #16744, 1000.000000000000000 ) ;
#19360 = DIRECTION ( 'NONE',  ( 1.000000000000000000, 0.000000000000000000, 0.000000000000000000 ) ) ;
#19361 = ORIENTED_EDGE ( 'NONE', *, *, #24269, .T. ) ;
#19362 = CARTESIAN_POINT ( 'NONE',  ( 0.000000000000000000, 17.00000000000000000, 0.000000000000000000 ) ) ;
#19363 = CARTESIAN_POINT ( 'NONE',  ( -376.8544389702902890, 0.000000000000000000, 219.8317560660027539 ) ) ;
#19364 = ORIENTED_EDGE ( 'NONE', *, *, #7454, .T. ) ;
#19365 = AXIS2_PLACEMENT_3D ( 'NONE', #15301, #38908, #24454 ) ;
#19366 = CARTESIAN_POINT ( 'NONE',  ( 27.33593271309472073, -41.94268121623323964, -9.367992836599954742 ) ) ;
#19367 = AXIS2_PLACEMENT_3D ( 'NONE', #38236, #6911, #26667 ) ;
#19368 = CARTESIAN_POINT ( 'NONE',  ( 1.011271242968688311, -0.7347315653655855927, 3.333333333333333481 ) ) ;
#19369 = DIRECTION ( 'NONE',  ( 0.000000000000000000, -1.000000000000000000, 0.000000000000000000 ) ) ;
#19370 = EDGE_LOOP ( 'NONE', ( #34303, #29542, #10365, #8979, #37329 ) ) ;
#19371 = ORIENTED_EDGE ( 'NONE', *, *, #50234, .T. ) ;
#19372 = CARTESIAN_POINT ( 'NONE',  ( 183.0000000000000284, 2.775557561562891351E-14, -111.0000000000001563 ) ) ;
#19373 = AXIS2_PLACEMENT_3D ( 'NONE', #42842, #39028, #26707 ) ;
#19374 = CARTESIAN_POINT ( 'NONE',  ( 8.277096487746778308, -33.14818118907697198, 7.455576670931136185 ) ) ;
#19375 = ORIENTED_EDGE ( 'NONE', *, *, #18014, .T. ) ;
#19376 = ORIENTED_EDGE ( 'NONE', *, *, #4571, .T. ) ;
#19377 = DIRECTION ( 'NONE',  ( -0.000000000000000000, -0.000000000000000000, -1.000000000000000000 ) ) ;
#19378 = CARTESIAN_POINT ( 'NONE',  ( -3.996390545799824334, 16.57371371864897469, 8.953103998512858652 ) ) ;
#19379 = DIRECTION ( 'NONE',  ( -0.000000000000000000, -1.000000000000000000, -0.000000000000000000 ) ) ;
#19380 = VERTEX_POINT ( 'NONE', #12794 ) ;
#19381 = ORIENTED_EDGE ( 'NONE', *, *, #44019, .T. ) ;
#19382 = ORIENTED_EDGE ( 'NONE', *, *, #8632, .F. ) ;
#19383 = CARTESIAN_POINT ( 'NONE',  ( -19.99999999999971223, 17.00000000000000000, -84.99999999999998579 ) ) ;
#19384 = CARTESIAN_POINT ( 'NONE',  ( -84.94597344681493212, 1.025126265847089435, 159.0682875569279418 ) ) ;
#19385 = EDGE_LOOP ( 'NONE', ( #11606, #4729, #45972, #4203 ) ) ;
#19386 = EDGE_CURVE ( 'NONE', #30294, #45615, #28458, .T. ) ;
#19387 = CARTESIAN_POINT ( 'NONE',  ( 210.0000000000000568, 0.000000000000000000, -79.18171244307201562 ) ) ;
#19388 = ADVANCED_FACE ( 'NONE', ( #8946 ), #32310, .F. ) ;
#19389 = AXIS2_PLACEMENT_3D ( 'NONE', #22477, #11196, #30174 ) ;
#19390 = CARTESIAN_POINT ( 'NONE',  ( -205.6708471809678827, 1.750000000000009548, 1.843413822775065825 ) ) ;
#19391 = DIRECTION ( 'NONE',  ( -1.000000000000000000, -0.000000000000000000, -0.000000000000000000 ) ) ;
#19392 = VERTEX_POINT ( 'NONE', #20490 ) ;
#19393 = ORIENTED_EDGE ( 'NONE', *, *, #49158, .T. ) ;
#19394 = CARTESIAN_POINT ( 'NONE',  ( -5.000000000000000000, 184.8000000000000114, 359.7999999999997840 ) ) ;
#19395 = CARTESIAN_POINT ( 'NONE',  ( -124.9459734468149321, -1.025126265847081886, -120.9317124430720440 ) ) ;
#19396 = CARTESIAN_POINT ( 'NONE',  ( -84.94597344681494633, 2.143131898507880377E-16, 119.0682875569279702 ) ) ;
#19397 = EDGE_CURVE ( 'NONE', #29367, #35690, #1756, .T. ) ;
#19398 = UNCERTAINTY_MEASURE_WITH_UNIT (LENGTH_MEASURE( 1.000000000000000082E-05 ), #22317, 'distance_accuracy_value', 'NONE');
#19399 = ORIENTED_EDGE ( 'NONE', *, *, #35137, .T. ) ;
#19400 = ORIENTED_EDGE ( 'NONE', *, *, #34934, .F. ) ;
#19401 = ADVANCED_FACE ( 'NONE', ( #5079 ), #35911, .T. ) ;
#19402 = FACE_OUTER_BOUND ( 'NONE', #18374, .T. ) ;
#19403 = FILL_AREA_STYLE ('',( #16571 ) ) ;
#19404 = ORIENTED_EDGE ( 'NONE', *, *, #45385, .F. ) ;
#19405 = EDGE_CURVE ( 'NONE', #8523, #9153, #13877, .T. ) ;
#19406 = PLANE ( 'NONE',  #45162 ) ;
#19407 = CARTESIAN_POINT ( 'NONE',  ( 0.000000000000000000, 17.00000000000000000, 0.000000000000000000 ) ) ;
#19408 = CARTESIAN_POINT ( 'NONE',  ( 0.2050626648100478400, -1.807624707196173519, 9.903764339332001398 ) ) ;
#19409 = DIRECTION ( 'NONE',  ( -0.000000000000000000, -0.000000000000000000, -1.000000000000000000 ) ) ;
#19410 = EDGE_LOOP ( 'NONE', ( #45845, #28591, #29370, #7865 ) ) ;
#19411 = ADVANCED_FACE ( 'NONE', ( #41246 ), #10454, .T. ) ;
#19412 = CARTESIAN_POINT ( 'NONE',  ( -119.9999999999984652, 17.00000000000000000, 60.00000000000000000 ) ) ;
#19413 = CARTESIAN_POINT ( 'NONE',  ( 210.0000000000000568, 2.143131898507880377E-16, -0.9317124430720331585 ) ) ;
#19414 = EDGE_CURVE ( 'NONE', #50507, #10238, #41004, .T. ) ;
#19415 = B_SPLINE_CURVE_WITH_KNOTS ( 'NONE', 3,
 ( #19645, #12200, #46800, #657 ),
 .UNSPECIFIED., .F., .F.,
 ( 4, 4 ),
 ( 0.000000000000000000, 0.0004154657329505417928 ),
 .UNSPECIFIED. ) ;
#19416 = CARTESIAN_POINT ( 'NONE',  ( 79.99999999999997158, 17.00000000000000000, -114.9999999999999858 ) ) ;
#19417 = VECTOR ( 'NONE', #9157, 1000.000000000000000 ) ;
#19418 = CARTESIAN_POINT ( 'NONE',  ( 5.551115123125782702E-14, -166.9999999999999432, 343.9999999999997726 ) ) ;
#19419 = EDGE_LOOP ( 'NONE', ( #46240, #13578, #14889, #11389, #23212, #35723 ) ) ;
#19420 = DIRECTION ( 'NONE',  ( 0.000000000000000000, -0.9749645535258955054, 0.2223603367690637767 ) ) ;
#19421 = CARTESIAN_POINT ( 'NONE',  ( -49.89397392339119364, 8.245536726717011433, 7.906207997025717304 ) ) ;
#19422 = CARTESIAN_POINT ( 'NONE',  ( -167.7210997126620384, -1.750000000000009548, -160.2068387089191219 ) ) ;
#19423 = ORIENTED_EDGE ( 'NONE', *, *, #25632, .T. ) ;
#19424 = CARTESIAN_POINT ( 'NONE',  ( -6.695973446814940111, -1.750000000000023315, 160.8182875569279702 ) ) ;
#19425 = CARTESIAN_POINT ( 'NONE',  ( -177.4999999999999716, 57.49999999999996447, -9.999999999999973355 ) ) ;
#19426 = ORIENTED_EDGE ( 'NONE', *, *, #12043, .F. ) ;
#19427 = DIRECTION ( 'NONE',  ( 0.000000000000000000, 0.000000000000000000, 1.000000000000000000 ) ) ;
#19428 = CARTESIAN_POINT ( 'NONE',  ( 2.538055338523173443, 50.00000000000000711, -9.367992836599951190 ) ) ;
#19429 = PLANE ( 'NONE',  #24155 ) ;
#19430 = CARTESIAN_POINT ( 'NONE',  ( 30.00000000000153833, 16.00000000000000000, 35.00000000000000000 ) ) ;
#19431 =( BOUNDED_CURVE ( )  B_SPLINE_CURVE ( 3, ( #18723, #4369, #4111, #43602 ),
 .UNSPECIFIED., .F., .F. ) 
 B_SPLINE_CURVE_WITH_KNOTS ( ( 4, 4 ),
 ( 1.570796326794896558, 3.141592653589793116 ),
 .UNSPECIFIED. ) 
 CURVE ( )  GEOMETRIC_REPRESENTATION_ITEM ( )  RATIONAL_B_SPLINE_CURVE ( ( 1.000000000000000000, 0.8047378541243649375, 0.8047378541243649375, 1.000000000000000000 ) ) 
 REPRESENTATION_ITEM ( '' )  );
#19432 = ORIENTED_EDGE ( 'NONE', *, *, #45121, .T. ) ;
#19433 = CARTESIAN_POINT ( 'NONE',  ( -124.9459734468149463, 2.143131898507847836E-16, -37.43171244307205825 ) ) ;
#19434 = ORIENTED_EDGE ( 'NONE', *, *, #27768, .T. ) ;
#19435 = EDGE_LOOP ( 'NONE', ( #49311, #19935, #19092, #17315 ) ) ;
#19436 = ADVANCED_FACE ( 'NONE', ( #17648 ), #47771, .T. ) ;
#19437 = CARTESIAN_POINT ( 'NONE',  ( 195.0540265531851105, -1.025126265847089435, 122.5682875569280128 ) ) ;
#19438 = ORIENTED_EDGE ( 'NONE', *, *, #31542, .T. ) ;
#19439 = LINE ( 'NONE', #22778, #40160 ) ;
#19440 = DIRECTION ( 'NONE',  ( 0.000000000000000000, 0.000000000000000000, 1.000000000000000000 ) ) ;
#19441 = CARTESIAN_POINT ( 'NONE',  ( -5.647304616913629616, 295.8217383796908848, 144.9816133044550668 ) ) ;
#19442 = EDGE_LOOP ( 'NONE', ( #46230, #30645, #35717, #43100 ) ) ;
#19443 = CARTESIAN_POINT ( 'NONE',  ( -86.69597344681496054, 0.000000000000000000, 165.0000000000000000 ) ) ;
#19444 = CARTESIAN_POINT ( 'NONE',  ( -7.721099712662037540, 1.750000000000023981, 119.7931612910808781 ) ) ;
#19445 = EDGE_LOOP ( 'NONE', ( #18788, #50003 ) ) ;
#19446 = DIRECTION ( 'NONE',  ( 0.000000000000000000, 0.000000000000000000, 1.000000000000000000 ) ) ;
#19447 = CARTESIAN_POINT ( 'NONE',  ( -86.69597344681494633, 1.750000000000009992, 0.8182875569279768335 ) ) ;
#19448 = ORIENTED_EDGE ( 'NONE', *, *, #38878, .T. ) ;
#19449 = ORIENTED_EDGE ( 'NONE', *, *, #48139, .T. ) ;
#19450 = ORIENTED_EDGE ( 'NONE', *, *, #31186, .F. ) ;
#19451 = DIRECTION ( 'NONE',  ( 0.9908916497796512735, 0.000000000000000000, 0.1346615698592613375 ) ) ;
#19452 = CARTESIAN_POINT ( 'NONE',  ( -225.0000000000000568, 175.0000000000000000, 0.000000000000000000 ) ) ;
#19453 = ORIENTED_EDGE ( 'NONE', *, *, #39960, .T. ) ;
#19454 = CARTESIAN_POINT ( 'NONE',  ( -0.3862712429686809279, -1.188820645368942941, 9.972675548442463622 ) ) ;
#19455 =( NAMED_UNIT ( * ) PLANE_ANGLE_UNIT ( ) SI_UNIT ( $, .RADIAN. ) );
#19456 = CARTESIAN_POINT ( 'NONE',  ( -64.99999999999815259, 17.00000000000000000, 65.00000000000000000 ) ) ;
#19457 = CARTESIAN_POINT ( 'NONE',  ( -126.6959734468149321, 0.000000000000000000, 165.0000000000000000 ) ) ;
#19458 = LINE ( 'NONE', #34368, #10765 ) ;
#19459 = VECTOR ( 'NONE', #43255, 1000.000000000000000 ) ;
#19460 = CARTESIAN_POINT ( 'NONE',  ( 84.99999999999997158, 16.00000000000000000, -90.00000000000000000 ) ) ;
#19461 = CARTESIAN_POINT ( 'NONE',  ( -1.377594142017869450, 0.6023266041008150662, 9.944962737616616977 ) ) ;
#19462 = ADVANCED_FACE ( 'NONE', ( #49411 ), #48899, .T. ) ;
#19463 = CARTESIAN_POINT ( 'NONE',  ( 194.9999999999999432, -173.0000000000000000, 372.0000000000000568 ) ) ;
#19464 = CARTESIAN_POINT ( 'NONE',  ( -206.6959734468149463, 0.000000000000000000, 165.0000000000000000 ) ) ;
#19465 = ORIENTED_EDGE ( 'NONE', *, *, #17951, .T. ) ;
#19466 = CARTESIAN_POINT ( 'NONE',  ( 349.9999999999999432, -180.9999999999999716, 355.9999999999997726 ) ) ;
#19467 = DIRECTION ( 'NONE',  ( 0.000000000000000000, 5.664403186863042467E-17, 1.000000000000000000 ) ) ;
#19468 = CARTESIAN_POINT ( 'NONE',  ( -167.4999999999999432, 67.47808924524055385, -120.5992382549688955 ) ) ;
#19469 = CARTESIAN_POINT ( 'NONE',  ( -5.000000000000000000, -184.7999999999999545, -359.8000000000002387 ) ) ;
#19470 = ORIENTED_EDGE ( 'NONE', *, *, #40387, .T. ) ;
#19471 = CARTESIAN_POINT ( 'NONE',  ( 358.0000000000000000, 165.0000000000000000, -106.0000000000001990 ) ) ;
#19472 = FACE_OUTER_BOUND ( 'NONE', #6571, .T. ) ;
#19473 = CARTESIAN_POINT ( 'NONE',  ( 342.0000000000000568, 181.0000000000000284, 355.9999999999998863 ) ) ;
#19474 = CARTESIAN_POINT ( 'NONE',  ( -0.3862712429686809279, -1.188820645368943163, 10.00000000000000000 ) ) ;
#19475 = ORIENTED_EDGE ( 'NONE', *, *, #23641, .F. ) ;
#19476 = DIRECTION ( 'NONE',  ( 0.000000000000000000, 0.000000000000000000, -1.000000000000000000 ) ) ;
#19477 = ORIENTED_EDGE ( 'NONE', *, *, #5606, .T. ) ;
#19478 = CARTESIAN_POINT ( 'NONE',  ( 195.0540265531851105, 2.143131898507880377E-16, 39.06828755692798438 ) ) ;
#19479 = VERTEX_POINT ( 'NONE', #6861 ) ;
#19480 = DIRECTION ( 'NONE',  ( 0.000000000000000000, 0.000000000000000000, 1.000000000000000000 ) ) ;
#19481 = LINE ( 'NONE', #27953, #31516 ) ;
#19482 = VERTEX_POINT ( 'NONE', #25858 ) ;
#19483 = CARTESIAN_POINT ( 'NONE',  ( -15.00000000000001421, 16.00000000000000000, -90.00000000000000000 ) ) ;
#19484 = VERTEX_POINT ( 'NONE', #22257 ) ;
#19485 = EDGE_CURVE ( 'NONE', #3719, #37447, #49155, .T. ) ;
#19486 = VECTOR ( 'NONE', #2853, 1000.000000000000000 ) ;
#19487 = ORIENTED_EDGE ( 'NONE', *, *, #29564, .F. ) ;
#19488 = DIRECTION ( 'NONE',  ( -0.000000000000000000, -1.000000000000000000, 2.537652627714643577E-15 ) ) ;
#19489 = CARTESIAN_POINT ( 'NONE',  ( -4.999999999999997335, 204.9999999999999716, -234.7500000000000000 ) ) ;
#19490 = ORIENTED_EDGE ( 'NONE', *, *, #44739, .F. ) ;
#19491 = CARTESIAN_POINT ( 'NONE',  ( -30.25247992116029394, 39.82368563463828792, -3.760136334089591248 ) ) ;
#19492 = DIRECTION ( 'NONE',  ( 1.000000000000000000, -4.996003610813203446E-16, -1.586032878436834529E-16 ) ) ;
#19493 = LINE ( 'NONE', #35181, #9341 ) ;
#19494 = EDGE_LOOP ( 'NONE', ( #12019, #47500, #7905, #11897, #12626, #33085, #33772, #29099, #3654, #34225, #28119, #44884, #26920, #33231 ) ) ;
#19495 = CARTESIAN_POINT ( 'NONE',  ( 339.9999999999999432, -180.9999999999999716, -360.0000000000002274 ) ) ;
#19496 = DIRECTION ( 'NONE',  ( 0.000000000000000000, 0.000000000000000000, -1.000000000000000000 ) ) ;
#19497 = ORIENTED_EDGE ( 'NONE', *, *, #20192, .F. ) ;
#19498 = CARTESIAN_POINT ( 'NONE',  ( -1.035950918207909632, -50.00000000000000711, -2.408242355805840784 ) ) ;
#19499 = CARTESIAN_POINT ( 'NONE',  ( -126.6959734468149321, -1.749999999999997335, -79.18171244307201562 ) ) ;
#19500 =( BOUNDED_CURVE ( )  B_SPLINE_CURVE ( 3, ( #46652, #27200, #15644, #757 ),
 .UNSPECIFIED., .F., .F. ) 
 B_SPLINE_CURVE_WITH_KNOTS ( ( 4, 4 ),
 ( 1.570796326794896558, 3.141592653589793116 ),
 .UNSPECIFIED. ) 
 CURVE ( )  GEOMETRIC_REPRESENTATION_ITEM ( )  RATIONAL_B_SPLINE_CURVE ( ( 1.000000000000000000, 0.8047378541243649375, 0.8047378541243649375, 1.000000000000000000 ) ) 
 REPRESENTATION_ITEM ( '' )  );
#19501 = EDGE_LOOP ( 'NONE', ( #27417, #43401, #31658, #5536, #37153, #49265 ) ) ;
#19502 = DIRECTION ( 'NONE',  ( -1.586032892321652236E-16, -1.000000000000000000, -6.853681917100419162E-49 ) ) ;
#19503 = CARTESIAN_POINT ( 'NONE',  ( 32.57170742938662755, 18.58316106410423174, 7.697694107796188234 ) ) ;
#19504 = B_SPLINE_SURFACE_WITH_KNOTS ( 'NONE', 3, 3, ( 
 ( #3055, #42058, #33374, #5901 ),
 ( #30024, #21550, #37238, #6916 ),
 ( #22559, #17705, #10505, #41559 ),
 ( #38240, #18194, #10005, #25667 ) ),
 .UNSPECIFIED., .F., .F., .F.,
 ( 4, 4 ),
 ( 4, 4 ),
 ( 0.000000000000000000, 1.000000000000000000 ),
 ( 0.000000000000000000, 1.000000000000000000 ),
 .UNSPECIFIED. ) ;
#19505 = VERTEX_POINT ( 'NONE', #37930 ) ;
#19506 = CYLINDRICAL_SURFACE ( 'NONE', #3792, 4.000000000000003553 ) ;
#19507 = CARTESIAN_POINT ( 'NONE',  ( -48.33712804702535948, -13.03701565032741883, -9.367992836599951190 ) ) ;
#19508 = CARTESIAN_POINT ( 'NONE',  ( 153.3040265531850537, -1.750000000000010658, -119.1817124430720440 ) ) ;
#19509 = DIRECTION ( 'NONE',  ( 1.000000000000000000, 0.000000000000000000, 0.000000000000000000 ) ) ;
#19510 = ORIENTED_EDGE ( 'NONE', *, *, #6672, .T. ) ;
#19511 = CARTESIAN_POINT ( 'NONE',  ( -84.94597344681493212, 1.025126265847089213, -160.9317124430720014 ) ) ;
#19513 = EDGE_CURVE ( 'NONE', #50669, #24507, #38171, .T. ) ;
#19512 = CARTESIAN_POINT ( 'NONE',  ( 168.9999999999999716, -254.4999999999999432, -349.9999999999999432 ) ) ;
#19514 = CARTESIAN_POINT ( 'NONE',  ( 13.59579750444771307, -10.60877755095900632, 8.727788335465566760 ) ) ;
#19515 = ORIENTED_EDGE ( 'NONE', *, *, #3691, .T. ) ;
#19516 = EDGE_CURVE ( 'NONE', #42490, #13632, #45070, .T. ) ;
#19517 = ORIENTED_EDGE ( 'NONE', *, *, #30408, .F. ) ;
#19518 = DIRECTION ( 'NONE',  ( 1.000000000000000000, 0.000000000000000000, 0.000000000000000000 ) ) ;
#19519 = CARTESIAN_POINT ( 'NONE',  ( -208.4459734468149463, 0.000000000000000000, -80.93171244307201562 ) ) ;
#19520 = LINE ( 'NONE', #51, #38975 ) ;
#19521 = AXIS2_PLACEMENT_3D ( 'NONE', #40937, #44763, #9636 ) ;
#19522 = DIRECTION ( 'NONE',  ( 1.000000000000000000, 0.000000000000000000, 0.000000000000000000 ) ) ;
#19523 = CARTESIAN_POINT ( 'NONE',  ( 181.0000000000000284, -174.9999999999999716, -111.0000000000001563 ) ) ;
#19524 = CARTESIAN_POINT ( 'NONE',  ( 10.30302290646030627, 13.08520913973580058, -9.683996418299976483 ) ) ;
#19525 = ORIENTED_EDGE ( 'NONE', *, *, #7368, .T. ) ;
#19526 = CARTESIAN_POINT ( 'NONE',  ( 33.43156050989131955, -4.370686678976570150, 8.807470649214879543 ) ) ;
#19527 = EDGE_CURVE ( 'NONE', #16028, #44556, #18396, .T. ) ;
#19528 = EDGE_CURVE ( 'NONE', #32184, #41885, #42008, .T. ) ;
#19529 = CARTESIAN_POINT ( 'NONE',  ( 360.0000000000000568, -3.000000000000196732, -178.0000000000003695 ) ) ;
#19530 = CARTESIAN_POINT ( 'NONE',  ( -124.9459734468149463, 2.143131898507847836E-16, 165.0000000000000000 ) ) ;
#19531 = CARTESIAN_POINT ( 'NONE',  ( 193.3040265531851105, 0.000000000000000000, 165.0000000000000000 ) ) ;
#19532 = EDGE_CURVE ( 'NONE', #1115, #2541, #22503, .T. ) ;
#19533 = ORIENTED_EDGE ( 'NONE', *, *, #48630, .T. ) ;
#19534 = ORIENTED_EDGE ( 'NONE', *, *, #2640, .T. ) ;
#19535 = CARTESIAN_POINT ( 'NONE',  ( 135.0000000000021600, 17.00000000000000000, 115.0000000000000142 ) ) ;
#19536 = DIRECTION ( 'NONE',  ( 0.000000000000000000, 0.000000000000000000, 1.000000000000000000 ) ) ;
#19537 = ORIENTED_EDGE ( 'NONE', *, *, #41293, .F. ) ;
#19538 = CARTESIAN_POINT ( 'NONE',  ( -6.695973446814940111, 1.750000000000023759, 40.81828755692798438 ) ) ;
#19539 = DIRECTION ( 'NONE',  ( -1.000000000000000000, 0.000000000000000000, 0.000000000000000000 ) ) ;
#19540 = EDGE_CURVE ( 'NONE', #39358, #9482, #21749, .T. ) ;
#19541 = CARTESIAN_POINT ( 'NONE',  ( 32.00969891772083287, 38.54699130261819562, -8.917361510505369182 ) ) ;
#19542 = DIRECTION ( 'NONE',  ( 0.000000000000000000, -0.000000000000000000, 1.000000000000000000 ) ) ;
#19543 = EDGE_CURVE ( 'NONE', #31501, #2900, #37672, .T. ) ;
#19544 = ORIENTED_EDGE ( 'NONE', *, *, #40912, .F. ) ;
#19545 = ADVANCED_FACE ( 'NONE', ( #42502 ), #23535, .T. ) ;
#19546 = ADVANCED_FACE ( 'NONE', ( #23003 ), #22773, .T. ) ;
#19547 = DIRECTION ( 'NONE',  ( -1.000000000000000000, -0.000000000000000000, -0.000000000000000000 ) ) ;
#19548 = VERTEX_POINT ( 'NONE', #8140 ) ;
#19549 = DIRECTION ( 'NONE',  ( 1.000000000000000000, 0.000000000000000000, 0.000000000000000000 ) ) ;
#19550 = CARTESIAN_POINT ( 'NONE',  ( -0.1475726264153620626, -1.496347932843211215, 9.927319414211227766 ) ) ;
#19551 = DIRECTION ( 'NONE',  ( -1.000000000000000000, 0.000000000000000000, 0.000000000000000000 ) ) ;
#19552 = LINE ( 'NONE', #8536, #46314 ) ;
#19553 = EDGE_CURVE ( 'NONE', #27291, #29017, #34062, .T. ) ;
#19554 = EDGE_LOOP ( 'NONE', ( #46167, #29308, #6269, #16020, #4679, #27110, #13302, #42985 ) ) ;
#19555 = EDGE_LOOP ( 'NONE', ( #44805, #10520, #38653, #34956 ) ) ;
#19556 = AXIS2_PLACEMENT_3D ( 'NONE', #7290, #10126, #41432 ) ;
#19557 =( BOUNDED_CURVE ( )  B_SPLINE_CURVE ( 3, ( #28084, #48037, #20374, #24243 ),
 .UNSPECIFIED., .F., .F. ) 
 B_SPLINE_CURVE_WITH_KNOTS ( ( 4, 4 ),
 ( 4.712388980384689674, 6.283185307179586232 ),
 .UNSPECIFIED. ) 
 CURVE ( )  GEOMETRIC_REPRESENTATION_ITEM ( )  RATIONAL_B_SPLINE_CURVE ( ( 1.000000000000000000, 0.8047378541243649375, 0.8047378541243649375, 1.000000000000000000 ) ) 
 REPRESENTATION_ITEM ( '' )  );
#19558 = CIRCLE ( 'NONE', #2388, 2.000000000000001776 ) ;
#19559 = ORIENTED_EDGE ( 'NONE', *, *, #20191, .T. ) ;
#19560 = CARTESIAN_POINT ( 'NONE',  ( 210.0000000000000568, 0.000000000000000000, -37.43171244307202272 ) ) ;
#19561 = DIRECTION ( 'NONE',  ( -1.000000000000000000, 0.000000000000000000, -0.000000000000000000 ) ) ;
#19562 = FACE_OUTER_BOUND ( 'NONE', #16577, .T. ) ;
#19563 = VERTEX_POINT ( 'NONE', #46830 ) ;
#19565 = AXIS2_PLACEMENT_3D ( 'NONE', #21357, #39880, #43948 ) ;
#19564 = DIRECTION ( 'NONE',  ( 1.000000000000000000, 0.000000000000000000, -4.758098676964956461E-16 ) ) ;
#19566 = VECTOR ( 'NONE', #21031, 1000.000000000000000 ) ;
#19567 = EDGE_LOOP ( 'NONE', ( #19822, #29399, #12002, #6187 ) ) ;
#19568 =( BOUNDED_CURVE ( )  B_SPLINE_CURVE ( 3, ( #2007, #37185, #17653, #33320 ),
 .UNSPECIFIED., .F., .F. ) 
 B_SPLINE_CURVE_WITH_KNOTS ( ( 4, 4 ),
 ( 4.712388980384689674, 6.283185307179586232 ),
 .UNSPECIFIED. ) 
 CURVE ( )  GEOMETRIC_REPRESENTATION_ITEM ( )  RATIONAL_B_SPLINE_CURVE ( ( 1.000000000000000000, 0.8047378541243649375, 0.8047378541243649375, 1.000000000000000000 ) ) 
 REPRESENTATION_ITEM ( '' )  );
#19569 = CARTESIAN_POINT ( 'NONE',  ( -15.44803555374685189, -6.237487519713257100, -3.546734833711462365 ) ) ;
#19570 = AXIS2_PLACEMENT_3D ( 'NONE', #20538, #1046, #16192 ) ;
#19571 = ADVANCED_FACE ( 'NONE', ( #438 ), #46081, .T. ) ;
#19572 = DIRECTION ( 'NONE',  ( -0.000000000000000000, -0.000000000000000000, -1.000000000000000000 ) ) ;
#19573 = VECTOR ( 'NONE', #26381, 1000.000000000000000 ) ;
#19574 = CARTESIAN_POINT ( 'NONE',  ( 0.6440276692615888310, 16.64212148744554298, -9.683996418299976483 ) ) ;
#19575 = ADVANCED_FACE ( 'NONE', ( #34574 ), #7118, .T. ) ;
#19576 = EDGE_LOOP ( 'NONE', ( #30814, #29218, #21370, #42928 ) ) ;
#19577 = EDGE_CURVE ( 'NONE', #37650, #45334, #10143, .T. ) ;
#19578 = EDGE_LOOP ( 'NONE', ( #43998, #50420, #26854, #28007 ) ) ;
#19579 = ORIENTED_EDGE ( 'NONE', *, *, #29601, .F. ) ;
#19580 = DIRECTION ( 'NONE',  ( 0.000000000000000000, 0.000000000000000000, -1.000000000000000000 ) ) ;
#19581 = B_SPLINE_CURVE_WITH_KNOTS ( 'NONE', 3,
 ( #48705, #1813, #41059, #41561 ),
 .UNSPECIFIED., .F., .F.,
 ( 4, 4 ),
 ( 1.735570302229820823E-18, 8.326314924663078294E-06 ),
 .UNSPECIFIED. ) ;
#19583 = EDGE_CURVE ( 'NONE', #27396, #2997, #30727, .T. ) ;
#19582 = CARTESIAN_POINT ( 'NONE',  ( 191.5540265531851105, 0.000000000000000000, 162.5682875569279702 ) ) ;
#19584 = CARTESIAN_POINT ( 'NONE',  ( -22.51959565330812296, -30.03043964857251780, -6.568693074176339408 ) ) ;
#19585 = ORIENTED_EDGE ( 'NONE', *, *, #44379, .T. ) ;
#19586 = LINE ( 'NONE', #3683, #32985 ) ;
#19587 = ORIENTED_EDGE ( 'NONE', *, *, #19228, .T. ) ;
#19588 = EDGE_CURVE ( 'NONE', #28405, #20395, #15331, .T. ) ;
#19589 = DIRECTION ( 'NONE',  ( 0.000000000000000000, -1.000000000000000000, 0.000000000000000000 ) ) ;
#19590 = ORIENTED_EDGE ( 'NONE', *, *, #14240, .F. ) ;
#19591 =( LENGTH_UNIT ( ) NAMED_UNIT ( * ) SI_UNIT ( .MILLI., .METRE. ) );
#19592 = CARTESIAN_POINT ( 'NONE',  ( 0.000000000000000000, -166.9999999999999432, -356.0000000000002274 ) ) ;
#19593 = LINE ( 'NONE', #14991, #26027 ) ;
#19594 = DIRECTION ( 'NONE',  ( 0.000000000000000000, -1.000000000000000000, -1.544785076050074834E-48 ) ) ;
#19595 = DIRECTION ( 'NONE',  ( -1.000000000000000000, 0.000000000000000000, 0.000000000000000000 ) ) ;
#19596 = VERTEX_POINT ( 'NONE', #7626 ) ;
#19597 = ORIENTED_EDGE ( 'NONE', *, *, #30625, .T. ) ;
#19598 = CYLINDRICAL_SURFACE ( 'NONE', #43589, 40.00000000000000000 ) ;
#19599 = DIRECTION ( 'NONE',  ( -0.7233555441435721711, -0.6904757466825004464, 0.000000000000000000 ) ) ;
#19600 = FACE_OUTER_BOUND ( 'NONE', #18279, .T. ) ;
#19601 = B_SPLINE_CURVE_WITH_KNOTS ( 'NONE', 3,
 ( #40777, #32332, #44585, #9468 ),
 .UNSPECIFIED., .F., .F.,
 ( 4, 4 ),
 ( 0.01012863361515542113, 0.01015667504234211982 ),
 .UNSPECIFIED. ) ;
#19602 = CIRCLE ( 'NONE', #21248, 1.880036658038868991 ) ;
#19603 = AXIS2_PLACEMENT_3D ( 'NONE', #21371, #25228, #5723 ) ;
#19604 = LINE ( 'NONE', #11160, #3438 ) ;
#19605 = EDGE_CURVE ( 'NONE', #4495, #44090, #35098, .T. ) ;
#19606 = CARTESIAN_POINT ( 'NONE',  ( 33.57695195286775913, 16.69845195084893064, 8.914903342594561408 ) ) ;
#19607 = PRESENTATION_LAYER_ASSIGNMENT (  '', '', ( #14697 ) ) ;
#19608 = ORIENTED_EDGE ( 'NONE', *, *, #5796, .T. ) ;
#19609 = AXIS2_PLACEMENT_3D ( 'NONE', #13606, #6166, #22312 ) ;
#19610 = PLANE ( 'NONE',  #24595 ) ;
#19611 = CARTESIAN_POINT ( 'NONE',  ( -6.880036658038818587, -197.4999999999999432, -228.6347188485896140 ) ) ;
#19612 = ORIENTED_EDGE ( 'NONE', *, *, #21872, .T. ) ;
#19613 = VECTOR ( 'NONE', #5733, 1000.000000000000000 ) ;
#19614 = EDGE_CURVE ( 'NONE', #19783, #22379, #17338, .T. ) ;
#19615 = EDGE_CURVE ( 'NONE', #33842, #14142, #947, .T. ) ;
#19616 = CARTESIAN_POINT ( 'NONE',  ( 35.00000000000028422, 17.00000000000000000, -84.99999999999998579 ) ) ;
#19617 = CARTESIAN_POINT ( 'NONE',  ( -127.7210997126620242, 1.749999999999996669, 41.84341382277508359 ) ) ;
#19618 = EDGE_CURVE ( 'NONE', #12550, #7144, #50471, .T. ) ;
#19619 = DIRECTION ( 'NONE',  ( -1.000000000000000000, 0.000000000000000000, 0.000000000000000000 ) ) ;
#19620 = EDGE_CURVE ( 'NONE', #12768, #18535, #10167, .T. ) ;
#19621 = ORIENTED_EDGE ( 'NONE', *, *, #46014, .F. ) ;
#19622 = PRODUCT_DEFINITION_SHAPE ( 'NONE', 'NONE',  #50729 ) ;
#19623 = ORIENTED_EDGE ( 'NONE', *, *, #19343, .T. ) ;
#19624 = DIRECTION ( 'NONE',  ( -0.000000000000000000, -1.000000000000000000, -0.000000000000000000 ) ) ;
#19625 = EDGE_CURVE ( 'NONE', #27056, #41220, #44263, .T. ) ;
#19626 = CARTESIAN_POINT ( 'NONE',  ( -6.196515397221703303, -4.974751005920792224, 9.432811472610147518 ) ) ;
#19627 = ORIENTED_EDGE ( 'NONE', *, *, #17143, .F. ) ;
#19628 = ORIENTED_EDGE ( 'NONE', *, *, #15825, .T. ) ;
#19629 = CARTESIAN_POINT ( 'NONE',  ( 193.3040265531851105, -1.750000000000009992, -159.1817124430720298 ) ) ;
#19630 = CARTESIAN_POINT ( 'NONE',  ( -8.277096487746778308, 50.00000000000000711, 7.455576670931136185 ) ) ;
#19631 = LINE ( 'NONE', #34804, #24282 ) ;
#19632 = DIRECTION ( 'NONE',  ( 1.000000000000000000, 0.000000000000000000, 0.000000000000000000 ) ) ;
#19633 = VERTEX_POINT ( 'NONE', #48339 ) ;
#19634 = ORIENTED_EDGE ( 'NONE', *, *, #13464, .T. ) ;
#19635 = ORIENTED_EDGE ( 'NONE', *, *, #7340, .T. ) ;
#19636 = VECTOR ( 'NONE', #42078, 999.9999999999998863 ) ;
#19637 = DIRECTION ( 'NONE',  ( -1.000000000000000000, -0.000000000000000000, -0.000000000000000000 ) ) ;
#19638 = VECTOR ( 'NONE', #3319, 1000.000000000000000 ) ;
#19639 = DIRECTION ( 'NONE',  ( -0.000000000000000000, -0.000000000000000000, 1.000000000000000000 ) ) ;
#19640 = EDGE_LOOP ( 'NONE', ( #19840, #4267, #44167, #34189, #26204, #27762 ) ) ;
#19641 = VECTOR ( 'NONE', #28328, 1000.000000000000000 ) ;
#19642 = CARTESIAN_POINT ( 'NONE',  ( 1.066995270233474624, -33.23888904628638841, -3.760136334089591248 ) ) ;
#19643 = EDGE_CURVE ( 'NONE', #43762, #7812, #18976, .T. ) ;
#19644 = CARTESIAN_POINT ( 'NONE',  ( 357.1715728752542418, 167.0000000000003695, 342.0000000000001137 ) ) ;
#19645 = CARTESIAN_POINT ( 'NONE',  ( -1.448406091252275818, 0.9360325558308429938, 9.928159647716187308 ) ) ;
#19646 = EDGE_LOOP ( 'NONE', ( #32659, #41642, #47548, #33546, #10772 ) ) ;
#19647 = ORIENTED_EDGE ( 'NONE', *, *, #50041, .F. ) ;
#19648 = DIRECTION ( 'NONE',  ( -1.000000000000000000, 1.586032892321652236E-16, 9.711650524620651178E-33 ) ) ;
#19649 = AXIS2_PLACEMENT_3D ( 'NONE', #1035, #28487, #44599 ) ;
#19650 = FACE_OUTER_BOUND ( 'NONE', #15364, .T. ) ;
#19651 = CARTESIAN_POINT ( 'NONE',  ( 113.3040265531850537, -1.749999999999996891, 0.8182875569279768335 ) ) ;
#19652 = ORIENTED_EDGE ( 'NONE', *, *, #2894, .T. ) ;
#19653 = VERTEX_POINT ( 'NONE', #36623 ) ;
#19654 = CARTESIAN_POINT ( 'NONE',  ( -0.3862712429686977478, 1.188820645368937390, 10.00000000000000000 ) ) ;
#19655 = CARTESIAN_POINT ( 'NONE',  ( -225.0000000000000568, 164.9999999999999716, 231.9999999999999716 ) ) ;
#19656 = VERTEX_POINT ( 'NONE', #36358 ) ;
#19657 = AXIS2_PLACEMENT_3D ( 'NONE', #50240, #27464, #35179 ) ;
#19658 = FACE_OUTER_BOUND ( 'NONE', #18748, .T. ) ;
#19659 = CARTESIAN_POINT ( 'NONE',  ( 71.55402655318505367, -1.025126265847089435, -157.4317124430720582 ) ) ;
#19660 = LINE ( 'NONE', #11973, #5643 ) ;
#19661 = DIRECTION ( 'NONE',  ( -0.000000000000000000, -0.000000000000000000, -1.000000000000000000 ) ) ;
#19662 = ORIENTED_EDGE ( 'NONE', *, *, #48614, .T. ) ;
#19663 = EDGE_CURVE ( 'NONE', #38030, #24255, #24042, .T. ) ;
#19664 = DIRECTION ( 'NONE',  ( -0.000000000000000000, -1.000000000000000000, -0.000000000000000000 ) ) ;
#19665 = CARTESIAN_POINT ( 'NONE',  ( 6.000000000000000888, 7.347880794884120722E-16, 15.00000000000000000 ) ) ;
#19666 = CYLINDRICAL_SURFACE ( 'NONE', #3933, 1.750000000000008438 ) ;
#19667 = CARTESIAN_POINT ( 'NONE',  ( 16.50002041759926286, 3.070736177214647977, -9.233365092205394475 ) ) ;
#19668 = EDGE_LOOP ( 'NONE', ( #27279, #2500, #35006, #19674 ) ) ;
#19669 = CARTESIAN_POINT ( 'NONE',  ( 1.011271242968677653, 0.7347315653656002477, 10.00000000000000000 ) ) ;
#19670 = CARTESIAN_POINT ( 'NONE',  ( -17.23491422248386584, 0.5912720620001978844, 8.727788335465566760 ) ) ;
#19671 = VECTOR ( 'NONE', #964, 1000.000000000000000 ) ;
#19672 = CARTESIAN_POINT ( 'NONE',  ( 194.3291528190321742, 1.750000000000009548, -160.2068387089191219 ) ) ;
#19673 = AXIS2_PLACEMENT_3D ( 'NONE', #30672, #46268, #45769 ) ;
#19674 = ORIENTED_EDGE ( 'NONE', *, *, #1503, .F. ) ;
#19675 = CARTESIAN_POINT ( 'NONE',  ( 168.9999999999999716, -164.9999999999999432, -350.0000000000001705 ) ) ;
#19676 = EDGE_CURVE ( 'NONE', #11666, #30190, #43854, .T. ) ;
#19677 = ADVANCED_FACE ( 'NONE', ( #9136 ), #39695, .T. ) ;
#19678 = VECTOR ( 'NONE', #30187, 1000.000000000000000 ) ;
#19679 = CARTESIAN_POINT ( 'NONE',  ( -114.9999999999984652, 17.00000000000000000, 35.00000000000000000 ) ) ;
#19680 = AXIS2_PLACEMENT_3D ( 'NONE', #40926, #4763, #17321 ) ;
#19681 = ORIENTED_EDGE ( 'NONE', *, *, #19625, .T. ) ;
#19682 = CARTESIAN_POINT ( 'NONE',  ( -69.99999999999847944, 16.00000000000000000, 60.00000000000000000 ) ) ;
#19683 = CYLINDRICAL_SURFACE ( 'NONE', #50185, 6.000000000000000888 ) ;
#19684 = CARTESIAN_POINT ( 'NONE',  ( -45.67084718096785423, 1.750000000000010214, 121.8434138227750623 ) ) ;
#19685 = VECTOR ( 'NONE', #32091, 1000.000000000000000 ) ;
#19686 = ADVANCED_FACE ( 'NONE', ( #27889 ), #44017, .T. ) ;
#19687 = ORIENTED_EDGE ( 'NONE', *, *, #37885, .F. ) ;
#19688 = CARTESIAN_POINT ( 'NONE',  ( 115.0540265531850395, 1.025126265847081886, -80.93171244307201562 ) ) ;
#19689 = ORIENTED_EDGE ( 'NONE', *, *, #9385, .T. ) ;
#19690 = ORIENTED_EDGE ( 'NONE', *, *, #20507, .F. ) ;
#19691 = CARTESIAN_POINT ( 'NONE',  ( 29.61572577327002520, 16.11461842845735859, 8.807470649214879543 ) ) ;
#19692 = EDGE_CURVE ( 'NONE', #7457, #30535, #43774, .T. ) ;
#19693 = LINE ( 'NONE', #23801, #36963 ) ;
#19694 = EDGE_CURVE ( 'NONE', #44652, #48624, #4773, .T. ) ;
#19695 = AXIS2_PLACEMENT_3D ( 'NONE', #39778, #23866, #1529 ) ;
#19696 = ORIENTED_EDGE ( 'NONE', *, *, #18623, .F. ) ;
#19697 = DIRECTION ( 'NONE',  ( -0.000000000000000000, 1.544785076050074834E-48, 1.000000000000000000 ) ) ;
#19698 = CARTESIAN_POINT ( 'NONE',  ( -8.445973446814962315, -1.025126265847096985, 162.5682875569279986 ) ) ;
#19699 = EDGE_CURVE ( 'NONE', #25517, #43044, #17535, .T. ) ;
#19700 = DIRECTION ( 'NONE',  ( 0.000000000000000000, 0.000000000000000000, -1.000000000000000000 ) ) ;
#19701 = EDGE_LOOP ( 'NONE', ( #22416, #32916, #17857, #14158 ) ) ;
#19702 = DIRECTION ( 'NONE',  ( 0.000000000000000000, 0.000000000000000000, -1.000000000000000000 ) ) ;
#19703 = LINE ( 'NONE', #18924, #39018 ) ;
#19704 = CARTESIAN_POINT ( 'NONE',  ( 181.0000000000000000, -9.999999999999953815, -350.0000000000001705 ) ) ;
#19705 = VERTEX_POINT ( 'NONE', #28392 ) ;
#19706 = LINE ( 'NONE', #12504, #47229 ) ;
#19707 = CARTESIAN_POINT ( 'NONE',  ( 167.5000000000000000, -102.5000000000000142, -8.575805527524005711 ) ) ;
#19708 = ORIENTED_EDGE ( 'NONE', *, *, #4484, .F. ) ;
#19709 = ORIENTED_EDGE ( 'NONE', *, *, #6753, .F. ) ;
#19710 = VERTEX_POINT ( 'NONE', #44288 ) ;
#19711 = CARTESIAN_POINT ( 'NONE',  ( 23.31729631074197329, 24.19776167542427814, -8.016098858316199838 ) ) ;
#19712 = CARTESIAN_POINT ( 'NONE',  ( 34.32915281903212446, -1.750000000000010436, 119.7931612910808781 ) ) ;
#19713 = EDGE_LOOP ( 'NONE', ( #47794, #9448, #39168, #33139, #21977, #8847, #19824, #41835 ) ) ;
#19714 = AXIS2_PLACEMENT_3D ( 'NONE', #31256, #11743, #38448 ) ;
#19715 = CARTESIAN_POINT ( 'NONE',  ( -23.29043492822808759, 24.10797434788186067, 1.847720168420772691 ) ) ;
#19716 = CARTESIAN_POINT ( 'NONE',  ( 9.999999999999994671, -1.084202172485504187E-16, 9.303249460322209785 ) ) ;
#19717 = CARTESIAN_POINT ( 'NONE',  ( -208.4459734468149463, 0.000000000000000000, 165.0000000000000000 ) ) ;
#19718 = AXIS2_PLACEMENT_3D ( 'NONE', #47401, #11800, #42329 ) ;
#19719 = DIRECTION ( 'NONE',  ( 1.000000000000000000, 0.000000000000000000, 0.000000000000000000 ) ) ;
#19720 = DIRECTION ( 'NONE',  ( -1.000000000000000000, -0.000000000000000000, -0.000000000000000000 ) ) ;
#19721 = CARTESIAN_POINT ( 'NONE',  ( -167.7210997126620384, -1.750000000000010214, 79.79316129108087807 ) ) ;
#19722 = CARTESIAN_POINT ( 'NONE',  ( -84.94597344681494633, 2.143131898507880377E-16, 39.06828755692798438 ) ) ;
#19723 =( LENGTH_UNIT ( ) NAMED_UNIT ( * ) SI_UNIT ( .MILLI., .METRE. ) );
#19724 = DIRECTION ( 'NONE',  ( 0.000000000000000000, 0.000000000000000000, 1.000000000000000000 ) ) ;
#19725 = VECTOR ( 'NONE', #7733, 1000.000000000000000 ) ;
#19726 = FACE_OUTER_BOUND ( 'NONE', #3876, .T. ) ;
#19727 = VECTOR ( 'NONE', #12288, 1000.000000000000000 ) ;
#19728 = EDGE_CURVE ( 'NONE', #13070, #44903, #4794, .T. ) ;
#19729 = CYLINDRICAL_SURFACE ( 'NONE', #18333, 2.000000000000001776 ) ;
#19730 = CARTESIAN_POINT ( 'NONE',  ( 214.9999999999999432, 164.9999999999999716, 352.0000000000000000 ) ) ;
#19731 = CARTESIAN_POINT ( 'NONE',  ( 14.49999999999999822, 12.98684210526315930, 19.37312575500900280 ) ) ;
#19732 = DIRECTION ( 'NONE',  ( 0.000000000000000000, 0.000000000000000000, -1.000000000000000000 ) ) ;
#19733 = ORIENTED_EDGE ( 'NONE', *, *, #22712, .F. ) ;
#19734 = CARTESIAN_POINT ( 'NONE',  ( -23.79193388295331602, -28.98609808354994044, -9.422646554964178023 ) ) ;
#19735 =( BOUNDED_CURVE ( )  B_SPLINE_CURVE ( 3, ( #1210, #5293, #16595, #20950 ),
 .UNSPECIFIED., .F., .F. ) 
 B_SPLINE_CURVE_WITH_KNOTS ( ( 4, 4 ),
 ( 3.141592653589793116, 4.712388980384710990 ),
 .UNSPECIFIED. ) 
 CURVE ( )  GEOMETRIC_REPRESENTATION_ITEM ( )  RATIONAL_B_SPLINE_CURVE ( ( 1.000000000000000000, 0.8047378541243599415, 0.8047378541243599415, 1.000000000000000000 ) ) 
 REPRESENTATION_ITEM ( '' )  );
#19736 = DIRECTION ( 'NONE',  ( 0.000000000000000000, 1.000000000000000000, 0.000000000000000000 ) ) ;
#19737 = FACE_OUTER_BOUND ( 'NONE', #16252, .T. ) ;
#19738 = CARTESIAN_POINT ( 'NONE',  ( -16.99749102614300966, 1.320765928724422222, 8.953103998512858652 ) ) ;
#19739 = EDGE_LOOP ( 'NONE', ( #27029, #34649 ) ) ;
#19740 = LINE ( 'NONE', #35419, #17441 ) ;
#19741 = ORIENTED_EDGE ( 'NONE', *, *, #20236, .F. ) ;
#19742 = EDGE_CURVE ( 'NONE', #27161, #2812, #33094, .T. ) ;
#19743 = DIRECTION ( 'NONE',  ( -6.938893903907222461E-16, -0.000000000000000000, -1.000000000000000000 ) ) ;
#19744 = ORIENTED_EDGE ( 'NONE', *, *, #13283, .T. ) ;
#19745 = CARTESIAN_POINT ( 'NONE',  ( 153.3040265531850537, -1.750000000000009992, -159.1817124430720298 ) ) ;
#19746 = CARTESIAN_POINT ( 'NONE',  ( 195.0540265531851105, 2.143131898507880377E-16, 122.5682875569279702 ) ) ;
#19747 = EDGE_LOOP ( 'NONE', ( #9018, #5880, #40166, #38739, #7278 ) ) ;
#19748 = FACE_OUTER_BOUND ( 'NONE', #2889, .T. ) ;
#19749 = ORIENTED_EDGE ( 'NONE', *, *, #22527, .T. ) ;
#19750 = AXIS2_PLACEMENT_3D ( 'NONE', #7075, #43227, #27599 ) ;
#19751 = EDGE_CURVE ( 'NONE', #4003, #41575, #24566, .T. ) ;
#19752 = EDGE_CURVE ( 'NONE', #39413, #45145, #23620, .T. ) ;
#19753 = ORIENTED_EDGE ( 'NONE', *, *, #50522, .T. ) ;
#19754 = CARTESIAN_POINT ( 'NONE',  ( 191.5540265531851105, 0.000000000000000000, 165.0000000000000000 ) ) ;
#19755 =( REPRESENTATION_RELATIONSHIP ('NONE','NONE', #45699, #3157 ) REPRESENTATION_RELATIONSHIP_WITH_TRANSFORMATION ( #1051 )SHAPE_REPRESENTATION_RELATIONSHIP( ) );
#19756 = EDGE_LOOP ( 'NONE', ( #8896, #42749, #15368, #18594, #11904, #25352 ) ) ;
#19757 = DIRECTION ( 'NONE',  ( 0.000000000000000000, 0.000000000000000000, -1.000000000000000000 ) ) ;
#19758 = EDGE_CURVE ( 'NONE', #8521, #5706, #10446, .T. ) ;
#19759 = LINE ( 'NONE', #36710, #38029 ) ;
#19760 = VERTEX_POINT ( 'NONE', #43799 ) ;
#19761 = VECTOR ( 'NONE', #15763, 1000.000000000000000 ) ;
#19762 = LINE ( 'NONE', #50505, #27563 ) ;
#19763 = CARTESIAN_POINT ( 'NONE',  ( 164.9999999999999716, 175.0000000000000284, -344.0000000000001137 ) ) ;
#19764 = VERTEX_POINT ( 'NONE', #12997 ) ;
#19765 = DIRECTION ( 'NONE',  ( -1.586032892321652236E-16, -1.000000000000000000, -6.853681917100419162E-49 ) ) ;
#19766 = CARTESIAN_POINT ( 'NONE',  ( 224.9999999999999716, -164.9999999999999716, 32.29650858650035161 ) ) ;
#19767 = EDGE_LOOP ( 'NONE', ( #27554, #12607, #39772, #49675, #21968, #3035 ) ) ;
#19768 = CARTESIAN_POINT ( 'NONE',  ( -88.44597344681497475, 0.000000000000000000, -0.9317124430720524764 ) ) ;
#19769 = CARTESIAN_POINT ( 'NONE',  ( -86.69597344681494633, 1.750000000000010658, 120.8182875569279702 ) ) ;
#19770 = EDGE_LOOP ( 'NONE', ( #27310, #3667, #5318, #10826, #28101 ) ) ;
#19771 = CARTESIAN_POINT ( 'NONE',  ( -1.073226156958101862, -0.6788500330460245369, 9.975314328424618182 ) ) ;
#19772 = CARTESIAN_POINT ( 'NONE',  ( -0.3862712429686895876, 1.188820645368940720, -10.00000000000000000 ) ) ;
#19773 = LINE ( 'NONE', #4641, #32814 ) ;
#19774 = CARTESIAN_POINT ( 'NONE',  ( 72.27890028733797578, -1.750000000000010214, -120.2068387089191219 ) ) ;
#19775 = ORIENTED_EDGE ( 'NONE', *, *, #36185, .F. ) ;
#19776 = CARTESIAN_POINT ( 'NONE',  ( 0.3862712429686727678, 1.188820645368945605, 10.00000000000000000 ) ) ;
#19777 = CARTESIAN_POINT ( 'NONE',  ( 0.000000000000000000, 23.48684210526316107, 0.000000000000000000 ) ) ;
#19778 = AXIS2_PLACEMENT_3D ( 'NONE', #13840, #17943, #33628 ) ;
#19779 = CARTESIAN_POINT ( 'NONE',  ( 210.0000000000000568, 2.143131898507880377E-16, 159.0682875569279702 ) ) ;
#19780 = ORIENTED_EDGE ( 'NONE', *, *, #35600, .T. ) ;
#19781 = ADVANCED_FACE ( 'NONE', ( #17113 ), #16611, .T. ) ;
#19783 = VERTEX_POINT ( 'NONE', #28169 ) ;
#19782 = VECTOR ( 'NONE', #36147, 1000.000000000000000 ) ;
#19784 = DIRECTION ( 'NONE',  ( 0.06908597091091817077, 1.369134433078534943E-14, 0.9976107099581962290 ) ) ;
#19785 = CARTESIAN_POINT ( 'NONE',  ( 111.5540265531850537, -1.025126265847081886, -80.93171244307201562 ) ) ;
#19786 = CARTESIAN_POINT ( 'NONE',  ( -4.641001526964561030, -50.00000000000000000, -8.016098858316205167 ) ) ;
#19787 = CARTESIAN_POINT ( 'NONE',  ( -206.6959734468149463, 1.750000000000010214, -39.18171244307202983 ) ) ;
#19788 = CARTESIAN_POINT ( 'NONE',  ( 2.538055338523173443, 50.00000000000000000, -9.367992836599951190 ) ) ;
#19789 = VERTEX_POINT ( 'NONE', #16109 ) ;
#19790 = CARTESIAN_POINT ( 'NONE',  ( -20.00000000000003197, 17.00000000000000000, -114.9999999999999858 ) ) ;
#19792 = VECTOR ( 'NONE', #29091, 1000.000000000000000 ) ;
#19791 = DIRECTION ( 'NONE',  ( -1.000000000000000000, 0.000000000000000000, 0.000000000000000000 ) ) ;
#19793 = DIRECTION ( 'NONE',  ( -1.000000000000000000, -0.000000000000000000, -0.000000000000000000 ) ) ;
#19794 = CYLINDRICAL_SURFACE ( 'NONE', #41190, 1.750000000000001554 ) ;
#19795 = EDGE_LOOP ( 'NONE', ( #21878, #26011, #12447, #330 ) ) ;
#19796 = CARTESIAN_POINT ( 'NONE',  ( 10.50000000000000178, -46.01315789473684248, 5.916985404131813731 ) ) ;
#19797 = ORIENTED_EDGE ( 'NONE', *, *, #11131, .T. ) ;
#19798 = DIRECTION ( 'NONE',  ( 1.000000000000000000, 0.000000000000000000, -0.000000000000000000 ) ) ;
#19799 = ORIENTED_EDGE ( 'NONE', *, *, #7305, .F. ) ;
#19800 = DIRECTION ( 'NONE',  ( -0.000000000000000000, -0.000000000000000000, -1.000000000000000000 ) ) ;
#19801 = DIRECTION ( 'NONE',  ( 4.758098676964956461E-16, 1.000000000000000000, 0.000000000000000000 ) ) ;
#19802 = DIRECTION ( 'NONE',  ( -0.000000000000000000, -0.000000000000000000, -1.000000000000000000 ) ) ;
#19803 = CARTESIAN_POINT ( 'NONE',  ( -50.64730461691362962, 47.68801056904006685, 742.8425600500171413 ) ) ;
#19804 = ORIENTED_EDGE ( 'NONE', *, *, #534, .T. ) ;
#19805 = CARTESIAN_POINT ( 'NONE',  ( 181.0000000000000000, -79.49999999999997158, -350.0000000000001705 ) ) ;
#19806 = LINE ( 'NONE', #35751, #46701 ) ;
#19807 = ORIENTED_EDGE ( 'NONE', *, *, #15552, .T. ) ;
#19808 = DIRECTION ( 'NONE',  ( -0.000000000000000000, -1.000000000000000000, -0.000000000000000000 ) ) ;
#19809 = CARTESIAN_POINT ( 'NONE',  ( -126.6959734468149321, 1.749999999999996891, 160.8182875569279702 ) ) ;
#19810 =( BOUNDED_CURVE ( )  B_SPLINE_CURVE ( 3, ( #6123, #13306, #24624, #1279 ),
 .UNSPECIFIED., .F., .F. ) 
 B_SPLINE_CURVE_WITH_KNOTS ( ( 4, 4 ),
 ( 0.000000000000000000, 1.570796326794896558 ),
 .UNSPECIFIED. ) 
 CURVE ( )  GEOMETRIC_REPRESENTATION_ITEM ( )  RATIONAL_B_SPLINE_CURVE ( ( 1.000000000000000000, 0.8047378541243649375, 0.8047378541243649375, 1.000000000000000000 ) ) 
 REPRESENTATION_ITEM ( '' )  );
#19811 = PLANE ( 'NONE',  #40176 ) ;
#19812 = LINE ( 'NONE', #27274, #37372 ) ;
#19813 = EDGE_CURVE ( 'NONE', #357, #22708, #39474, .T. ) ;
#19814 = ORIENTED_EDGE ( 'NONE', *, *, #42831, .T. ) ;
#19815 = ORIENTED_EDGE ( 'NONE', *, *, #2920, .T. ) ;
#19816 = CARTESIAN_POINT ( 'NONE',  ( 155.0540265531850537, 2.143131898507880377E-16, -40.93171244307202983 ) ) ;
#19817 = ORIENTED_EDGE ( 'NONE', *, *, #30537, .T. ) ;
#19818 = VECTOR ( 'NONE', #13410, 1000.000000000000000 ) ;
#19819 = CARTESIAN_POINT ( 'NONE',  ( -54.99999999999997868, -52.50000000000000711, -5.000000000000000000 ) ) ;
#19820 = FACE_OUTER_BOUND ( 'NONE', #42707, .T. ) ;
#19821 = DIRECTION ( 'NONE',  ( -0.000000000000000000, -0.000000000000000000, -1.000000000000000000 ) ) ;
#19822 = ORIENTED_EDGE ( 'NONE', *, *, #9570, .T. ) ;
#19823 = CARTESIAN_POINT ( 'NONE',  ( 191.5540265531851105, 0.000000000000000000, 165.0000000000000000 ) ) ;
#19824 = ORIENTED_EDGE ( 'NONE', *, *, #47426, .F. ) ;
#19825 = DIRECTION ( 'NONE',  ( 6.203854594147707562E-25, -2.067951531382569187E-25, 1.000000000000000000 ) ) ;
#19826 = ADVANCED_FACE ( 'NONE', ( #8673 ), #47870, .F. ) ;
#19827 = B_SPLINE_CURVE_WITH_KNOTS ( 'NONE', 3,
 ( #50312, #38589, #30889, #31392, #27541, #344 ),
 .UNSPECIFIED., .F., .F.,
 ( 4, 2, 4 ),
 ( 4.906538933386797396E-18, 0.009877169331704833619, 0.01975433866340966030 ),
 .UNSPECIFIED. ) ;
#19828 = CARTESIAN_POINT ( 'NONE',  ( -1.011271242968688533, 0.7347315653655859258, 10.00000000000000000 ) ) ;
#19829 = CARTESIAN_POINT ( 'NONE',  ( -8.277096487746778308, 33.14818118907697198, 7.455576670931136185 ) ) ;
#19830 = ORIENTED_EDGE ( 'NONE', *, *, #32109, .T. ) ;
#19831 = VERTEX_POINT ( 'NONE', #20970 ) ;
#19832 = ORIENTED_EDGE ( 'NONE', *, *, #10325, .F. ) ;
#19833 = DIRECTION ( 'NONE',  ( 0.000000000000000000, 0.000000000000000000, -1.000000000000000000 ) ) ;
#19834 = CARTESIAN_POINT ( 'NONE',  ( -64.99999999999846523, 17.00000000000000000, 35.00000000000000000 ) ) ;
#19835 = VERTEX_POINT ( 'NONE', #36654 ) ;
#19836 = CARTESIAN_POINT ( 'NONE',  ( 183.0000000000000000, -184.9999999999999716, -356.0000000000014211 ) ) ;
#19837 = ADVANCED_FACE ( 'NONE', ( #20210 ), #24070, .T. ) ;
#19838 = VERTEX_POINT ( 'NONE', #4313 ) ;
#19839 = DIRECTION ( 'NONE',  ( -1.000000000000000000, -0.000000000000000000, -0.000000000000000000 ) ) ;
#19840 = ORIENTED_EDGE ( 'NONE', *, *, #46011, .T. ) ;
#19841 = LINE ( 'NONE', #3687, #50377 ) ;
#19842 = EDGE_CURVE ( 'NONE', #30983, #30113, #24329, .T. ) ;
#19843 = CARTESIAN_POINT ( 'NONE',  ( 168.9999999999999716, 6.000000000000060396, 339.9999999999998295 ) ) ;
#19844 = LINE ( 'NONE', #20607, #44849 ) ;
#19845 = CARTESIAN_POINT ( 'NONE',  ( -168.4459734468149747, 1.025126265847089435, -117.4317124430720156 ) ) ;
#19846 = PLANE ( 'NONE',  #20054 ) ;
#19847 = CARTESIAN_POINT ( 'NONE',  ( 0.000000000000000000, -175.0000000000000284, 353.7500000000001705 ) ) ;
#19848 = ORIENTED_EDGE ( 'NONE', *, *, #42550, .F. ) ;
#19849 = ORIENTED_EDGE ( 'NONE', *, *, #39357, .T. ) ;
#19850 = DIRECTION ( 'NONE',  ( 0.000000000000000000, -0.000000000000000000, 1.000000000000000000 ) ) ;
#19851 = AXIS2_PLACEMENT_3D ( 'NONE', #10619, #26033, #5326 ) ;
#19852 = CARTESIAN_POINT ( 'NONE',  ( 130.0000000000012221, 17.00000000000000000, 5.000000000000004441 ) ) ;
#19853 = CARTESIAN_POINT ( 'NONE',  ( -3.441214337941710610, 1.549069628443896285, 9.865049507598756762 ) ) ;
#19854 = AXIS2_PLACEMENT_3D ( 'NONE', #25539, #41179, #6029 ) ;
#19855 = SURFACE_SIDE_STYLE ('',( #47533 ) ) ;
#19856 = CIRCLE ( 'NONE', #48492, 2.000000000000001776 ) ;
#19857 = DIRECTION ( 'NONE',  ( -1.000000000000000000, 0.000000000000000000, -0.000000000000000000 ) ) ;
#19858 = ORIENTED_EDGE ( 'NONE', *, *, #10236, .F. ) ;
#19859 = CYLINDRICAL_SURFACE ( 'NONE', #49112, 0.4999999999999992228 ) ;
#19860 = DIRECTION ( 'NONE',  ( 0.000000000000000000, 0.000000000000000000, 1.000000000000000000 ) ) ;
#19861 = ORIENTED_EDGE ( 'NONE', *, *, #47108, .T. ) ;
#19862 =( BOUNDED_CURVE ( )  B_SPLINE_CURVE ( 3, ( #43504, #8375, #24021, #31979 ),
 .UNSPECIFIED., .F., .F. ) 
 B_SPLINE_CURVE_WITH_KNOTS ( ( 4, 4 ),
 ( 1.570796326794896558, 3.141592653589793116 ),
 .UNSPECIFIED. ) 
 CURVE ( )  GEOMETRIC_REPRESENTATION_ITEM ( )  RATIONAL_B_SPLINE_CURVE ( ( 1.000000000000000000, 0.8047378541243649375, 0.8047378541243649375, 1.000000000000000000 ) ) 
 REPRESENTATION_ITEM ( '' )  );
#19863 = EDGE_CURVE ( 'NONE', #45661, #7807, #24247, .T. ) ;
#19864 = EDGE_CURVE ( 'NONE', #38973, #26951, #28421, .T. ) ;
#19865 = FACE_OUTER_BOUND ( 'NONE', #26339, .T. ) ;
#19866 = CARTESIAN_POINT ( 'NONE',  ( 164.9999999999999716, -164.9999999999999432, -344.0000000000001137 ) ) ;
#19867 = LINE ( 'NONE', #28584, #9460 ) ;
#19868 = EDGE_CURVE ( 'NONE', #36027, #4421, #39725, .T. ) ;
#19869 =( BOUNDED_CURVE ( )  B_SPLINE_CURVE ( 3, ( #45130, #44879, #2559, #33882 ),
 .UNSPECIFIED., .F., .F. ) 
 B_SPLINE_CURVE_WITH_KNOTS ( ( 4, 4 ),
 ( 1.570796326794896558, 3.141592653589793116 ),
 .UNSPECIFIED. ) 
 CURVE ( )  GEOMETRIC_REPRESENTATION_ITEM ( )  RATIONAL_B_SPLINE_CURVE ( ( 1.000000000000000000, 0.8047378541243649375, 0.8047378541243649375, 1.000000000000000000 ) ) 
 REPRESENTATION_ITEM ( '' )  );
#19870 = AXIS2_PLACEMENT_3D ( 'NONE', #46475, #3148, #22915 ) ;
#19871 = VERTEX_POINT ( 'NONE', #16358 ) ;
#19872 = ORIENTED_EDGE ( 'NONE', *, *, #44457, .T. ) ;
#19873 = DIRECTION ( 'NONE',  ( -0.000000000000000000, -1.000000000000000000, -0.000000000000000000 ) ) ;
#19874 = EDGE_CURVE ( 'NONE', #43828, #25523, #1316, .T. ) ;
#19875 = CARTESIAN_POINT ( 'NONE',  ( 153.3040265531850537, -1.750000000000009992, 0.8182875569279768335 ) ) ;
#19876 = ADVANCED_FACE ( 'NONE', ( #41211 ), #36902, .T. ) ;
#19877 = ORIENTED_EDGE ( 'NONE', *, *, #31485, .T. ) ;
#19878 = ORIENTED_EDGE ( 'NONE', *, *, #47586, .F. ) ;
#19879 = LINE ( 'NONE', #8096, #48308 ) ;
#19880 = PLANE ( 'NONE',  #47826 ) ;
#19881 = CARTESIAN_POINT ( 'NONE',  ( 73.30402655318508209, 1.750000000000010658, 120.8182875569279702 ) ) ;
#19882 =( GEOMETRIC_REPRESENTATION_CONTEXT ( 3 ) GLOBAL_UNCERTAINTY_ASSIGNED_CONTEXT ( ( #20482 ) ) GLOBAL_UNIT_ASSIGNED_CONTEXT ( ( #6522, #18567, #45993 ) ) REPRESENTATION_CONTEXT ( 'NONE', 'WORKASPACE' ) );
#19883 = ORIENTED_EDGE ( 'NONE', *, *, #18868, .F. ) ;
#19884 = ORIENTED_EDGE ( 'NONE', *, *, #25759, .F. ) ;
#19885 = EDGE_LOOP ( 'NONE', ( #26726, #40920, #41818, #39206, #45979 ) ) ;
#19886 = MECHANICAL_DESIGN_GEOMETRIC_PRESENTATION_REPRESENTATION (  '', ( #14951 ), #35521 ) ;
#19887 = CARTESIAN_POINT ( 'NONE',  ( -4.945973446814917018, -1.025126265847096985, 42.56828755692800570 ) ) ;
#19888 = VERTEX_POINT ( 'NONE', #25572 ) ;
#19889 = CARTESIAN_POINT ( 'NONE',  ( 4.672045878990125800, -33.19353511768168374, 1.847720168420772691 ) ) ;
#19890 = VECTOR ( 'NONE', #27247, 1000.000000000000000 ) ;
#19891 = CARTESIAN_POINT ( 'NONE',  ( 16.91580242619102137, 33.50775492265647415, 4.835783797351798974 ) ) ;
#19892 = ORIENTED_EDGE ( 'NONE', *, *, #6719, .T. ) ;
#19893 = ORIENTED_EDGE ( 'NONE', *, *, #11144, .T. ) ;
#19894 = CARTESIAN_POINT ( 'NONE',  ( 80.00000000000092371, 17.00000000000000000, -24.99999999999999289 ) ) ;
#19895 = DIRECTION ( 'NONE',  ( -1.000000000000000000, -0.000000000000000000, -0.000000000000000000 ) ) ;
#19896 = VERTEX_POINT ( 'NONE', #48870 ) ;
#19897 = ADVANCED_FACE ( 'NONE', ( #1722 ), #2469, .F. ) ;
#19898 = EDGE_CURVE ( 'NONE', #37204, #42077, #36711, .T. ) ;
#19899 = ORIENTED_EDGE ( 'NONE', *, *, #7062, .T. ) ;
#19900 = CARTESIAN_POINT ( 'NONE',  ( 75.05402655318509630, 2.143131898507880377E-16, -160.9317124430720582 ) ) ;
#19901 = CARTESIAN_POINT ( 'NONE',  ( -4.945973446814903696, 2.143131898507912917E-16, -160.9317124430720582 ) ) ;
#19902 = EDGE_LOOP ( 'NONE', ( #22783, #8631, #34930 ) ) ;
#19903 = EDGE_CURVE ( 'NONE', #50334, #9206, #15398, .T. ) ;
#19904 = DIRECTION ( 'NONE',  ( -1.000000000000000000, 0.000000000000000000, 0.000000000000000000 ) ) ;
#19905 = LINE ( 'NONE', #16826, #40783 ) ;
#19906 = CARTESIAN_POINT ( 'NONE',  ( -215.0000000000000568, -173.0000000000000000, 132.0000000000001137 ) ) ;
#19907 = EDGE_CURVE ( 'NONE', #3402, #26155, #32815, .T. ) ;
#19908 = ORIENTED_EDGE ( 'NONE', *, *, #36838, .T. ) ;
#19909 = EDGE_CURVE ( 'NONE', #9194, #9127, #16004, .T. ) ;
#19910 = DIRECTION ( 'NONE',  ( 0.000000000000000000, -1.000000000000000000, -3.186989995019654210E-49 ) ) ;
#19911 = ADVANCED_FACE ( 'NONE', ( #49376 ), #43701, .T. ) ;
#19912 = CARTESIAN_POINT ( 'NONE',  ( 214.9999999999999432, 0.000000000000000000, 10.00000000000000000 ) ) ;
#19913 = CARTESIAN_POINT ( 'NONE',  ( -4.945973446814903696, 2.143131898507913410E-16, -165.0000000000000000 ) ) ;
#19914 = CARTESIAN_POINT ( 'NONE',  ( 135.0000000000003411, 17.00000000000000000, -84.99999999999998579 ) ) ;
#19915 = AXIS2_PLACEMENT_3D ( 'NONE', #16091, #11733, #27899 ) ;
#19916 = DIRECTION ( 'NONE',  ( 0.000000000000000000, 1.000000000000000000, 0.000000000000000000 ) ) ;
#19917 = AXIS2_PLACEMENT_3D ( 'NONE', #11399, #47957, #23197 ) ;
#19918 = CARTESIAN_POINT ( 'NONE',  ( 1.250000000000000222, 0.000000000000000000, -3.333333333333333481 ) ) ;
#19919 = EDGE_CURVE ( 'NONE', #3733, #1058, #13783, .T. ) ;
#19920 = DIRECTION ( 'NONE',  ( 0.000000000000000000, -0.2223603367690619725, 0.9749645535258958384 ) ) ;
#19921 = VECTOR ( 'NONE', #41010, 1000.000000000000000 ) ;
#19922 = VERTEX_POINT ( 'NONE', #9664 ) ;
#19923 = EDGE_CURVE ( 'NONE', #38528, #14628, #25828, .T. ) ;
#19924 = EDGE_CURVE ( 'NONE', #16572, #13422, #5816, .T. ) ;
#19925 = VECTOR ( 'NONE', #25670, 1000.000000000000000 ) ;
#19926 = CARTESIAN_POINT ( 'NONE',  ( 194.3291528190321742, -1.750000000000009548, 161.8434138227750907 ) ) ;
#19927 = ORIENTED_EDGE ( 'NONE', *, *, #12431, .F. ) ;
#19928 = CARTESIAN_POINT ( 'NONE',  ( 49.46074318306830975, -9.578883844006831794, 8.807470649214879543 ) ) ;
#19929 = DIRECTION ( 'NONE',  ( -1.000000000000000000, 0.000000000000000000, 0.000000000000000000 ) ) ;
#19930 = CARTESIAN_POINT ( 'NONE',  ( 32.27890028733795447, -1.750000000000009548, 1.843413822775065825 ) ) ;
#19931 = EDGE_LOOP ( 'NONE', ( #21666, #47687, #39202, #28408, #3785, #45626, #28744, #46957 ) ) ;
#19932 = CARTESIAN_POINT ( 'NONE',  ( 114.3291528190321173, 1.749999999999996891, -80.20683870891909351 ) ) ;
#19933 = B_SPLINE_SURFACE_WITH_KNOTS ( 'NONE', 3, 3, ( 
 ( #12804, #17407, #48654, #28709 ),
 ( #4609, #33075, #39767, #8720 ),
 ( #21256, #25116, #44084, #16918 ),
 ( #32825, #28210, #8956, #28465 ) ),
 .UNSPECIFIED., .F., .F., .F.,
 ( 4, 4 ),
 ( 4, 4 ),
 ( 0.000000000000000000, 1.000000000000000000 ),
 ( 0.000000000000000000, 1.000000000000000000 ),
 .UNSPECIFIED. ) ;
#19934 = VERTEX_POINT ( 'NONE', #1968 ) ;
#19935 = ORIENTED_EDGE ( 'NONE', *, *, #10247, .F. ) ;
#19936 = DIRECTION ( 'NONE',  ( 0.000000000000000000, 0.000000000000000000, -1.000000000000000000 ) ) ;
#19937 = DIRECTION ( 'NONE',  ( 0.000000000000000000, 0.000000000000000000, 1.000000000000000000 ) ) ;
#19938 = ORIENTED_EDGE ( 'NONE', *, *, #10513, .F. ) ;
#19939 = CARTESIAN_POINT ( 'NONE',  ( 193.3040265531851105, 0.000000000000000000, 165.0000000000000000 ) ) ;
#19940 = CARTESIAN_POINT ( 'NONE',  ( 130.0000000000008811, 17.00000000000000000, -24.99999999999999289 ) ) ;
#19941 = EDGE_CURVE ( 'NONE', #24424, #21250, #20637, .T. ) ;
#19942 = LINE ( 'NONE', #45221, #29233 ) ;
#19943 = VERTEX_POINT ( 'NONE', #9914 ) ;
#19944 = FACE_OUTER_BOUND ( 'NONE', #33979, .T. ) ;
#19945 = DIRECTION ( 'NONE',  ( 0.000000000000000000, 1.000000000000000000, 0.000000000000000000 ) ) ;
#19946 = DIRECTION ( 'NONE',  ( 1.000000000000000000, 0.000000000000000000, -2.312964634635864737E-16 ) ) ;
#19947 = VERTEX_POINT ( 'NONE', #34810 ) ;
#19948 = PLANE ( 'NONE',  #34987 ) ;
#19949 = CARTESIAN_POINT ( 'NONE',  ( -0.3862712429686809279, -1.188820645368943163, 10.00000000000000000 ) ) ;
#19950 = VECTOR ( 'NONE', #35177, 1000.000000000000000 ) ;
#19951 = ORIENTED_EDGE ( 'NONE', *, *, #32744, .F. ) ;
#19952 = EDGE_CURVE ( 'NONE', #2948, #49297, #23226, .T. ) ;
#19953 = ORIENTED_EDGE ( 'NONE', *, *, #20891, .T. ) ;
#19954 = EDGE_LOOP ( 'NONE', ( #50428, #29630, #26178, #8913 ) ) ;
#19955 = DIRECTION ( 'NONE',  ( -1.000000000000000000, -0.000000000000000000, -0.000000000000000000 ) ) ;
#19956 = VECTOR ( 'NONE', #18641, 1000.000000000000000 ) ;
#19957 = FACE_OUTER_BOUND ( 'NONE', #6775, .T. ) ;
#19958 = EDGE_LOOP ( 'NONE', ( #41749, #21724, #33703, #48790 ) ) ;
#19959 = CIRCLE ( 'NONE', #33098, 4.000000000000003553 ) ;
#19960 = CARTESIAN_POINT ( 'NONE',  ( -0.5107275442771143092, -1.175643901748072873, 9.976582533991681601 ) ) ;
#19961 = CARTESIAN_POINT ( 'NONE',  ( 214.9999999999999432, 164.9999999999999716, 500.0000000000000000 ) ) ;
#19962 = VECTOR ( 'NONE', #44316, 1000.000000000000000 ) ;
#19963 = CARTESIAN_POINT ( 'NONE',  ( 111.5540265531850679, 0.000000000000000000, -80.93171244307201562 ) ) ;
#19964 = EDGE_CURVE ( 'NONE', #25110, #10906, #25891, .T. ) ;
#19965 = DIRECTION ( 'NONE',  ( 3.172065745548403743E-16, 1.000000000000000000, 0.000000000000000000 ) ) ;
#19966 = CARTESIAN_POINT ( 'NONE',  ( 185.0000000000000000, 165.0000000000000000, -356.0000000000001705 ) ) ;
#19967 = EDGE_CURVE ( 'NONE', #2131, #34244, #34750, .T. ) ;
#19968 = CARTESIAN_POINT ( 'NONE',  ( -0.1083801931742817276, -1.382014125000175397, 9.960033073700733652 ) ) ;
#19969 = CARTESIAN_POINT ( 'NONE',  ( -1.081517186030697797, 0.5722085955955610315, 9.993783931180535873 ) ) ;
#19970 = FILL_AREA_STYLE_COLOUR ( '', #12816 ) ;
#19971 = CARTESIAN_POINT ( 'NONE',  ( -175.0000000000000000, 15.00000000000000000, -122.5000000000000000 ) ) ;
#19972 = ADVANCED_FACE ( 'NONE', ( #38397 ), #46542, .F. ) ;
#19973 = DIRECTION ( 'NONE',  ( 0.000000000000000000, 0.000000000000000000, -1.000000000000000000 ) ) ;
#19974 = FACE_OUTER_BOUND ( 'NONE', #6324, .T. ) ;
#19975 = EDGE_CURVE ( 'NONE', #49105, #10936, #23502, .T. ) ;
#19976 = EDGE_CURVE ( 'NONE', #37483, #16843, #41973, .T. ) ;
#19977 = DIRECTION ( 'NONE',  ( -0.000000000000000000, -0.000000000000000000, 1.000000000000000000 ) ) ;
#19978 = CARTESIAN_POINT ( 'NONE',  ( -0.9390173899430289683, -1.130417317737636651, 9.958264684458541183 ) ) ;
#19979 = VECTOR ( 'NONE', #32930, 1000.000000000000000 ) ;
#19980 = DIRECTION ( 'NONE',  ( 0.000000000000000000, 0.000000000000000000, 1.000000000000000000 ) ) ;
#19981 = DIRECTION ( 'NONE',  ( -0.000000000000000000, -0.000000000000000000, -1.000000000000000000 ) ) ;
#19982 = ORIENTED_EDGE ( 'NONE', *, *, #19742, .F. ) ;
#19983 = DIRECTION ( 'NONE',  ( 0.000000000000000000, -1.000000000000000000, 0.000000000000000000 ) ) ;
#19984 = EDGE_CURVE ( 'NONE', #16730, #49806, #3736, .T. ) ;
#19985 = LINE ( 'NONE', #47645, #41689 ) ;
#19986 = CARTESIAN_POINT ( 'NONE',  ( -165.0000000000000284, 16.00000000000000000, -84.99999999999998579 ) ) ;
#19987 = CARTESIAN_POINT ( 'NONE',  ( 0.1287570809895604018, 0.3962735484563146282, 10.00000000000000000 ) ) ;
#19988 = ORIENTED_EDGE ( 'NONE', *, *, #27216, .F. ) ;
#19989 = DIRECTION ( 'NONE',  ( -0.5038710255240859137, 0.000000000000000000, 0.8637789008984335659 ) ) ;
#19990 = ORIENTED_EDGE ( 'NONE', *, *, #15158, .T. ) ;
#19991 = VECTOR ( 'NONE', #12557, 1000.000000000000000 ) ;
#19992 = CARTESIAN_POINT ( 'NONE',  ( 16.99749102614301677, -1.320765928724307425, 8.953103998512858652 ) ) ;
#19993 = AXIS2_PLACEMENT_3D ( 'NONE', #34032, #49370, #25821 ) ;
#19994 = VERTEX_POINT ( 'NONE', #27342 ) ;
#19995 = CARTESIAN_POINT ( 'NONE',  ( 7.500000000000000000, 224.9999999999999716, -224.9999999999999716 ) ) ;
#19996 = AXIS2_PLACEMENT_3D ( 'NONE', #45647, #14626, #7453 ) ;
#19997 = CARTESIAN_POINT ( 'NONE',  ( -239.0000000000000853, -165.6999999999999602, 250.3600000000000136 ) ) ;
#19998 = CARTESIAN_POINT ( 'NONE',  ( -48.44597344681495343, 0.000000000000000000, 2.568287556927978166 ) ) ;
#19999 = ORIENTED_EDGE ( 'NONE', *, *, #14208, .F. ) ;
#20000 = CARTESIAN_POINT ( 'NONE',  ( 32.57170742938662755, 18.58316106410423174, 7.697694107796188234 ) ) ;
#20001 = ORIENTED_EDGE ( 'NONE', *, *, #45223, .T. ) ;
#20002 = AXIS2_PLACEMENT_3D ( 'NONE', #32066, #47657, #12547 ) ;
#20003 = ORIENTED_EDGE ( 'NONE', *, *, #48189, .F. ) ;
#20004 = DIRECTION ( 'NONE',  ( 0.000000000000000000, 0.000000000000000000, 1.000000000000000000 ) ) ;
#20005 = CARTESIAN_POINT ( 'NONE',  ( 71.55402655318505367, 0.000000000000000000, 165.0000000000000000 ) ) ;
#20006 = EDGE_LOOP ( 'NONE', ( #22544, #21166, #146, #43994, #42768 ) ) ;
#20007 = DIRECTION ( 'NONE',  ( 0.000000000000000000, 0.000000000000000000, 1.000000000000000000 ) ) ;
#20008 = LINE ( 'NONE', #43856, #50438 ) ;
#20009 = CYLINDRICAL_SURFACE ( 'NONE', #34782, 4.000000000000003553 ) ;
#20010 = FACE_OUTER_BOUND ( 'NONE', #38751, .T. ) ;
#20011 = EDGE_CURVE ( 'NONE', #20258, #2953, #42714, .T. ) ;
#20012 = CARTESIAN_POINT ( 'NONE',  ( -22.82242230425432439, 2.683863964738837371, 226.0000000000000000 ) ) ;
#20013 =( BOUNDED_CURVE ( )  B_SPLINE_CURVE ( 3, ( #39995, #35398, #4813, #20469 ),
 .UNSPECIFIED., .F., .F. ) 
 B_SPLINE_CURVE_WITH_KNOTS ( ( 4, 4 ),
 ( 0.000000000000000000, 1.570796326794896558 ),
 .UNSPECIFIED. ) 
 CURVE ( )  GEOMETRIC_REPRESENTATION_ITEM ( )  RATIONAL_B_SPLINE_CURVE ( ( 1.000000000000000000, 0.8047378541243649375, 0.8047378541243649375, 1.000000000000000000 ) ) 
 REPRESENTATION_ITEM ( '' )  );
#20014 = VECTOR ( 'NONE', #24093, 1000.000000000000000 ) ;
#20015 = ORIENTED_EDGE ( 'NONE', *, *, #40714, .T. ) ;
#20016 = DIRECTION ( 'NONE',  ( 1.000000000000000000, 0.000000000000000000, 0.000000000000000000 ) ) ;
#20017 = CARTESIAN_POINT ( 'NONE',  ( -210.0000000000000568, 0.000000000000000000, 40.81828755692798438 ) ) ;
#20018 = ORIENTED_EDGE ( 'NONE', *, *, #28962, .F. ) ;
#20019 = CARTESIAN_POINT ( 'NONE',  ( 193.3040265531851105, 1.750000000000009992, -159.1817124430720298 ) ) ;
#20020 =( BOUNDED_CURVE ( )  B_SPLINE_CURVE ( 3, ( #27551, #36016, #855, #20591 ),
 .UNSPECIFIED., .F., .F. ) 
 B_SPLINE_CURVE_WITH_KNOTS ( ( 4, 4 ),
 ( 4.712388980384689674, 6.283185307179586232 ),
 .UNSPECIFIED. ) 
 CURVE ( )  GEOMETRIC_REPRESENTATION_ITEM ( )  RATIONAL_B_SPLINE_CURVE ( ( 1.000000000000000000, 0.8047378541243649375, 0.8047378541243649375, 1.000000000000000000 ) ) 
 REPRESENTATION_ITEM ( '' )  );
#20021 = LINE ( 'NONE', #35192, #34151 ) ;
#20022 = VERTEX_POINT ( 'NONE', #154 ) ;
#20023 = CARTESIAN_POINT ( 'NONE',  ( 183.0000000000000000, 165.0000000000000000, -356.0000000000001705 ) ) ;
#20024 = DIRECTION ( 'NONE',  ( 0.000000000000000000, 0.000000000000000000, -1.000000000000000000 ) ) ;
#20025 = DIRECTION ( 'NONE',  ( -0.000000000000000000, -1.000000000000000000, -0.000000000000000000 ) ) ;
#20026 = DIRECTION ( 'NONE',  ( -1.000000000000000000, 0.000000000000000000, 1.860490536778032451E-50 ) ) ;
#20027 = EDGE_CURVE ( 'NONE', #27168, #47806, #6827, .T. ) ;
#20028 = ADVANCED_FACE ( 'NONE', ( #7859 ), #22474, .F. ) ;
#20029 = VERTEX_POINT ( 'NONE', #49860 ) ;
#20030 = VECTOR ( 'NONE', #32391, 1000.000000000000000 ) ;
#20031 = CARTESIAN_POINT ( 'NONE',  ( 0.000000000000000000, 183.0000000000000284, -344.0000000000001705 ) ) ;
#20032 = DIRECTION ( 'NONE',  ( -0.000000000000000000, -0.000000000000000000, -1.000000000000000000 ) ) ;
#20033 = CIRCLE ( 'NONE', #46176, 4.000000000000003553 ) ;
#20034 =( BOUNDED_CURVE ( )  B_SPLINE_CURVE ( 3, ( #3737, #50639, #15543, #46793 ),
 .UNSPECIFIED., .F., .F. ) 
 B_SPLINE_CURVE_WITH_KNOTS ( ( 4, 4 ),
 ( 0.000000000000000000, 0.5599187270832629570 ),
 .UNSPECIFIED. ) 
 CURVE ( )  GEOMETRIC_REPRESENTATION_ITEM ( )  RATIONAL_B_SPLINE_CURVE ( ( 1.000000000000000000, 0.9740444450880465510, 0.9740444450880465510, 1.000000000000000000 ) ) 
 REPRESENTATION_ITEM ( '' )  );
#20035 = ADVANCED_FACE ( 'NONE', ( #14778 ), #30431, .T. ) ;
#20036 = CARTESIAN_POINT ( 'NONE',  ( -11.73320209285699889, 11.96063479729179768, 9.403735324607438884 ) ) ;
#20037 = ORIENTED_EDGE ( 'NONE', *, *, #38254, .F. ) ;
#20038 = VECTOR ( 'NONE', #42981, 1000.000000000000000 ) ;
#20039 = ORIENTED_EDGE ( 'NONE', *, *, #32906, .F. ) ;
#20040 = EDGE_CURVE ( 'NONE', #9900, #27596, #46295, .T. ) ;
#20041 = CARTESIAN_POINT ( 'NONE',  ( 1251.690412480603527, 1456.903237050707276, 1414.757437540365117 ) ) ;
#20042 = EDGE_CURVE ( 'NONE', #15072, #49733, #15299, .T. ) ;
#20043 = CARTESIAN_POINT ( 'NONE',  ( -239.0000000000000853, -165.6999999999999602, 250.3600000000000136 ) ) ;
#20044 = CARTESIAN_POINT ( 'NONE',  ( -1.578643388466005160, 1.550786058692512182, 9.881002359080275355 ) ) ;
#20045 = CARTESIAN_POINT ( 'NONE',  ( -17.51065725283106289, 28.41934970907792746, -9.367992836599954742 ) ) ;
#20046 = CARTESIAN_POINT ( 'NONE',  ( 21.61731705588930907, 25.43568671410602278, -9.367992836599954742 ) ) ;
#20047 = VERTEX_POINT ( 'NONE', #7335 ) ;
#20048 = ADVANCED_FACE ( 'NONE', ( #27089 ), #11316, .T. ) ;
#20049 = DIRECTION ( 'NONE',  ( 0.000000000000000000, 0.000000000000000000, 1.000000000000000000 ) ) ;
#20050 = DIRECTION ( 'NONE',  ( 0.000000000000000000, 0.000000000000000000, 1.000000000000000000 ) ) ;
#20051 = LINE ( 'NONE', #19530, #29905 ) ;
#20052 = FACE_OUTER_BOUND ( 'NONE', #15044, .T. ) ;
#20053 = ORIENTED_EDGE ( 'NONE', *, *, #44960, .T. ) ;
#20054 = AXIS2_PLACEMENT_3D ( 'NONE', #7817, #19081, #11913 ) ;
#20055 = CARTESIAN_POINT ( 'NONE',  ( 191.5540265531850537, -1.025126265847089657, 119.0682875569279560 ) ) ;
#20056 = ORIENTED_EDGE ( 'NONE', *, *, #10149, .T. ) ;
#20057 = CARTESIAN_POINT ( 'NONE',  ( -9.999999999999994671, 2.168404344971008375E-16, 8.340239149799208107 ) ) ;
#20058 = VECTOR ( 'NONE', #38252, 1000.000000000000000 ) ;
#20059 = VERTEX_POINT ( 'NONE', #24768 ) ;
#20060 = DIRECTION ( 'NONE',  ( -1.000000000000000000, -0.000000000000000000, -0.000000000000000000 ) ) ;
#20061 = DIRECTION ( 'NONE',  ( -1.000000000000000000, 0.000000000000000000, 0.000000000000000000 ) ) ;
#20062 = CARTESIAN_POINT ( 'NONE',  ( -206.6959734468149463, -1.750000000000010214, -39.18171244307202983 ) ) ;
#20063 = VERTEX_POINT ( 'NONE', #16808 ) ;
#20064 = CARTESIAN_POINT ( 'NONE',  ( 0.3965304326644019106, -0.1288405477284165490, 9.992737347336296594 ) ) ;
#20065 = DIRECTION ( 'NONE',  ( -0.000000000000000000, -1.000000000000000000, -0.000000000000000000 ) ) ;
#20066 = ORIENTED_EDGE ( 'NONE', *, *, #49509, .T. ) ;
#20067 = DIRECTION ( 'NONE',  ( 0.000000000000000000, -0.9602398687205827565, -0.2791762785758810650 ) ) ;
#20068 = AXIS2_PLACEMENT_3D ( 'NONE', #2960, #33786, #38149 ) ;
#20069 = CARTESIAN_POINT ( 'NONE',  ( -128.4459734468149179, 0.000000000000000000, -165.0000000000000000 ) ) ;
#20070 = DIRECTION ( 'NONE',  ( -0.000000000000000000, -0.000000000000000000, -1.000000000000000000 ) ) ;
#20071 = LINE ( 'NONE', #47235, #36522 ) ;
#20072 = ADVANCED_FACE ( 'NONE', ( #44234 ), #12443, .T. ) ;
#20073 = ORIENTED_EDGE ( 'NONE', *, *, #16218, .T. ) ;
#20074 = EDGE_LOOP ( 'NONE', ( #24263, #49383, #32703, #48856 ) ) ;
#20075 = CARTESIAN_POINT ( 'NONE',  ( 84.99999999999997158, 17.00000000000000000, -90.00000000000000000 ) ) ;
#20076 = EDGE_CURVE ( 'NONE', #12440, #20059, #27609, .T. ) ;
#20077 = ORIENTED_EDGE ( 'NONE', *, *, #19663, .F. ) ;
#20078 = CARTESIAN_POINT ( 'NONE',  ( -126.6959734468149321, -1.749999999999997335, -119.1817124430720440 ) ) ;
#20079 = LINE ( 'NONE', #4431, #7910 ) ;
#20080 = CARTESIAN_POINT ( 'NONE',  ( -126.6959734468149321, 0.000000000000000000, 165.0000000000000000 ) ) ;
#20081 = ORIENTED_EDGE ( 'NONE', *, *, #2658, .T. ) ;
#20082 = CARTESIAN_POINT ( 'NONE',  ( -50.00000000000000000, 50.00000000000000000, 800.0000000000000000 ) ) ;
#20083 = ORIENTED_EDGE ( 'NONE', *, *, #24045, .T. ) ;
#20084 = DIRECTION ( 'NONE',  ( -1.000000000000000000, 0.000000000000000000, 0.000000000000000000 ) ) ;
#20085 = DIRECTION ( 'NONE',  ( 1.132880637372608740E-16, 4.718402560806925739E-50, 1.000000000000000000 ) ) ;
#20086 = AXIS2_PLACEMENT_3D ( 'NONE', #9400, #40955, #44776 ) ;
#20087 = ORIENTED_EDGE ( 'NONE', *, *, #33668, .T. ) ;
#20088 = VERTEX_POINT ( 'NONE', #43988 ) ;
#20089 = EDGE_LOOP ( 'NONE', ( #36106, #47571, #3995, #27071 ) ) ;
#20090 = VECTOR ( 'NONE', #16146, 1000.000000000000000 ) ;
#20091 = CARTESIAN_POINT ( 'NONE',  ( -21.24469349090191983, -33.89193117067290473, 910.0000000000000000 ) ) ;
#20092 = LINE ( 'NONE', #8559, #21790 ) ;
#20093 = CARTESIAN_POINT ( 'NONE',  ( -204.9459734468149463, 2.143131898507880377E-16, -157.4317124430720582 ) ) ;
#20094 = PRODUCT_DEFINITION_CONTEXT ( 'detailed design', #30246, 'design' ) ;
#20095 = ORIENTED_EDGE ( 'NONE', *, *, #44628, .T. ) ;
#20096 = LINE ( 'NONE', #16007, #50120 ) ;
#20097 = ORIENTED_EDGE ( 'NONE', *, *, #31784, .T. ) ;
#20098 = CARTESIAN_POINT ( 'NONE',  ( -28.96803024440907137, -18.11533787072017176, 7.455576670931136185 ) ) ;
#20099 = ORIENTED_EDGE ( 'NONE', *, *, #46152, .F. ) ;
#20100 = AXIS2_PLACEMENT_3D ( 'NONE', #17519, #29827, #33191 ) ;
#20101 = DIRECTION ( 'NONE',  ( 1.000000000000000000, 0.000000000000000000, -1.612977847700450206E-50 ) ) ;
#20102 = LINE ( 'NONE', #20354, #36808 ) ;
#20103 = PRESENTATION_STYLE_ASSIGNMENT (( #34832 ) ) ;
#20104 = VECTOR ( 'NONE', #28875, 1000.000000000000114 ) ;
#20105 = CARTESIAN_POINT ( 'NONE',  ( 1.066995270233474624, -50.00000000000000711, -3.760136334089591248 ) ) ;
#20106 = AXIS2_PLACEMENT_3D ( 'NONE', #46375, #49700, #2787 ) ;
#20107 = ORIENTED_EDGE ( 'NONE', *, *, #37768, .T. ) ;
#20108 = VERTEX_POINT ( 'NONE', #40419 ) ;
#20109 = EDGE_CURVE ( 'NONE', #26847, #44300, #5252, .T. ) ;
#20110 = CARTESIAN_POINT ( 'NONE',  ( -64.99999999999940314, 17.00000000000000000, -54.99999999999999289 ) ) ;
#20111 = CARTESIAN_POINT ( 'NONE',  ( -9.483938762529191990, 3.217310375392813615, 3.215106848023462138 ) ) ;
#20112 = DIRECTION ( 'NONE',  ( -1.000000000000000000, 0.000000000000000000, -0.000000000000000000 ) ) ;
#20113 = VECTOR ( 'NONE', #35707, 1000.000000000000000 ) ;
#20114 = DIRECTION ( 'NONE',  ( 0.000000000000000000, -0.000000000000000000, 1.000000000000000000 ) ) ;
#20115 =( BOUNDED_CURVE ( )  B_SPLINE_CURVE ( 3, ( #17854, #33521, #22219, #26574 ),
 .UNSPECIFIED., .F., .F. ) 
 B_SPLINE_CURVE_WITH_KNOTS ( ( 4, 4 ),
 ( 4.712388980384710990, 6.283185307179309120 ),
 .UNSPECIFIED. ) 
 CURVE ( )  GEOMETRIC_REPRESENTATION_ITEM ( )  RATIONAL_B_SPLINE_CURVE ( ( 1.000000000000000000, 0.8047378541243699335, 0.8047378541243699335, 1.000000000000000000 ) ) 
 REPRESENTATION_ITEM ( '' )  );
#20116 = CARTESIAN_POINT ( 'NONE',  ( 356.0000000000000000, 174.9999999999996589, -344.0000000000002842 ) ) ;
#20117 = ORIENTED_EDGE ( 'NONE', *, *, #23029, .T. ) ;
#20118 = LINE ( 'NONE', #23725, #45030 ) ;
#20119 = CARTESIAN_POINT ( 'NONE',  ( 210.0000000000000568, 0.000000000000000000, -159.1817124430720298 ) ) ;
#20120 = ORIENTED_EDGE ( 'NONE', *, *, #50609, .F. ) ;
#20121 = AXIS2_PLACEMENT_3D ( 'NONE', #49043, #1403, #13929 ) ;
#20122 = CARTESIAN_POINT ( 'NONE',  ( -50.00000000000000000, -50.00000000000000000, 900.0000000000000000 ) ) ;
#20123 = VECTOR ( 'NONE', #8420, 1000.000000000000000 ) ;
#20124 = CARTESIAN_POINT ( 'NONE',  ( -166.6959734468149463, 1.750000000000010214, 40.81828755692798438 ) ) ;
#20125 = CARTESIAN_POINT ( 'NONE',  ( 0.000000000000000000, 181.0000000000000284, 359.9999999999997726 ) ) ;
#20126 = CIRCLE ( 'NONE', #37346, 0.4999999999999997224 ) ;
#20127 = ORIENTED_EDGE ( 'NONE', *, *, #2980, .F. ) ;
#20128 = ORIENTED_EDGE ( 'NONE', *, *, #13650, .T. ) ;
#20129 = DIRECTION ( 'NONE',  ( 0.000000000000000000, -1.000000000000000000, 0.000000000000000000 ) ) ;
#20130 = CARTESIAN_POINT ( 'NONE',  ( 47.23269937569327226, -16.43609759007049931, -2.408242355805840784 ) ) ;
#20131 = AXIS2_PLACEMENT_3D ( 'NONE', #7146, #10990, #23287 ) ;
#20132 = ORIENTED_EDGE ( 'NONE', *, *, #193, .F. ) ;
#20133 = ORIENTED_EDGE ( 'NONE', *, *, #45592, .T. ) ;
#20134 = CARTESIAN_POINT ( 'NONE',  ( 1.040834085586084257E-14, -6.912230148066169200, 5.000000000000000000 ) ) ;
#20135 = CARTESIAN_POINT ( 'NONE',  ( 6.408332700304398166, 7.676800896350598258, 0.000000000000000000 ) ) ;
#20136 = CARTESIAN_POINT ( 'NONE',  ( 34.95136153415558056, -36.40974830873469870, 8.356839323120299312 ) ) ;
#20137 = CARTESIAN_POINT ( 'NONE',  ( -204.9459734468148895, -1.025126265847089213, 42.56828755692799149 ) ) ;
#20138 = CARTESIAN_POINT ( 'NONE',  ( -86.69597344681496054, 0.000000000000000000, -165.0000000000000000 ) ) ;
#20139 = AXIS2_PLACEMENT_3D ( 'NONE', #13709, #25515, #6009 ) ;
#20140 = ORIENTED_EDGE ( 'NONE', *, *, #42232, .T. ) ;
#20141 = VERTEX_POINT ( 'NONE', #918 ) ;
#20142 = ORIENTED_EDGE ( 'NONE', *, *, #11749, .T. ) ;
#20143 = VECTOR ( 'NONE', #16832, 1000.000000000000000 ) ;
#20144 = AXIS2_PLACEMENT_3D ( 'NONE', #47796, #32457, #43973 ) ;
#20145 = CARTESIAN_POINT ( 'NONE',  ( 210.0000000000000568, 2.143131898507881856E-16, 119.0682875569279560 ) ) ;
#20146 = ORIENTED_EDGE ( 'NONE', *, *, #3241, .T. ) ;
#20147 = LINE ( 'NONE', #42719, #2503 ) ;
#20148 = ORIENTED_EDGE ( 'NONE', *, *, #32213, .F. ) ;
#20149 = ORIENTED_EDGE ( 'NONE', *, *, #3088, .F. ) ;
#20150 = FACE_OUTER_BOUND ( 'NONE', #38593, .T. ) ;
#20151 = CARTESIAN_POINT ( 'NONE',  ( -18.67411147745623978, -27.51799019669813973, -3.760136334089591248 ) ) ;
#20152 = DIRECTION ( 'NONE',  ( -4.758098676964956461E-16, -1.000000000000000000, 0.000000000000000000 ) ) ;
#20153 = EDGE_LOOP ( 'NONE', ( #26197, #22486, #902, #17165 ) ) ;
#20154 = ORIENTED_EDGE ( 'NONE', *, *, #6024, .F. ) ;
#20155 = DIRECTION ( 'NONE',  ( -1.000000000000000000, -0.000000000000000000, -0.000000000000000000 ) ) ;
#20156 = FACE_OUTER_BOUND ( 'NONE', #34154, .T. ) ;
#20157 = ORIENTED_EDGE ( 'NONE', *, *, #30569, .T. ) ;
#20158 = VECTOR ( 'NONE', #38518, 1000.000000000000000 ) ;
#20159 = CARTESIAN_POINT ( 'NONE',  ( 339.9999999999998863, -180.9999999999999716, 355.9999999999997726 ) ) ;
#20160 = CARTESIAN_POINT ( 'NONE',  ( -5.000000000000000000, 175.0000000000000284, 353.7500000000001705 ) ) ;
#20161 = CARTESIAN_POINT ( 'NONE',  ( 185.0000000000000284, -174.9999999999999716, -111.0000000000001563 ) ) ;
#20162 = DIRECTION ( 'NONE',  ( -0.000000000000000000, -1.000000000000000000, -0.000000000000000000 ) ) ;
#20163 = VECTOR ( 'NONE', #18124, 1000.000000000000114 ) ;
#20164 = ORIENTED_EDGE ( 'NONE', *, *, #34914, .F. ) ;
#20165 = EDGE_CURVE ( 'NONE', #1474, #14334, #23751, .T. ) ;
#20166 = CARTESIAN_POINT ( 'NONE',  ( -19.99999999999878142, 17.00000000000000000, 30.00000000000000000 ) ) ;
#20167 = CARTESIAN_POINT ( 'NONE',  ( -48.44597344681496054, 1.025126265847089657, -80.93171244307201562 ) ) ;
#20168 = LINE ( 'NONE', #16834, #44915 ) ;
#20169 = EDGE_CURVE ( 'NONE', #12891, #38992, #28600, .T. ) ;
#20170 = CARTESIAN_POINT ( 'NONE',  ( 0.3862712429686978033, -1.188820645368937834, -10.00000000000000000 ) ) ;
#20171 = EDGE_CURVE ( 'NONE', #7456, #36951, #32475, .T. ) ;
#20172 =( BOUNDED_CURVE ( )  B_SPLINE_CURVE ( 3, ( #18744, #31341, #15424, #19508 ),
 .UNSPECIFIED., .F., .F. ) 
 B_SPLINE_CURVE_WITH_KNOTS ( ( 4, 4 ),
 ( 3.141592653589793116, 4.712388980384689674 ),
 .UNSPECIFIED. ) 
 CURVE ( )  GEOMETRIC_REPRESENTATION_ITEM ( )  RATIONAL_B_SPLINE_CURVE ( ( 1.000000000000000000, 0.8047378541243649375, 0.8047378541243649375, 1.000000000000000000 ) ) 
 REPRESENTATION_ITEM ( '' )  );
#20173=STYLED_ITEM('',(#50747),#22072);
#20174 = LINE ( 'NONE', #28391, #3208 ) ;
#20175 = EDGE_CURVE ( 'NONE', #26183, #45274, #43238, .T. ) ;
#20176 =( BOUNDED_CURVE ( )  B_SPLINE_CURVE ( 3, ( #26371, #37437, #13546, #29460 ),
 .UNSPECIFIED., .F., .F. ) 
 B_SPLINE_CURVE_WITH_KNOTS ( ( 4, 4 ),
 ( 0.000000000000000000, 1.570796326794896558 ),
 .UNSPECIFIED. ) 
 CURVE ( )  GEOMETRIC_REPRESENTATION_ITEM ( )  RATIONAL_B_SPLINE_CURVE ( ( 1.000000000000000000, 0.8047378541243649375, 0.8047378541243649375, 1.000000000000000000 ) ) 
 REPRESENTATION_ITEM ( '' )  );
#20177 = ADVANCED_FACE ( 'NONE', ( #39417 ), #47809, .F. ) ;
#20178 = CARTESIAN_POINT ( 'NONE',  ( -1.593403307199984020, -0.6097984806593539364, 9.912102921405034905 ) ) ;
#20179 = DIRECTION ( 'NONE',  ( 0.000000000000000000, -0.3790464617558786942, 0.9253776417389547593 ) ) ;
#20180 = VECTOR ( 'NONE', #7525, 1000.000000000000000 ) ;
#20181 = EDGE_CURVE ( 'NONE', #14015, #14684, #14030, .T. ) ;
#20182 = ORIENTED_EDGE ( 'NONE', *, *, #10622, .T. ) ;
#20183 = LINE ( 'NONE', #24306, #14163 ) ;
#20184 = CARTESIAN_POINT ( 'NONE',  ( 0.3147652639080171233, -1.255102005797306575, 9.947020512645400103 ) ) ;
#20185 = ORIENTED_EDGE ( 'NONE', *, *, #18328, .T. ) ;
#20186 = FACE_OUTER_BOUND ( 'NONE', #16917, .T. ) ;
#20187 = CARTESIAN_POINT ( 'NONE',  ( 73.30402655318508209, -1.750000000000010658, -79.18171244307201562 ) ) ;
#20188 = DIRECTION ( 'NONE',  ( 0.5877852522924743583, -0.8090169943749466741, 0.000000000000000000 ) ) ;
#20189 = ORIENTED_EDGE ( 'NONE', *, *, #11528, .T. ) ;
#20190 = CARTESIAN_POINT ( 'NONE',  ( 111.5540265531850679, 0.000000000000000000, 122.5682875569279560 ) ) ;
#20191 = EDGE_CURVE ( 'NONE', #24864, #14077, #15690, .T. ) ;
#20193 = VERTEX_POINT ( 'NONE', #47308 ) ;
#20192 = EDGE_CURVE ( 'NONE', #23599, #3803, #48055, .T. ) ;
#20194 = ORIENTED_EDGE ( 'NONE', *, *, #23938, .T. ) ;
#20195 = PLANE ( 'NONE',  #36591 ) ;
#20196 = CARTESIAN_POINT ( 'NONE',  ( -8.445973446814964092, 1.025126265847097429, 79.06828755692792754 ) ) ;
#20197 = EDGE_CURVE ( 'NONE', #24185, #31089, #20978, .T. ) ;
#20198 = ADVANCED_FACE ( 'NONE', ( #16303 ), #4750, .T. ) ;
#20199 = AXIS2_PLACEMENT_3D ( 'NONE', #31132, #38079, #50572 ) ;
#20200 = VERTEX_POINT ( 'NONE', #6004 ) ;
#20201 = LINE ( 'NONE', #48108, #21321 ) ;
#20202 = FACE_OUTER_BOUND ( 'NONE', #3279, .T. ) ;
#20203 = VECTOR ( 'NONE', #33239, 1000.000000000000000 ) ;
#20204 = ORIENTED_EDGE ( 'NONE', *, *, #28961, .T. ) ;
#20205 = ADVANCED_FACE ( 'NONE', ( #48565 ), #49065, .T. ) ;
#20206 = EDGE_CURVE ( 'NONE', #10704, #28357, #33233, .T. ) ;
#20207 = CYLINDRICAL_SURFACE ( 'NONE', #41531, 1.750000000000001554 ) ;
#20208 = ORIENTED_EDGE ( 'NONE', *, *, #8704, .F. ) ;
#20209 = DIRECTION ( 'NONE',  ( -1.000000000000000000, -0.000000000000000000, -0.000000000000000000 ) ) ;
#20210 = FACE_OUTER_BOUND ( 'NONE', #25214, .T. ) ;
#20211 = CARTESIAN_POINT ( 'NONE',  ( 1.011271242968688311, -0.7347315653655855927, -3.333333333333333481 ) ) ;
#20212 = EDGE_LOOP ( 'NONE', ( #23510, #7646, #32441, #29445 ) ) ;
#20213 = CARTESIAN_POINT ( 'NONE',  ( 11.73320209285708415, -11.96063479729170886, 9.403735324607438884 ) ) ;
#20214 = DIRECTION ( 'NONE',  ( -0.000000000000000000, -1.000000000000000000, -0.000000000000000000 ) ) ;
#20215 = ORIENTED_EDGE ( 'NONE', *, *, #2047, .F. ) ;
#20216 = ORIENTED_EDGE ( 'NONE', *, *, #48614, .F. ) ;
#20217 = VERTEX_POINT ( 'NONE', #21402 ) ;
#20218 = LINE ( 'NONE', #25085, #24598 ) ;
#20219 = CARTESIAN_POINT ( 'NONE',  ( 5.551115123125782702E-14, -168.9999999999999432, 355.9999999999997726 ) ) ;
#20220 = ORIENTED_EDGE ( 'NONE', *, *, #45836, .T. ) ;
#20221 = EDGE_CURVE ( 'NONE', #7107, #6771, #5503, .T. ) ;
#20222 = CIRCLE ( 'NONE', #9564, 2.000000000000001776 ) ;
#20223 = DIRECTION ( 'NONE',  ( 1.000000000000000000, -4.758098676964956461E-16, -8.975803739141899931E-48 ) ) ;
#20224 = CARTESIAN_POINT ( 'NONE',  ( 183.0000000000000000, 175.0000000000000284, -356.0000000000001705 ) ) ;
#20225 = FACE_OUTER_BOUND ( 'NONE', #29854, .T. ) ;
#20226 = EDGE_CURVE ( 'NONE', #38090, #42902, #18055, .T. ) ;
#20227 = DIRECTION ( 'NONE',  ( -1.000000000000000000, 0.000000000000000000, 3.469446951953611724E-16 ) ) ;
#20228 = CARTESIAN_POINT ( 'NONE',  ( 167.0000000000000000, -180.9999999999999716, -115.0000000000001563 ) ) ;
#20229 = EDGE_CURVE ( 'NONE', #50192, #29738, #13945, .T. ) ;
#20230 = CARTESIAN_POINT ( 'NONE',  ( 151.5540265531850537, 0.000000000000000000, 159.0682875569279702 ) ) ;
#20231 = CARTESIAN_POINT ( 'NONE',  ( -168.4459734468149463, 0.000000000000000000, 165.0000000000000000 ) ) ;
#20232 = DIRECTION ( 'NONE',  ( -0.6805276818820470419, 0.4944323023721968191, -0.5407575913134976542 ) ) ;
#20233 = CARTESIAN_POINT ( 'NONE',  ( 151.5540265531850537, 0.000000000000000000, 42.56828755692798438 ) ) ;
#20234 = DIRECTION ( 'NONE',  ( 1.000000000000000000, 0.000000000000000000, -0.000000000000000000 ) ) ;
#20235 = DIRECTION ( 'NONE',  ( 0.000000000000000000, -0.000000000000000000, -1.000000000000000000 ) ) ;
#20236 = EDGE_CURVE ( 'NONE', #27759, #42182, #21656, .T. ) ;
#20237 = CARTESIAN_POINT ( 'NONE',  ( 210.0000000000000568, 0.000000000000000000, 0.8182875569279768335 ) ) ;
#20238 = VECTOR ( 'NONE', #25078, 1000.000000000000000 ) ;
#20239 = LINE ( 'NONE', #39502, #3501 ) ;
#20240 = ORIENTED_EDGE ( 'NONE', *, *, #16472, .T. ) ;
#20241 = CARTESIAN_POINT ( 'NONE',  ( 350.0000000000001137, 169.0000000000000000, 341.9999999999997726 ) ) ;
#20242 = CARTESIAN_POINT ( 'NONE',  ( 115.0540265531850395, 2.143131898507847836E-16, 165.0000000000000000 ) ) ;
#20243 = DIRECTION ( 'NONE',  ( 0.000000000000000000, 0.000000000000000000, 1.000000000000000000 ) ) ;
#20244 = CARTESIAN_POINT ( 'NONE',  ( 31.28234235046230793, 11.28615439405779064, -3.760136334089591248 ) ) ;
#20245 = EDGE_CURVE ( 'NONE', #12842, #13365, #42208, .T. ) ;
#20246 = ORIENTED_EDGE ( 'NONE', *, *, #50617, .T. ) ;
#20247 = FACE_OUTER_BOUND ( 'NONE', #19767, .T. ) ;
#20248 = B_SPLINE_CURVE_WITH_KNOTS ( 'NONE', 3,
 ( #34781, #30927, #7565, #17023 ),
 .UNSPECIFIED., .F., .F.,
 ( 4, 4 ),
 ( 0.001937412222931638979, 0.003978261222109142140 ),
 .UNSPECIFIED. ) ;
#20249 = DIRECTION ( 'NONE',  ( 0.000000000000000000, 0.000000000000000000, 1.000000000000000000 ) ) ;
#20250 = ADVANCED_FACE ( 'NONE', ( #36837 ), #29614, .T. ) ;
#20251 = ORIENTED_EDGE ( 'NONE', *, *, #19090, .T. ) ;
#20252 = PLANE ( 'NONE',  #16464 ) ;
#20253 = CARTESIAN_POINT ( 'NONE',  ( -1.267276237729528798, 0.08162529406826846134, 9.975314328424614629 ) ) ;
#20254 = CARTESIAN_POINT ( 'NONE',  ( -36.28567981536816234, -9.465698090293395595, -9.422646554964174470 ) ) ;
#20255 = ORIENTED_EDGE ( 'NONE', *, *, #15140, .F. ) ;
#20256 = DIRECTION ( 'NONE',  ( -1.000000000000000000, 0.000000000000000000, 0.000000000000000000 ) ) ;
#20257 = ORIENTED_EDGE ( 'NONE', *, *, #40000, .T. ) ;
#20258 = VERTEX_POINT ( 'NONE', #1917 ) ;
#20259 = EDGE_CURVE ( 'NONE', #1207, #20650, #40650, .T. ) ;
#20260 = EDGE_CURVE ( 'NONE', #32080, #8986, #32713, .T. ) ;
#20261 = ORIENTED_EDGE ( 'NONE', *, *, #11230, .T. ) ;
#20262 = CARTESIAN_POINT ( 'NONE',  ( 72.27890028733797578, 1.750000000000010436, 79.79316129108087807 ) ) ;
#20263 = CARTESIAN_POINT ( 'NONE',  ( -205.6708471809678827, 1.750000000000010214, 121.8434138227750623 ) ) ;
#20264 = ORIENTED_EDGE ( 'NONE', *, *, #44586, .F. ) ;
#20265 = DIRECTION ( 'NONE',  ( 0.000000000000000000, 0.000000000000000000, -1.000000000000000000 ) ) ;
#20266 = CARTESIAN_POINT ( 'NONE',  ( 46.76852358249013264, -17.86468378716708827, -9.367992836599951190 ) ) ;
#20267 = ADVANCED_FACE ( 'NONE', ( #2172 ), #6510, .F. ) ;
#20268 = CARTESIAN_POINT ( 'NONE',  ( 181.0000000000000000, 10.00000000000006395, -340.0000000000001137 ) ) ;
#20269 = ADVANCED_FACE ( 'NONE', ( #29866 ), #32978, .T. ) ;
#20270 = DIRECTION ( 'NONE',  ( 0.000000000000000000, 0.000000000000000000, 1.000000000000000000 ) ) ;
#20271 = VERTEX_POINT ( 'NONE', #45482 ) ;
#20272 = EDGE_CURVE ( 'NONE', #47971, #29800, #13201, .T. ) ;
#20273 = FACE_OUTER_BOUND ( 'NONE', #18879, .T. ) ;
#20274 = ORIENTED_EDGE ( 'NONE', *, *, #48358, .F. ) ;
#20275 = AXIS2_PLACEMENT_3D ( 'NONE', #24861, #44571, #44087 ) ;
#20276 = LINE ( 'NONE', #40784, #16914 ) ;
#20277 = CARTESIAN_POINT ( 'NONE',  ( -64.99999999999783995, 16.00000000000000000, 115.0000000000000142 ) ) ;
#20278 = EDGE_LOOP ( 'NONE', ( #35823, #696, #5495 ) ) ;
#20279 = LINE ( 'NONE', #3866, #29223 ) ;
#20280 = ORIENTED_EDGE ( 'NONE', *, *, #6052, .T. ) ;
#20281 = CARTESIAN_POINT ( 'NONE',  ( -46.69597344681494633, 1.750000000000010658, 80.81828755692798438 ) ) ;
#20282 = CARTESIAN_POINT ( 'NONE',  ( -0.1287570809895632329, 0.3962735484563137400, -10.00000000000000000 ) ) ;
#20283 = DIRECTION ( 'NONE',  ( -0.000000000000000000, -0.000000000000000000, -1.000000000000000000 ) ) ;
#20284 = CARTESIAN_POINT ( 'NONE',  ( -86.69597344681494633, -1.750000000000009992, 0.8182875569279768335 ) ) ;
#20285 = EDGE_CURVE ( 'NONE', #20108, #23722, #9360, .T. ) ;
#20286 = EDGE_LOOP ( 'NONE', ( #17532, #23944, #7809, #39762 ) ) ;
#20287 = LINE ( 'NONE', #47192, #10560 ) ;
#20288 = FACE_OUTER_BOUND ( 'NONE', #39606, .T. ) ;
#20289 = CARTESIAN_POINT ( 'NONE',  ( -24.47767542868268364, 23.18653802921800278, 8.807470649214879543 ) ) ;
#20290 = EDGE_LOOP ( 'NONE', ( #22304, #340, #12655, #17815 ) ) ;
#20291 = ORIENTED_EDGE ( 'NONE', *, *, #21387, .F. ) ;
#20292 = APPLICATION_PROTOCOL_DEFINITION ( 'draft international standard', 'automotive_design', 1998, #38126 ) ;
#20293 = DIRECTION ( 'NONE',  ( -1.586032892321651989E-16, -1.194346094642793337E-32, -1.000000000000000000 ) ) ;
#20294 = PLANE ( 'NONE',  #33265 ) ;
#20295 = FACE_OUTER_BOUND ( 'NONE', #7270, .T. ) ;
#20296 = CARTESIAN_POINT ( 'NONE',  ( -5.000000000000000000, 165.2000000000000171, -340.2000000000001592 ) ) ;
#20297 = CARTESIAN_POINT ( 'NONE',  ( -84.94597344681494633, 2.143131898507880377E-16, -117.4317124430720725 ) ) ;
#20298 = VERTEX_POINT ( 'NONE', #25259 ) ;
#20299 = LINE ( 'NONE', #1059, #10810 ) ;
#20300 = ADVANCED_FACE ( 'NONE', ( #40913 ), #5752, .T. ) ;
#20301 = DIRECTION ( 'NONE',  ( -1.000000000000000000, 0.000000000000000000, 0.000000000000000000 ) ) ;
#20302 = CARTESIAN_POINT ( 'NONE',  ( 2.143303251558809297, -0.2857918750720293000, 9.885585981620947038 ) ) ;
#20303 = CYLINDRICAL_SURFACE ( 'NONE', #237, 1.750000000000036193 ) ;
#20304 = VERTEX_POINT ( 'NONE', #41917 ) ;
#20305 = DIRECTION ( 'NONE',  ( -0.000000000000000000, -1.000000000000000000, -0.000000000000000000 ) ) ;
#20306 = ORIENTED_EDGE ( 'NONE', *, *, #23938, .F. ) ;
#20307 = CARTESIAN_POINT ( 'NONE',  ( 34.95136153415558056, -36.40974830873469870, 8.356839323120299312 ) ) ;
#20308 = ORIENTED_EDGE ( 'NONE', *, *, #12660, .F. ) ;
#20309 = CARTESIAN_POINT ( 'NONE',  ( 155.0540265531850537, 2.143131898507880377E-16, 119.0682875569279702 ) ) ;
#20310 = CARTESIAN_POINT ( 'NONE',  ( -6.695973446814940111, 1.750000000000023759, -39.18171244307202983 ) ) ;
#20311 = CARTESIAN_POINT ( 'NONE',  ( 183.0000000000000000, -272.5000000000000000, -111.0000000000001563 ) ) ;
#20312 = CYLINDRICAL_SURFACE ( 'NONE', #10776, 1.750000000000001554 ) ;
#20313 = ORIENTED_EDGE ( 'NONE', *, *, #1844, .F. ) ;
#20314 =( BOUNDED_CURVE ( )  B_SPLINE_CURVE ( 3, ( #9874, #9125, #1437, #25276 ),
 .UNSPECIFIED., .F., .F. ) 
 B_SPLINE_CURVE_WITH_KNOTS ( ( 4, 4 ),
 ( 1.570796326794896558, 3.141592653589793116 ),
 .UNSPECIFIED. ) 
 CURVE ( )  GEOMETRIC_REPRESENTATION_ITEM ( )  RATIONAL_B_SPLINE_CURVE ( ( 1.000000000000000000, 0.8047378541243649375, 0.8047378541243649375, 1.000000000000000000 ) ) 
 REPRESENTATION_ITEM ( '' )  );
#20315 = EDGE_CURVE ( 'NONE', #4748, #19163, #11374, .T. ) ;
#20316 = CARTESIAN_POINT ( 'NONE',  ( 27.33593271309472073, -41.94268121623323253, -9.367992836599951190 ) ) ;
#20317 = EDGE_CURVE ( 'NONE', #46590, #2507, #19324, .T. ) ;
#20318 = DIRECTION ( 'NONE',  ( 1.000000000000000000, 0.000000000000000000, -1.860490536778032451E-50 ) ) ;
#20319 = VERTEX_POINT ( 'NONE', #3672 ) ;
#20320 = CARTESIAN_POINT ( 'NONE',  ( -6.695973446814940111, 1.750000000000023315, 0.8182875569279768335 ) ) ;
#20321 = CYLINDRICAL_SURFACE ( 'NONE', #17505, 1.750000000000008438 ) ;
#20322 = CARTESIAN_POINT ( 'NONE',  ( -36.97942854200451990, 6.226705766838657397, 8.914903342594564961 ) ) ;
#20323 = DIRECTION ( 'NONE',  ( 0.000000000000000000, 0.000000000000000000, 1.000000000000000000 ) ) ;
#20324 =( BOUNDED_CURVE ( )  B_SPLINE_CURVE ( 3, ( #38923, #34555, #3749, #35084 ),
 .UNSPECIFIED., .F., .F. ) 
 B_SPLINE_CURVE_WITH_KNOTS ( ( 4, 4 ),
 ( 5.723266580096323608, 6.843104034262848856 ),
 .UNSPECIFIED. ) 
 CURVE ( )  GEOMETRIC_REPRESENTATION_ITEM ( )  RATIONAL_B_SPLINE_CURVE ( ( 1.000000000000000000, 0.8981988528445483677, 0.8981988528445483677, 1.000000000000000000 ) ) 
 REPRESENTATION_ITEM ( '' )  );
#20325 = ORIENTED_EDGE ( 'NONE', *, *, #4090, .F. ) ;
#20326 = EDGE_CURVE ( 'NONE', #7888, #2228, #30120, .T. ) ;
#20327 = ORIENTED_EDGE ( 'NONE', *, *, #17782, .F. ) ;
#20328 = DIRECTION ( 'NONE',  ( 0.000000000000000000, 0.000000000000000000, -1.000000000000000000 ) ) ;
#20329 = EDGE_CURVE ( 'NONE', #25250, #37586, #22580, .T. ) ;
#20330 = EDGE_CURVE ( 'NONE', #31946, #18303, #33975, .T. ) ;
#20331 = ORIENTED_EDGE ( 'NONE', *, *, #29114, .T. ) ;
#20332 = CARTESIAN_POINT ( 'NONE',  ( 0.5953091702432292687, 3.900377598923890243, 6.494306381704024744 ) ) ;
#20333 = CARTESIAN_POINT ( 'NONE',  ( 168.9999999999999716, 174.9999999999999716, -340.0000000000001137 ) ) ;
#20334 = CARTESIAN_POINT ( 'NONE',  ( 358.0000000000001137, -172.0000000000000000, -3.000000000000058176 ) ) ;
#20335 = ORIENTED_EDGE ( 'NONE', *, *, #26868, .F. ) ;
#20336 = CARTESIAN_POINT ( 'NONE',  ( 35.00000000000216716, 17.00000000000000000, 115.0000000000000142 ) ) ;
#20337 = EDGE_CURVE ( 'NONE', #19484, #33612, #44714, .T. ) ;
#20338 =( BOUNDED_CURVE ( )  B_SPLINE_CURVE ( 3, ( #26718, #49250, #18237, #34427 ),
 .UNSPECIFIED., .F., .F. ) 
 B_SPLINE_CURVE_WITH_KNOTS ( ( 4, 4 ),
 ( 4.712388980384689674, 6.283185307179586232 ),
 .UNSPECIFIED. ) 
 CURVE ( )  GEOMETRIC_REPRESENTATION_ITEM ( )  RATIONAL_B_SPLINE_CURVE ( ( 1.000000000000000000, 0.8047378541243649375, 0.8047378541243649375, 1.000000000000000000 ) ) 
 REPRESENTATION_ITEM ( '' )  );
#20339 = DIRECTION ( 'NONE',  ( -0.000000000000000000, -0.000000000000000000, -1.000000000000000000 ) ) ;
#20340 = ORIENTED_EDGE ( 'NONE', *, *, #5835, .F. ) ;
#20341 = AXIS2_PLACEMENT_3D ( 'NONE', #32801, #48393, #8938 ) ;
#20342 = VERTEX_POINT ( 'NONE', #7274 ) ;
#20343 = ORIENTED_EDGE ( 'NONE', *, *, #16863, .F. ) ;
#20344 = DIRECTION ( 'NONE',  ( 0.000000000000000000, -0.000000000000000000, -1.000000000000000000 ) ) ;
#20345 = PRESENTATION_STYLE_ASSIGNMENT (( #4705 ) ) ;
#20346 = LINE ( 'NONE', #43680, #38016 ) ;
#20347 = ORIENTED_EDGE ( 'NONE', *, *, #26070, .F. ) ;
#20348 = CARTESIAN_POINT ( 'NONE',  ( 341.9999999999999432, 169.0000000000001990, -344.0000000000002842 ) ) ;
#20349 = ORIENTED_EDGE ( 'NONE', *, *, #30936, .F. ) ;
#20350 = CARTESIAN_POINT ( 'NONE',  ( 349.9999999999999432, -168.9999999999999432, 341.9999999999997726 ) ) ;
#20351 = ORIENTED_EDGE ( 'NONE', *, *, #22554, .F. ) ;
#20352 = CARTESIAN_POINT ( 'NONE',  ( 3.231548175622897645, -9.463461120997347820, 9.282506307616472441 ) ) ;
#20353 = CARTESIAN_POINT ( 'NONE',  ( 1.647520908219943792, -0.4432416309287623979, 9.912102921405036682 ) ) ;
#20354 = CARTESIAN_POINT ( 'NONE',  ( 35.00000000000122213, 16.00000000000000000, 30.00000000000000000 ) ) ;
#20355 = DIRECTION ( 'NONE',  ( 0.000000000000000000, 0.000000000000000000, 1.000000000000000000 ) ) ;
#20356 = FACE_BOUND ( 'NONE', #25115, .T. ) ;
#20357 = CYLINDRICAL_SURFACE ( 'NONE', #18231, 2.000000000000001776 ) ;
#20358 = VERTEX_POINT ( 'NONE', #18802 ) ;
#20359 = CARTESIAN_POINT ( 'NONE',  ( 169.0000000000000000, -9.999999999999953815, -111.0000000000001563 ) ) ;
#20360 = B_SPLINE_SURFACE_WITH_KNOTS ( 'NONE', 3, 3, ( 
 ( #115, #42935, #7553, #45997 ),
 ( #15746, #39124, #38614, #31161 ),
 ( #18571, #14735, #11150, #35028 ),
 ( #31416, #50599, #30652, #34247 ) ),
 .UNSPECIFIED., .F., .F., .F.,
 ( 4, 4 ),
 ( 4, 4 ),
 ( 0.000000000000000000, 1.000000000000000000 ),
 ( 0.000000000000000000, 1.000000000000000000 ),
 .UNSPECIFIED. ) ;
#20361 = CARTESIAN_POINT ( 'NONE',  ( -46.69597344681494633, -1.750000000000010658, 80.81828755692798438 ) ) ;
#20362 = CARTESIAN_POINT ( 'NONE',  ( 181.0000000000000000, -184.9999999999999716, -360.0000000000002274 ) ) ;
#20363 = ADVANCED_FACE ( 'NONE', ( #49810 ), #7797, .T. ) ;
#20364 = DIRECTION ( 'NONE',  ( -0.000000000000000000, -0.000000000000000000, -1.000000000000000000 ) ) ;
#20365 = DIRECTION ( 'NONE',  ( 0.000000000000000000, 0.000000000000000000, -1.000000000000000000 ) ) ;
#20366 = ORIENTED_EDGE ( 'NONE', *, *, #33425, .F. ) ;
#20367 = FACE_OUTER_BOUND ( 'NONE', #11142, .T. ) ;
#20368 = B_SPLINE_CURVE_WITH_KNOTS ( 'NONE', 3,
 ( #34332, #25625, #30222, #37197 ),
 .UNSPECIFIED., .F., .F.,
 ( 4, 4 ),
 ( 0.003717746584991899611, 0.009855832532552960198 ),
 .UNSPECIFIED. ) ;
#20369 = CARTESIAN_POINT ( 'NONE',  ( 135.0000000000009663, 17.00000000000000000, -24.99999999999999289 ) ) ;
#20370 = VERTEX_POINT ( 'NONE', #30897 ) ;
#20371 = VECTOR ( 'NONE', #9381, 1000.000000000000000 ) ;
#20372 = DIRECTION ( 'NONE',  ( -1.000000000000000000, -0.000000000000000000, -0.000000000000000000 ) ) ;
#20373 = FACE_OUTER_BOUND ( 'NONE', #37560, .T. ) ;
#20374 = CARTESIAN_POINT ( 'NONE',  ( -168.4459734468149747, 1.025126265847089213, -160.9317124430720014 ) ) ;
#20375 = CARTESIAN_POINT ( 'NONE',  ( 349.9999999999999432, -166.9999999999999432, 355.9999999999997726 ) ) ;
#20376 = EDGE_LOOP ( 'NONE', ( #4922, #16972, #42634, #48101 ) ) ;
#20377 = CLOSED_SHELL ( 'NONE', ( #17944, #35882, #32436, #35967, #44810, #22464, #50412, #26867, #21523, #29678, #34710, #39208, #43489, #33847, #15347, #14532, #39011, #17527 ) ) ;
#20378 = ORIENTED_EDGE ( 'NONE', *, *, #26518, .T. ) ;
#20379 = CARTESIAN_POINT ( 'NONE',  ( 154.3291528190321458, 1.750000000000010214, 81.84341382277507648 ) ) ;
#20380 = CARTESIAN_POINT ( 'NONE',  ( -48.44597344681496054, 1.025126265847088991, -157.4317124430720582 ) ) ;
#20381 = EDGE_CURVE ( 'NONE', #13763, #10372, #42663, .T. ) ;
#20382 = ORIENTED_EDGE ( 'NONE', *, *, #45087, .F. ) ;
#20383 = ORIENTED_EDGE ( 'NONE', *, *, #22870, .T. ) ;
#20384 = CARTESIAN_POINT ( 'NONE',  ( -225.0000000000000568, 0.000000000000000000, 500.0000000000000000 ) ) ;
#20385 = LINE ( 'NONE', #8849, #18403 ) ;
#20386 = CARTESIAN_POINT ( 'NONE',  ( -64.99999999999846523, 16.00000000000000000, 60.00000000000000000 ) ) ;
#20387 = CARTESIAN_POINT ( 'NONE',  ( -206.6959734468149463, 0.000000000000000000, 165.0000000000000000 ) ) ;
#20388 = VERTEX_POINT ( 'NONE', #7026 ) ;
#20389 = ORIENTED_EDGE ( 'NONE', *, *, #25839, .F. ) ;
#20390 = EDGE_CURVE ( 'NONE', #7259, #38550, #45730, .T. ) ;
#20391 = EDGE_LOOP ( 'NONE', ( #7093, #37236, #25028, #36470 ) ) ;
#20392 = CARTESIAN_POINT ( 'NONE',  ( 194.9999999999999432, 0.000000000000000000, 0.000000000000000000 ) ) ;
#20393 = CARTESIAN_POINT ( 'NONE',  ( 1.011271242968683648, 0.7347315653655930312, 3.333333333333333481 ) ) ;
#20394 = ORIENTED_EDGE ( 'NONE', *, *, #7473, .F. ) ;
#20395 = VERTEX_POINT ( 'NONE', #50579 ) ;
#20396 = CYLINDRICAL_SURFACE ( 'NONE', #40198, 2.000000000000001776 ) ;
#20397 = FACE_OUTER_BOUND ( 'NONE', #48626, .T. ) ;
#20398 = CARTESIAN_POINT ( 'NONE',  ( 14.76429217231961566, 8.192625680377691566, 9.178419661560148768 ) ) ;
#20399 = ORIENTED_EDGE ( 'NONE', *, *, #26633, .F. ) ;
#20400 = VERTEX_POINT ( 'NONE', #22412 ) ;
#20401 = LINE ( 'NONE', #24781, #28251 ) ;
#20402 = CARTESIAN_POINT ( 'NONE',  ( 339.9999999999998863, -168.9999999999999432, 339.9999999999997726 ) ) ;
#20404 = ORIENTED_EDGE ( 'NONE', *, *, #15233, .F. ) ;
#20403 = VECTOR ( 'NONE', #40686, 1000.000000000000114 ) ;
#20405 = DIRECTION ( 'NONE',  ( -0.000000000000000000, -0.000000000000000000, -1.000000000000000000 ) ) ;
#20406 = CARTESIAN_POINT ( 'NONE',  ( -48.44597344681492501, 0.000000000000000000, 162.5682875569279702 ) ) ;
#20407 = CARTESIAN_POINT ( 'NONE',  ( -14.99999999999782041, 16.00000000000000000, 95.00000000000000000 ) ) ;
#20408 = VECTOR ( 'NONE', #23132, 1000.000000000000000 ) ;
#20409 =( BOUNDED_CURVE ( )  B_SPLINE_CURVE ( 3, ( #22560, #34139, #7174, #3825 ),
 .UNSPECIFIED., .F., .F. ) 
 B_SPLINE_CURVE_WITH_KNOTS ( ( 4, 4 ),
 ( 3.141592653589793116, 4.712388980384689674 ),
 .UNSPECIFIED. ) 
 CURVE ( )  GEOMETRIC_REPRESENTATION_ITEM ( )  RATIONAL_B_SPLINE_CURVE ( ( 1.000000000000000000, 0.8047378541243649375, 0.8047378541243649375, 1.000000000000000000 ) ) 
 REPRESENTATION_ITEM ( '' )  );
#20410 = CARTESIAN_POINT ( 'NONE',  ( 169.0000000000000000, -9.999999999999953815, -95.00000000000014211 ) ) ;
#20411 = VECTOR ( 'NONE', #9066, 1000.000000000000000 ) ;
#20412 = VERTEX_POINT ( 'NONE', #22920 ) ;
#20413 = VECTOR ( 'NONE', #18176, 1000.000000000000000 ) ;
#20414 = CARTESIAN_POINT ( 'NONE',  ( -31.94178169330213279, 9.256608784834037706, -3.760136334089591248 ) ) ;
#20415 = CARTESIAN_POINT ( 'NONE',  ( 355.9999999999999432, 174.9999999999996305, -360.0000000000003411 ) ) ;
#20416 = CARTESIAN_POINT ( 'NONE',  ( -21.58778298521296080, 25.34222074689773407, 3.199614146704519602 ) ) ;
#20417 = EDGE_CURVE ( 'NONE', #10351, #16113, #22667, .T. ) ;
#20418 = LINE ( 'NONE', #16330, #27965 ) ;
#20419 = VECTOR ( 'NONE', #3519, 1000.000000000000000 ) ;
#20420 = CYLINDRICAL_SURFACE ( 'NONE', #49077, 1.750000000000001554 ) ;
#20421 = DIRECTION ( 'NONE',  ( -0.000000000000000000, -1.000000000000000000, -0.000000000000000000 ) ) ;
#20422 = CARTESIAN_POINT ( 'NONE',  ( -166.6959734468149463, 0.000000000000000000, 165.0000000000000000 ) ) ;
#20423 = ORIENTED_EDGE ( 'NONE', *, *, #43987, .F. ) ;
#20424 = PRESENTATION_STYLE_ASSIGNMENT (( #15831 ) ) ;
#20425 = DIRECTION ( 'NONE',  ( 0.000000000000000000, 0.000000000000000000, -1.000000000000000000 ) ) ;
#20426 = ORIENTED_EDGE ( 'NONE', *, *, #26542, .F. ) ;
#20427 = FACE_OUTER_BOUND ( 'NONE', #25979, .T. ) ;
#20428 = CARTESIAN_POINT ( 'NONE',  ( -25.79500241909648395, -7.388441598285492518, 229.0000000000000000 ) ) ;
#20429 = CARTESIAN_POINT ( 'NONE',  ( 31.55402655318503236, 0.000000000000000000, -77.43171244307198720 ) ) ;
#20430 = ORIENTED_EDGE ( 'NONE', *, *, #50402, .F. ) ;
#20431 = LINE ( 'NONE', #43022, #24919 ) ;
#20432 = EDGE_LOOP ( 'NONE', ( #46910, #21450, #23095, #18022 ) ) ;
#20434 = ORIENTED_EDGE ( 'NONE', *, *, #13798, .T. ) ;
#20433 = VECTOR ( 'NONE', #28839, 1000.000000000000000 ) ;
#20435 = CARTESIAN_POINT ( 'NONE',  ( -5.000000000000000000, -184.7999999999999545, -340.2000000000001592 ) ) ;
#20436 = CARTESIAN_POINT ( 'NONE',  ( 183.0000000000000284, -9.999999999999953815, -99.00000000000014211 ) ) ;
#20437 = CIRCLE ( 'NONE', #27000, 2.000000000000001776 ) ;
#20438 = VECTOR ( 'NONE', #14683, 1000.000000000000000 ) ;
#20439 = ORIENTED_EDGE ( 'NONE', *, *, #42119, .T. ) ;
#20440 = CYLINDRICAL_SURFACE ( 'NONE', #13111, 1.749999999999987566 ) ;
#20441 = DIRECTION ( 'NONE',  ( 0.000000000000000000, -2.265761274745217480E-16, 1.000000000000000000 ) ) ;
#20442 = ORIENTED_EDGE ( 'NONE', *, *, #25315, .T. ) ;
#20443 = ADVANCED_FACE ( 'NONE', ( #37842 ), #34232, .T. ) ;
#20444 = VECTOR ( 'NONE', #28983, 1000.000000000000000 ) ;
#20445 = CARTESIAN_POINT ( 'NONE',  ( -50.00000000000000000, 50.00000000000000000, 900.0000000000000000 ) ) ;
#20446 = ORIENTED_EDGE ( 'NONE', *, *, #39456, .T. ) ;
#20447 = DIRECTION ( 'NONE',  ( -1.000000000000000000, 0.000000000000000000, 0.000000000000000000 ) ) ;
#20448 = CARTESIAN_POINT ( 'NONE',  ( -7.721099712662037540, -1.750000000000022871, -158.1565861772249093 ) ) ;
#20449 = CARTESIAN_POINT ( 'NONE',  ( -14.99999999999970868, 17.00000000000000000, -60.00000000000000000 ) ) ;
#20450 = AXIS2_PLACEMENT_3D ( 'NONE', #40953, #1460, #48347 ) ;
#20451 = ORIENTED_EDGE ( 'NONE', *, *, #11821, .T. ) ;
#20452 = CARTESIAN_POINT ( 'NONE',  ( -7.929028342769414373, 0.8360401409709390386, 1.626303258728256651E-16 ) ) ;
#20453 = DIRECTION ( 'NONE',  ( -1.000000000000000000, -0.000000000000000000, -0.000000000000000000 ) ) ;
#20454 = ORIENTED_EDGE ( 'NONE', *, *, #35416, .T. ) ;
#20455 = ORIENTED_EDGE ( 'NONE', *, *, #304, .T. ) ;
#20456 = ORIENTED_EDGE ( 'NONE', *, *, #47464, .F. ) ;
#20457 = CARTESIAN_POINT ( 'NONE',  ( -206.6959734468149463, -1.750000000000010658, 120.8182875569279702 ) ) ;
#20458 = B_SPLINE_CURVE_WITH_KNOTS ( 'NONE', 3,
 ( #11901, #38605, #50590, #34759 ),
 .UNSPECIFIED., .F., .F.,
 ( 4, 4 ),
 ( 0.0003760194760206631058, 0.0006307719036365294499 ),
 .UNSPECIFIED. ) ;
#20459 = EDGE_CURVE ( 'NONE', #49775, #12842, #45175, .T. ) ;
#20460 = CARTESIAN_POINT ( 'NONE',  ( 356.0000000000000568, 183.0000000000000853, 357.9999999999998295 ) ) ;
#20461 = ORIENTED_EDGE ( 'NONE', *, *, #32308, .F. ) ;
#20462 = EDGE_CURVE ( 'NONE', #38939, #30056, #1618, .T. ) ;
#20463 = LINE ( 'NONE', #44543, #46260 ) ;
#20464 = FACE_OUTER_BOUND ( 'NONE', #35981, .T. ) ;
#20465 = EDGE_CURVE ( 'NONE', #21273, #16032, #5161, .T. ) ;
#20466 = CARTESIAN_POINT ( 'NONE',  ( -5.647304616913629616, -154.8119894309598408, 472.8425600500173118 ) ) ;
#20467 =( BOUNDED_CURVE ( )  B_SPLINE_CURVE ( 3, ( #15925, #39790, #27723, #31841 ),
 .UNSPECIFIED., .F., .F. ) 
 B_SPLINE_CURVE_WITH_KNOTS ( ( 4, 4 ),
 ( 4.712388980384689674, 6.283185307179586232 ),
 .UNSPECIFIED. ) 
 CURVE ( )  GEOMETRIC_REPRESENTATION_ITEM ( )  RATIONAL_B_SPLINE_CURVE ( ( 1.000000000000000000, 0.8047378541243649375, 0.8047378541243649375, 1.000000000000000000 ) ) 
 REPRESENTATION_ITEM ( '' )  );
#20468 = DIRECTION ( 'NONE',  ( 3.364279341222521245E-16, 0.7071067811865474617, -0.7071067811865475727 ) ) ;
#20469 = CARTESIAN_POINT ( 'NONE',  ( 33.30402655318503946, 1.750000000000009992, -159.1817124430720298 ) ) ;
#20470 = CARTESIAN_POINT ( 'NONE',  ( 181.0000000000000000, -166.9999999999999432, -340.0000000000001137 ) ) ;
#20471 = LINE ( 'NONE', #7677, #12017 ) ;
#20472 = DIRECTION ( 'NONE',  ( 0.000000000000000000, 1.000000000000000000, 6.123233995736766036E-17 ) ) ;
#20473 =( BOUNDED_CURVE ( )  B_SPLINE_CURVE ( 3, ( #49643, #14533, #29945, #26086 ),
 .UNSPECIFIED., .F., .F. ) 
 B_SPLINE_CURVE_WITH_KNOTS ( ( 4, 4 ),
 ( 1.570796326794896558, 3.141592653589793116 ),
 .UNSPECIFIED. ) 
 CURVE ( )  GEOMETRIC_REPRESENTATION_ITEM ( )  RATIONAL_B_SPLINE_CURVE ( ( 1.000000000000000000, 0.8047378541243649375, 0.8047378541243649375, 1.000000000000000000 ) ) 
 REPRESENTATION_ITEM ( '' )  );
#20474 = DIRECTION ( 'NONE',  ( -1.000000000000000000, 0.000000000000000000, -0.000000000000000000 ) ) ;
#20475 = ADVANCED_FACE ( 'NONE', ( #14974 ), #20588, .T. ) ;
#20476 = PLANE ( 'NONE',  #37548 ) ;
#20477 = ADVANCED_FACE ( 'NONE', ( #605 ), #47501, .T. ) ;
#20478 = AXIS2_PLACEMENT_3D ( 'NONE', #18981, #6681, #34659 ) ;
#20479 = AXIS2_PLACEMENT_3D ( 'NONE', #2318, #2813, #37996 ) ;
#20480 = CYLINDRICAL_SURFACE ( 'NONE', #33100, 1.750000000000036193 ) ;
#20481 = EDGE_CURVE ( 'NONE', #3971, #47427, #16243, .T. ) ;
#20482 = UNCERTAINTY_MEASURE_WITH_UNIT (LENGTH_MEASURE( 1.000000000000000082E-05 ), #6522, 'distance_accuracy_value', 'NONE');
#20483 = ADVANCED_FACE ( 'NONE', ( #28294 ), #12632, .F. ) ;
#20484 = VECTOR ( 'NONE', #45762, 1000.000000000000000 ) ;
#20485 = CARTESIAN_POINT ( 'NONE',  ( 33.14391172085757375, 37.72293746533118508, -8.016098858316205167 ) ) ;
#20486 = ORIENTED_EDGE ( 'NONE', *, *, #4837, .T. ) ;
#20487 = LINE ( 'NONE', #17147, #758 ) ;
#20488 = AXIS2_PLACEMENT_3D ( 'NONE', #27420, #23827, #43052 ) ;
#20489 = LINE ( 'NONE', #43831, #14659 ) ;
#20490 = CARTESIAN_POINT ( 'NONE',  ( -114.9999999999978542, 17.00000000000000000, 115.0000000000000142 ) ) ;
#20491 = DIRECTION ( 'NONE',  ( 1.000000000000000000, 0.000000000000000000, -0.000000000000000000 ) ) ;
#20492 = VECTOR ( 'NONE', #6191, 1000.000000000000000 ) ;
#20493 = ORIENTED_EDGE ( 'NONE', *, *, #39821, .T. ) ;
#20494 = DIRECTION ( 'NONE',  ( 1.000000000000000000, 0.000000000000000000, 0.000000000000000000 ) ) ;
#20495 = FACE_OUTER_BOUND ( 'NONE', #24272, .T. ) ;
#20496 = ORIENTED_EDGE ( 'NONE', *, *, #28660, .F. ) ;
#20497 = CARTESIAN_POINT ( 'NONE',  ( -1.337801958641930300, -1.088266084286974689, 9.928159647716134018 ) ) ;
#20498 = FACE_OUTER_BOUND ( 'NONE', #20765, .T. ) ;
#20499 = CARTESIAN_POINT ( 'NONE',  ( 343.9999999999999432, 174.9999999999996589, -356.0000000000003411 ) ) ;
#20500 = VERTEX_POINT ( 'NONE', #39106 ) ;
#20501 = CARTESIAN_POINT ( 'NONE',  ( -208.4459734468149463, 0.000000000000000000, 159.0682875569279702 ) ) ;
#20502 = ADVANCED_FACE ( 'NONE', ( #4696 ), #43670, .T. ) ;
#20503 = ORIENTED_EDGE ( 'NONE', *, *, #48476, .T. ) ;
#20504 = ORIENTED_EDGE ( 'NONE', *, *, #39172, .T. ) ;
#20505 = EDGE_CURVE ( 'NONE', #25941, #24997, #39601, .T. ) ;
#20506 = B_SPLINE_CURVE_WITH_KNOTS ( 'NONE', 3,
 ( #14134, #10797, #11057, #17751 ),
 .UNSPECIFIED., .F., .F.,
 ( 4, 4 ),
 ( 0.0002936521407533901036, 0.0006663369986142128176 ),
 .UNSPECIFIED. ) ;
#20507 = EDGE_CURVE ( 'NONE', #25771, #40611, #46992, .T. ) ;
#20508 = ORIENTED_EDGE ( 'NONE', *, *, #27707, .T. ) ;
#20509 = LINE ( 'NONE', #36704, #31109 ) ;
#20510 = CARTESIAN_POINT ( 'NONE',  ( -5.670847180967843570, -1.750000000000022871, 161.8434138227750907 ) ) ;
#20511 = ORIENTED_EDGE ( 'NONE', *, *, #32433, .F. ) ;
#20512 = FACE_OUTER_BOUND ( 'NONE', #23617, .T. ) ;
#20513 = CARTESIAN_POINT ( 'NONE',  ( 342.8284271247462129, 167.0000000000000000, 341.9999999999998295 ) ) ;
#20514 = ADVANCED_FACE ( 'NONE', ( #12887 ), #31400, .F. ) ;
#20515 = CARTESIAN_POINT ( 'NONE',  ( 183.0000000000000000, -180.9999999999999432, -340.0000000000001137 ) ) ;
#20516 = CARTESIAN_POINT ( 'NONE',  ( -34.38425513258694366, 36.82177522737846687, 8.807470649214879543 ) ) ;
#20517 = ORIENTED_EDGE ( 'NONE', *, *, #39854, .T. ) ;
#20518 = ADVANCED_FACE ( 'NONE', ( #16497 ), #36014, .T. ) ;
#20519 = CARTESIAN_POINT ( 'NONE',  ( 6.204997580903516941, 7.611558401714507482, 230.0000000000000000 ) ) ;
#20520 = AXIS2_PLACEMENT_3D ( 'NONE', #5232, #20882, #8086 ) ;
#20521 = VECTOR ( 'NONE', #50490, 1000.000000000000000 ) ;
#20522 = ORIENTED_EDGE ( 'NONE', *, *, #7013, .F. ) ;
#20523 = FACE_OUTER_BOUND ( 'NONE', #26457, .T. ) ;
#20524 = LINE ( 'NONE', #4632, #26972 ) ;
#20525 = VERTEX_POINT ( 'NONE', #95 ) ;
#20526 = CARTESIAN_POINT ( 'NONE',  ( -1.080000014127418639, -0.7606467978654640749, 9.943883492372872723 ) ) ;
#20527 = CIRCLE ( 'NONE', #29429, 4.000000000000003553 ) ;
#20528 = VECTOR ( 'NONE', #44237, 1000.000000000000000 ) ;
#20529 = CARTESIAN_POINT ( 'NONE',  ( -115.0000000000000284, 17.00000000000000000, -114.9999999999999858 ) ) ;
#20530 = VECTOR ( 'NONE', #17719, 1000.000000000000000 ) ;
#20531 = ORIENTED_EDGE ( 'NONE', *, *, #18991, .T. ) ;
#20532 = FACE_OUTER_BOUND ( 'NONE', #15544, .T. ) ;
#20533 = DIRECTION ( 'NONE',  ( 1.000000000000000000, 0.000000000000000000, 0.000000000000000000 ) ) ;
#20534 = CARTESIAN_POINT ( 'NONE',  ( -46.69597344681494633, -1.750000000000010658, -79.18171244307201562 ) ) ;
#20535 = FACE_OUTER_BOUND ( 'NONE', #33654, .T. ) ;
#20536 = VERTEX_POINT ( 'NONE', #24455 ) ;
#20537 = EDGE_CURVE ( 'NONE', #11343, #16858, #4934, .T. ) ;
#20538 = CARTESIAN_POINT ( 'NONE',  ( 135.0000000000019043, 17.00000000000000000, 65.00000000000000000 ) ) ;
#20539 = DIRECTION ( 'NONE',  ( -0.000000000000000000, -0.000000000000000000, -1.000000000000000000 ) ) ;
#20540 = CARTESIAN_POINT ( 'NONE',  ( -34.38425513258695077, 36.82177522737848108, 8.807470649214879543 ) ) ;
#20541 = EDGE_LOOP ( 'NONE', ( #18050, #2265, #24663, #36244, #26820, #18122 ) ) ;
#20542 = EDGE_CURVE ( 'NONE', #24694, #11870, #43186, .T. ) ;
#20543 = EDGE_LOOP ( 'NONE', ( #28325, #36788, #26196, #23216, #2283 ) ) ;
#20544 = ITEM_DEFINED_TRANSFORMATION ( 'NONE', 'NONE', #41389,  #45486 ) ;
#20545 = CARTESIAN_POINT ( 'NONE',  ( -8.445973446814976526, 0.000000000000000000, -37.43171244307200141 ) ) ;
#20546 = CARTESIAN_POINT ( 'NONE',  ( -44.25629667545849344, 0.000000000000000000, 790.0000000000000000 ) ) ;
#20547 = EDGE_CURVE ( 'NONE', #4003, #44732, #39353, .T. ) ;
#20548 = EDGE_CURVE ( 'NONE', #49029, #5524, #12524, .T. ) ;
#20549 = CARTESIAN_POINT ( 'NONE',  ( 210.0000000000000568, 2.143131898507881856E-16, -120.9317124430720582 ) ) ;
#20550 = LINE ( 'NONE', #29762, #33050 ) ;
#20551 = CARTESIAN_POINT ( 'NONE',  ( -69.99999999999972999, 17.00000000000000000, -60.00000000000000000 ) ) ;
#20552 = ORIENTED_EDGE ( 'NONE', *, *, #12224, .F. ) ;
#20553 = EDGE_CURVE ( 'NONE', #38616, #17359, #32711, .T. ) ;
#20554 = LINE ( 'NONE', #30032, #46806 ) ;
#20555 = EDGE_CURVE ( 'NONE', #49286, #26731, #35506, .T. ) ;
#20556 = CARTESIAN_POINT ( 'NONE',  ( -205.6708471809678827, -1.750000000000009326, 161.8434138227750907 ) ) ;
#20557 = CARTESIAN_POINT ( 'NONE',  ( 135.0000000000012790, 17.00000000000000000, 30.00000000000000000 ) ) ;
#20558 = CARTESIAN_POINT ( 'NONE',  ( 0.5109188679997901383, 1.175605252300628623, 9.967237415621765351 ) ) ;
#20559 = VERTEX_POINT ( 'NONE', #8298 ) ;
#20560 = AXIS2_PLACEMENT_3D ( 'NONE', #12612, #46719, #31888 ) ;
#20561 = CARTESIAN_POINT ( 'NONE',  ( -0.4266413953668892756, -1.250184266969579294, 9.943883492372849631 ) ) ;
#20562 = ORIENTED_EDGE ( 'NONE', *, *, #39401, .F. ) ;
#20563 = EDGE_LOOP ( 'NONE', ( #21104, #4411, #37786, #41091, #37711, #34994 ) ) ;
#20564 = CYLINDRICAL_SURFACE ( 'NONE', #6599, 1.750000000000001554 ) ;
#20565 = CARTESIAN_POINT ( 'NONE',  ( -208.4459734468148611, -1.025126265847089213, 159.0682875569279418 ) ) ;
#20566 = AXIS2_PLACEMENT_3D ( 'NONE', #50672, #35099, #27129 ) ;
#20567 = CARTESIAN_POINT ( 'NONE',  ( -85.67084718096784002, 1.750000000000010214, -80.20683870891910772 ) ) ;
#20568 = DIRECTION ( 'NONE',  ( 0.000000000000000000, 0.000000000000000000, 1.000000000000000000 ) ) ;
#20569 = ORIENTED_EDGE ( 'NONE', *, *, #14902, .T. ) ;
#20570 = CARTESIAN_POINT ( 'NONE',  ( 0.000000000000000000, 13.48684210526315930, -4.250000000000000000 ) ) ;
#20571 = ADVANCED_FACE ( 'NONE', ( #32653 ), #29052, .T. ) ;
#20572 = EDGE_LOOP ( 'NONE', ( #35961, #15823 ) ) ;
#20573 = CARTESIAN_POINT ( 'NONE',  ( -164.9459734468149463, 1.025126265847089435, 39.06828755692797728 ) ) ;
#20574 = CARTESIAN_POINT ( 'NONE',  ( -166.6959734468149463, 0.000000000000000000, 165.0000000000000000 ) ) ;
#20575 = CARTESIAN_POINT ( 'NONE',  ( 33.86622497129647513, -3.037805405904928868, 7.906207997025717304 ) ) ;
#20576 = CYLINDRICAL_SURFACE ( 'NONE', #50405, 1.750000000000015543 ) ;
#20577 = ORIENTED_EDGE ( 'NONE', *, *, #17350, .F. ) ;
#20578 = VERTEX_POINT ( 'NONE', #13881 ) ;
#20579 = FACE_OUTER_BOUND ( 'NONE', #41599, .T. ) ;
#20580 = VERTEX_POINT ( 'NONE', #48501 ) ;
#20581 = CARTESIAN_POINT ( 'NONE',  ( -4.945973446814903696, 2.143131898507912917E-16, 165.0000000000000000 ) ) ;
#20582 = CARTESIAN_POINT ( 'NONE',  ( -164.9459734468149463, -1.025126265847089435, 39.06828755692797728 ) ) ;
#20583 = DIRECTION ( 'NONE',  ( 0.1191452206184309970, 0.000000000000000000, -0.9928768384869220975 ) ) ;
#20584 = VERTEX_POINT ( 'NONE', #33662 ) ;
#20585 = CARTESIAN_POINT ( 'NONE',  ( 166.9999999999999716, -5.999999999999950262, -340.0000000000001137 ) ) ;
#20586 = ADVANCED_FACE ( 'NONE', ( #33422, #48995 ), #44667, .F. ) ;
#20587 = DIRECTION ( 'NONE',  ( 1.000000000000000000, -0.000000000000000000, -0.000000000000000000 ) ) ;
#20588 = CYLINDRICAL_SURFACE ( 'NONE', #24288, 1.750000000000015543 ) ;
#20589 = VECTOR ( 'NONE', #42670, 1000.000000000000000 ) ;
#20590 = DIRECTION ( 'NONE',  ( 0.000000000000000000, 0.000000000000000000, 1.000000000000000000 ) ) ;
#20591 = CARTESIAN_POINT ( 'NONE',  ( -204.9459734468149463, 2.143131898507880377E-16, 119.0682875569279702 ) ) ;
#20592 = ORIENTED_EDGE ( 'NONE', *, *, #50621, .F. ) ;
#20593 = ORIENTED_EDGE ( 'NONE', *, *, #49638, .T. ) ;
#20594 = ADVANCED_FACE ( 'NONE', ( #41353 ), #44423, .T. ) ;
#20595 = ORIENTED_EDGE ( 'NONE', *, *, #42830, .F. ) ;
#20596 = CARTESIAN_POINT ( 'NONE',  ( -19.99999999999784706, 17.00000000000000000, 115.0000000000000142 ) ) ;
#20597 = AXIS2_PLACEMENT_3D ( 'NONE', #5583, #14033, #45574 ) ;
#20598 = PLANE ( 'NONE',  #50208 ) ;
#20599 = ORIENTED_EDGE ( 'NONE', *, *, #18745, .T. ) ;
#20600 = CARTESIAN_POINT ( 'NONE',  ( 350.0000000000000000, 181.0000000000000284, -344.0000000000001705 ) ) ;
#20601 = AXIS2_PLACEMENT_3D ( 'NONE', #41390, #19542, #39323 ) ;
#20602 = VERTEX_POINT ( 'NONE', #21091 ) ;
#20603 = DIRECTION ( 'NONE',  ( 1.000000000000000000, 0.000000000000000000, 0.000000000000000000 ) ) ;
#20604 = ORIENTED_EDGE ( 'NONE', *, *, #4805, .F. ) ;
#20605 =( NAMED_UNIT ( * ) PLANE_ANGLE_UNIT ( ) SI_UNIT ( $, .RADIAN. ) );
#20606 = CARTESIAN_POINT ( 'NONE',  ( 3.345242017215822372, -2.159124855890657724, -4.878909776184769953E-16 ) ) ;
#20607 = CARTESIAN_POINT ( 'NONE',  ( 350.0000000000000000, 181.0000000000000284, -360.0000000000002274 ) ) ;
#20608 = CARTESIAN_POINT ( 'NONE',  ( 151.5540265531850537, 0.000000000000000000, 39.06828755692798438 ) ) ;
#20609 = EDGE_CURVE ( 'NONE', #5026, #14784, #48250, .T. ) ;
#20610 = EDGE_CURVE ( 'NONE', #10906, #12365, #29549, .T. ) ;
#20611 = CARTESIAN_POINT ( 'NONE',  ( 224.9999999999999716, -164.9999999999999716, 32.29650858650035161 ) ) ;
#20612 = CARTESIAN_POINT ( 'NONE',  ( 151.5540265531850537, 0.000000000000000000, -77.43171244307204404 ) ) ;
#20613 = CARTESIAN_POINT ( 'NONE',  ( -2.538055338523177440, -50.00000000000000711, -9.367992836599954742 ) ) ;
#20614 = ORIENTED_EDGE ( 'NONE', *, *, #14042, .T. ) ;
#20615 = CARTESIAN_POINT ( 'NONE',  ( -204.9459734468148895, -1.025126265847089213, 159.0682875569279418 ) ) ;
#20616 = ADVANCED_FACE ( 'NONE', ( #5692 ), #1133, .T. ) ;
#20617 = DIRECTION ( 'NONE',  ( 0.000000000000000000, 0.000000000000000000, 1.000000000000000000 ) ) ;
#20618 = CARTESIAN_POINT ( 'NONE',  ( 166.9999999999999716, -164.9999999999999432, 355.9999999999998863 ) ) ;
#20619 = ADVANCED_FACE ( 'NONE', ( #13141 ), #2348, .F. ) ;
#20620 = EDGE_CURVE ( 'NONE', #40787, #14561, #50416, .T. ) ;
#20621 =( BOUNDED_CURVE ( )  B_SPLINE_CURVE ( 3, ( #47183, #31843, #4126, #19768 ),
 .UNSPECIFIED., .F., .F. ) 
 B_SPLINE_CURVE_WITH_KNOTS ( ( 4, 4 ),
 ( 4.712388980384689674, 6.283185307179586232 ),
 .UNSPECIFIED. ) 
 CURVE ( )  GEOMETRIC_REPRESENTATION_ITEM ( )  RATIONAL_B_SPLINE_CURVE ( ( 1.000000000000000000, 0.8047378541243649375, 0.8047378541243649375, 1.000000000000000000 ) ) 
 REPRESENTATION_ITEM ( '' )  );
#20622 = CARTESIAN_POINT ( 'NONE',  ( 33.43156050989131955, -4.370686678976570150, 8.807470649214879543 ) ) ;
#20623 = ORIENTED_EDGE ( 'NONE', *, *, #30204, .T. ) ;
#20624 = CARTESIAN_POINT ( 'NONE',  ( 360.0000000000000000, 169.0000000000001990, -344.0000000000002842 ) ) ;
#20625 = ORIENTED_EDGE ( 'NONE', *, *, #46351, .T. ) ;
#20626 = DIRECTION ( 'NONE',  ( 3.364279341222521245E-16, 0.7071067811865474617, -0.7071067811865476838 ) ) ;
#20627 =( BOUNDED_CURVE ( )  B_SPLINE_CURVE ( 3, ( #37244, #2066, #3311, #26168 ),
 .UNSPECIFIED., .F., .F. ) 
 B_SPLINE_CURVE_WITH_KNOTS ( ( 4, 4 ),
 ( 3.141592653589793116, 4.712388980384689674 ),
 .UNSPECIFIED. ) 
 CURVE ( )  GEOMETRIC_REPRESENTATION_ITEM ( )  RATIONAL_B_SPLINE_CURVE ( ( 1.000000000000000000, 0.8047378541243649375, 0.8047378541243649375, 1.000000000000000000 ) ) 
 REPRESENTATION_ITEM ( '' )  );
#20628 = AXIS2_PLACEMENT_3D ( 'NONE', #28040, #28547, #43672 ) ;
#20629 = CIRCLE ( 'NONE', #49249, 4.000000000000003553 ) ;
#20630 = ADVANCED_FACE ( 'NONE', ( #48754 ), #40605, .F. ) ;
#20631 = CARTESIAN_POINT ( 'NONE',  ( 0.000000000000000000, -168.9999999999999432, -360.0000000000002274 ) ) ;
#20632 = VERTEX_POINT ( 'NONE', #17990 ) ;
#20633 = VECTOR ( 'NONE', #20049, 1000.000000000000000 ) ;
#20634 = PLANE ( 'NONE',  #31236 ) ;
#20635 = CARTESIAN_POINT ( 'NONE',  ( 358.3431457505075741, -165.0000000000001137, -340.0000000000002274 ) ) ;
#20636 = CARTESIAN_POINT ( 'NONE',  ( 7.787882027935128626, 1.707024178319727969, -2.642742795433417058E-16 ) ) ;
#20637 =( BOUNDED_CURVE ( )  B_SPLINE_CURVE ( 3, ( #50384, #35321, #7086, #39158 ),
 .UNSPECIFIED., .F., .F. ) 
 B_SPLINE_CURVE_WITH_KNOTS ( ( 4, 4 ),
 ( 1.570796326794896558, 3.141592653589793116 ),
 .UNSPECIFIED. ) 
 CURVE ( )  GEOMETRIC_REPRESENTATION_ITEM ( )  RATIONAL_B_SPLINE_CURVE ( ( 1.000000000000000000, 0.8047378541243649375, 0.8047378541243649375, 1.000000000000000000 ) ) 
 REPRESENTATION_ITEM ( '' )  );
#20638 = ORIENTED_EDGE ( 'NONE', *, *, #6276, .T. ) ;
#20639 = ORIENTED_EDGE ( 'NONE', *, *, #42742, .F. ) ;
#20640 = CARTESIAN_POINT ( 'NONE',  ( -0.4402948852767746279, 2.015117899693936732, 9.894754715216722118 ) ) ;
#20641 = DIRECTION ( 'NONE',  ( -0.000000000000000000, -0.000000000000000000, -1.000000000000000000 ) ) ;
#20642 = VERTEX_POINT ( 'NONE', #13646 ) ;
#20643 = ORIENTED_EDGE ( 'NONE', *, *, #21107, .F. ) ;
#20644 = FACE_OUTER_BOUND ( 'NONE', #34403, .T. ) ;
#20645 = DIRECTION ( 'NONE',  ( -1.000000000000000000, -0.000000000000000000, -0.000000000000000000 ) ) ;
#20646 = CARTESIAN_POINT ( 'NONE',  ( 45.64490844644691236, 21.32281559348795952, 8.807470649214879543 ) ) ;
#20647 = CARTESIAN_POINT ( 'NONE',  ( 181.0000000000000000, -272.5000000000000000, -110.9999999999999005 ) ) ;
#20648 = VERTEX_POINT ( 'NONE', #1608 ) ;
#20649 = ORIENTED_EDGE ( 'NONE', *, *, #36630, .F. ) ;
#20650 = VERTEX_POINT ( 'NONE', #44911 ) ;
#20651 = EDGE_CURVE ( 'NONE', #41040, #30921, #3338, .T. ) ;
#20652 = CARTESIAN_POINT ( 'NONE',  ( -4.945973446814903696, 2.143131898507912917E-16, 42.56828755692802702 ) ) ;
#20653 = FACE_OUTER_BOUND ( 'NONE', #35371, .T. ) ;
#20654 = VERTEX_POINT ( 'NONE', #1856 ) ;
#20655 = ORIENTED_EDGE ( 'NONE', *, *, #49136, .F. ) ;
#20656 = CARTESIAN_POINT ( 'NONE',  ( -6.695973446814940111, -1.750000000000024203, -79.18171244307201562 ) ) ;
#20657 = VECTOR ( 'NONE', #21538, 1000.000000000000000 ) ;
#20658 = CARTESIAN_POINT ( 'NONE',  ( 45.64490844644691236, 21.32281559348795952, 8.807470649214879543 ) ) ;
#20659 = VERTEX_POINT ( 'NONE', #22609 ) ;
#20660 = VERTEX_POINT ( 'NONE', #3609 ) ;
#20661 = VECTOR ( 'NONE', #20364, 1000.000000000000000 ) ;
#20662 = CARTESIAN_POINT ( 'NONE',  ( -4.999999999999967137, -6.505213034912994064E-16, 0.000000000000000000 ) ) ;
#20663 = LINE ( 'NONE', #49577, #9227 ) ;
#20664 = ORIENTED_EDGE ( 'NONE', *, *, #5993, .F. ) ;
#20665 = CARTESIAN_POINT ( 'NONE',  ( -177.4999999999999716, -72.50000000000001421, -9.999999999999973355 ) ) ;
#20666 = CARTESIAN_POINT ( 'NONE',  ( -114.9999999999997158, 16.00000000000000000, -84.99999999999998579 ) ) ;
#20667 = CARTESIAN_POINT ( 'NONE',  ( 350.0000000000000000, -164.9999999999999432, -356.0000000000002274 ) ) ;
#20668 = EDGE_CURVE ( 'NONE', #41009, #13781, #26458, .T. ) ;
#20669 = EDGE_CURVE ( 'NONE', #30589, #17110, #26213, .T. ) ;
#20670 = CIRCLE ( 'NONE', #36256, 2.000000000000001776 ) ;
#20671 = CARTESIAN_POINT ( 'NONE',  ( -208.4459734468149463, 0.000000000000000000, -40.93171244307202983 ) ) ;
#20672 = B_SPLINE_CURVE_WITH_KNOTS ( 'NONE', 3,
 ( #28639, #24803, #37126, #17598 ),
 .UNSPECIFIED., .F., .F.,
 ( 4, 4 ),
 ( 0.9811748202683100439, 0.9878904167554126703 ),
 .UNSPECIFIED. ) ;
#20673 = VERTEX_POINT ( 'NONE', #42095 ) ;
#20674 = FACE_OUTER_BOUND ( 'NONE', #47258, .T. ) ;
#20675 = CARTESIAN_POINT ( 'NONE',  ( -6.695973446814940111, 0.000000000000000000, 165.0000000000000000 ) ) ;
#20676 = B_SPLINE_SURFACE_WITH_KNOTS ( 'NONE', 3, 3, ( 
 ( #30033, #44877, #10760, #48952 ),
 ( #49216, #49472, #18200, #26414 ),
 ( #2806, #17946, #41565, #22061 ),
 ( #33629, #25673, #45638, #33881 ) ),
 .UNSPECIFIED., .F., .F., .F.,
 ( 4, 4 ),
 ( 4, 4 ),
 ( 0.000000000000000000, 1.000000000000000000 ),
 ( 0.000000000000000000, 1.000000000000000000 ),
 .UNSPECIFIED. ) ;
#20677 = CARTESIAN_POINT ( 'NONE',  ( 210.0000000000000568, 2.143131898507881856E-16, -120.9317124430720582 ) ) ;
#20678 = EDGE_CURVE ( 'NONE', #7390, #14002, #27839, .T. ) ;
#20679 = CARTESIAN_POINT ( 'NONE',  ( -28.96803024440907137, -18.11533787072017176, 7.455576670931136185 ) ) ;
#20680 = ADVANCED_FACE ( 'NONE', ( #3099 ), #11060, .F. ) ;
#20681 = EDGE_CURVE ( 'NONE', #44030, #25517, #5802, .T. ) ;
#20682 = CARTESIAN_POINT ( 'NONE',  ( -0.9000089392641369423, -1.054368634403656690, 9.960033073700792272 ) ) ;
#20683 = AXIS2_PLACEMENT_3D ( 'NONE', #6626, #37953, #7853 ) ;
#20684 = CARTESIAN_POINT ( 'NONE',  ( -1.962539651752354564, 0.2571568065648870971, 9.897807938190499755 ) ) ;
#20685 = CARTESIAN_POINT ( 'NONE',  ( 15.42815683172628738, 34.17926237904582365, 7.697694107796191787 ) ) ;
#20686 = ORIENTED_EDGE ( 'NONE', *, *, #7113, .F. ) ;
#20687 = CARTESIAN_POINT ( 'NONE',  ( 71.55402655318505367, -1.025126265847089213, -160.9317124430720014 ) ) ;
#20688 = CARTESIAN_POINT ( 'NONE',  ( 0.000000000000000000, 17.00000000000000000, 0.000000000000000000 ) ) ;
#20689 = VECTOR ( 'NONE', #48575, 1000.000000000000000 ) ;
#20690 = EDGE_LOOP ( 'NONE', ( #17466, #34250, #15582, #49927 ) ) ;
#20691 = CARTESIAN_POINT ( 'NONE',  ( 10.01251772323701772, 8.486842105263161073, 18.46084505325461578 ) ) ;
#20692 = CARTESIAN_POINT ( 'NONE',  ( 5.930385588435886923, -41.38048276556310157, 8.846626183609801686 ) ) ;
#20693 = DIRECTION ( 'NONE',  ( 0.000000000000000000, 0.000000000000000000, 1.000000000000000000 ) ) ;
#20694 = ORIENTED_EDGE ( 'NONE', *, *, #33211, .F. ) ;
#20695 = CARTESIAN_POINT ( 'NONE',  ( 183.0000000000000000, -180.9999999999999716, -340.0000000000001137 ) ) ;
#20696 = ORIENTED_EDGE ( 'NONE', *, *, #22860, .T. ) ;
#20697 = ORIENTED_EDGE ( 'NONE', *, *, #3986, .F. ) ;
#20698 = CARTESIAN_POINT ( 'NONE',  ( -33.43156050989129824, 4.370686678976795747, 8.807470649214879543 ) ) ;
#20699 = AXIS2_PLACEMENT_3D ( 'NONE', #14881, #50486, #38749 ) ;
#20700 = FACE_OUTER_BOUND ( 'NONE', #15947, .T. ) ;
#20701 = VERTEX_POINT ( 'NONE', #18999 ) ;
#20702 = VECTOR ( 'NONE', #9072, 1000.000000000000000 ) ;
#20703 = LINE ( 'NONE', #43791, #9022 ) ;
#20704 = DIRECTION ( 'NONE',  ( 0.000000000000000000, 0.000000000000000000, 1.000000000000000000 ) ) ;
#20705 = ORIENTED_EDGE ( 'NONE', *, *, #7627, .T. ) ;
#20706 = ORIENTED_EDGE ( 'NONE', *, *, #22593, .F. ) ;
#20707 = DIRECTION ( 'NONE',  ( 6.203854594147707562E-25, -2.067951531382569187E-25, 1.000000000000000000 ) ) ;
#20708 = ORIENTED_EDGE ( 'NONE', *, *, #1694, .T. ) ;
#20709 = ADVANCED_FACE ( 'NONE', ( #6448, #34946, #18740, #22104, #2840, #42357 ), #15422, .T. ) ;
#20710 = CARTESIAN_POINT ( 'NONE',  ( -1.249999999999999778, 0.000000000000000000, -10.00000000000000000 ) ) ;
#20711 = CARTESIAN_POINT ( 'NONE',  ( -19.52505477809972945, -36.96330698207071919, 8.846626183609801686 ) ) ;
#20712 = CARTESIAN_POINT ( 'NONE',  ( -1.170692300221099824, -0.8653481604899971869, 9.938560165450807560 ) ) ;
#20713 = ORIENTED_EDGE ( 'NONE', *, *, #39119, .F. ) ;
#20714 = LINE ( 'NONE', #36391, #20238 ) ;
#20715 = CARTESIAN_POINT ( 'NONE',  ( -0.3370904143228978245, 0.2449105217885259589, 10.00000000000000000 ) ) ;
#20716 = VERTEX_POINT ( 'NONE', #45419 ) ;
#20717 = ORIENTED_EDGE ( 'NONE', *, *, #17539, .T. ) ;
#20718 = ORIENTED_EDGE ( 'NONE', *, *, #19923, .F. ) ;
#20719 = CARTESIAN_POINT ( 'NONE',  ( -1.468713901642213493, -0.3220470327672489419, 9.927319414211227766 ) ) ;
#20720 = AXIS2_PLACEMENT_3D ( 'NONE', #849, #16992, #46985 ) ;
#20721 = CARTESIAN_POINT ( 'NONE',  ( -1.962712821592842882, -1.022159834731130257, 9.881002359080275355 ) ) ;
#20722 = ORIENTED_EDGE ( 'NONE', *, *, #10976, .F. ) ;
#20723 = CARTESIAN_POINT ( 'NONE',  ( 35.05402655318504657, 2.143131898507880377E-16, -77.43171244307198720 ) ) ;
#20724 = CARTESIAN_POINT ( 'NONE',  ( -4.945973446814903696, 2.143131898507912917E-16, -117.4317124430720156 ) ) ;
#20725 = CARTESIAN_POINT ( 'NONE',  ( 73.30402655318508209, -1.750000000000010658, 120.8182875569279702 ) ) ;
#20726 = LINE ( 'NONE', #16890, #5508 ) ;
#20727 = CARTESIAN_POINT ( 'NONE',  ( -0.6126904405382037622, -1.085824959725731231, 9.981352469109934233 ) ) ;
#20728 = APPLICATION_CONTEXT ( 'automotive_design' ) ;
#20729 = CARTESIAN_POINT ( 'NONE',  ( 7.499999999999996447, 194.9999999999999716, -240.0000000000000000 ) ) ;
#20730 = CARTESIAN_POINT ( 'NONE',  ( 181.0000000000000284, 2.775557561562891351E-14, -111.0000000000001563 ) ) ;
#20731 = FACE_OUTER_BOUND ( 'NONE', #2580, .T. ) ;
#20732 = DIRECTION ( 'NONE',  ( 0.000000000000000000, 0.000000000000000000, 1.000000000000000000 ) ) ;
#20733 = CARTESIAN_POINT ( 'NONE',  ( 129.9999999999999432, 17.00000000000000000, -114.9999999999999858 ) ) ;
#20734 = VECTOR ( 'NONE', #24048, 1000.000000000000000 ) ;
#20735 = DIRECTION ( 'NONE',  ( 0.6904757466825006684, 0.7233555441435720601, -0.000000000000000000 ) ) ;
#20736 = AXIS2_PLACEMENT_3D ( 'NONE', #28509, #15687, #1057 ) ;
#20737 = CARTESIAN_POINT ( 'NONE',  ( 164.9999999999999716, 17.00000000000000000, -55.00000000000000711 ) ) ;
#20738 = ORIENTED_EDGE ( 'NONE', *, *, #35913, .F. ) ;
#20739 = ADVANCED_FACE ( 'NONE', ( #30570 ), #2590, .T. ) ;
#20740 = CARTESIAN_POINT ( 'NONE',  ( 344.0000000000000000, 185.0000000000000000, 359.9999999999998295 ) ) ;
#20741 = PLANE ( 'NONE',  #4043 ) ;
#20742 = DIRECTION ( 'NONE',  ( 1.000000000000000000, 1.156482317317870492E-16, 0.000000000000000000 ) ) ;
#20743 = LINE ( 'NONE', #36684, #14808 ) ;
#20744 = ORIENTED_EDGE ( 'NONE', *, *, #31058, .F. ) ;
#20745 = CARTESIAN_POINT ( 'NONE',  ( 5.204748896376250699E-16, 13.98684210526316107, 4.250000000000000000 ) ) ;
#20746 = CARTESIAN_POINT ( 'NONE',  ( 181.0000000000000000, -164.9999999999999432, -358.0000000000001705 ) ) ;
#20747 = EDGE_LOOP ( 'NONE', ( #21966, #30444, #8573, #32350, #41610, #268 ) ) ;
#20748 = CARTESIAN_POINT ( 'NONE',  ( 1.011271242968688311, -0.7347315653655855927, -10.00000000000000000 ) ) ;
#20749 = FACE_OUTER_BOUND ( 'NONE', #18814, .T. ) ;
#20750 = DIRECTION ( 'NONE',  ( 1.000000000000000000, 0.000000000000000000, 0.000000000000000000 ) ) ;
#20751 = ORIENTED_EDGE ( 'NONE', *, *, #42917, .T. ) ;
#20752 =( NAMED_UNIT ( * ) SI_UNIT ( $, .STERADIAN. ) SOLID_ANGLE_UNIT ( ) );
#20753 = VERTEX_POINT ( 'NONE', #18500 ) ;
#20754 = ORIENTED_EDGE ( 'NONE', *, *, #28681, .F. ) ;
#20755 = ORIENTED_EDGE ( 'NONE', *, *, #8346, .T. ) ;
#20756 = CARTESIAN_POINT ( 'NONE',  ( 343.9999999999999432, 185.0000000000002558, -360.0000000000003411 ) ) ;
#20757 = CARTESIAN_POINT ( 'NONE',  ( -7.749480817862350435, -14.85497772329513211, 9.403735324607438884 ) ) ;
#20758 = CIRCLE ( 'NONE', #26592, 0.5000000000000004441 ) ;
#20759 = ORIENTED_EDGE ( 'NONE', *, *, #24297, .F. ) ;
#20760 = CARTESIAN_POINT ( 'NONE',  ( -204.9459734468149463, 2.143131898507880377E-16, -77.43171244307204404 ) ) ;
#20761 = CARTESIAN_POINT ( 'NONE',  ( 35.00000000000152767, 17.00000000000000000, 35.00000000000000000 ) ) ;
#20762 = CIRCLE ( 'NONE', #13361, 4.000000000000003553 ) ;
#20763 = DIRECTION ( 'NONE',  ( 1.612977847700450206E-50, 0.000000000000000000, 1.000000000000000000 ) ) ;
#20764 = FACE_BOUND ( 'NONE', #22978, .T. ) ;
#20765 = EDGE_LOOP ( 'NONE', ( #45713, #12016, #9478, #15163 ) ) ;
#20766 = CARTESIAN_POINT ( 'NONE',  ( -5.000000000000000000, -165.1999999999999602, 359.7999999999997840 ) ) ;
#20767 = ORIENTED_EDGE ( 'NONE', *, *, #45029, .F. ) ;
#20768 = AXIS2_PLACEMENT_3D ( 'NONE', #37559, #2378, #30095 ) ;
#20769 = CARTESIAN_POINT ( 'NONE',  ( 112.2789002873379758, 1.749999999999996669, -160.2068387089191219 ) ) ;
#20770 = LINE ( 'NONE', #16942, #8131 ) ;
#20771 = VERTEX_POINT ( 'NONE', #10311 ) ;
#20772 = EDGE_LOOP ( 'NONE', ( #4821, #31533, #22403, #14271 ) ) ;
#20773 = LINE ( 'NONE', #32598, #29503 ) ;
#20774 =( BOUNDED_CURVE ( )  B_SPLINE_CURVE ( 3, ( #43568, #28187, #36669, #8435 ),
 .UNSPECIFIED., .F., .F. ) 
 B_SPLINE_CURVE_WITH_KNOTS ( ( 4, 4 ),
 ( 1.570796326794882791, 3.141592653589793116 ),
 .UNSPECIFIED. ) 
 CURVE ( )  GEOMETRIC_REPRESENTATION_ITEM ( )  RATIONAL_B_SPLINE_CURVE ( ( 1.000000000000000000, 0.8047378541243617178, 0.8047378541243617178, 1.000000000000000000 ) ) 
 REPRESENTATION_ITEM ( '' )  );
#20775 = LINE ( 'NONE', #9232, #19290 ) ;
#20776 = B_SPLINE_SURFACE_WITH_KNOTS ( 'NONE', 3, 3, ( 
 ( #50641, #15546, #11691, #31457 ),
 ( #42980, #43241, #8106, #39162 ),
 ( #3992, #39419, #37287, #25969 ),
 ( #29051, #21342, #33661, #36773 ) ),
 .UNSPECIFIED., .F., .F., .F.,
 ( 4, 4 ),
 ( 4, 4 ),
 ( 0.000000000000000000, 1.000000000000000000 ),
 ( 0.000000000000000000, 1.000000000000000000 ),
 .UNSPECIFIED. ) ;
#20777 = ORIENTED_EDGE ( 'NONE', *, *, #34938, .T. ) ;
#20778 = FACE_OUTER_BOUND ( 'NONE', #7795, .T. ) ;
#20779 = CARTESIAN_POINT ( 'NONE',  ( -25.04522487443065160, 22.77512090857326754, 8.356839323120299312 ) ) ;
#20780 = CARTESIAN_POINT ( 'NONE',  ( 181.0000000000000000, -256.4999999999999432, -339.9999999999998863 ) ) ;
#20781 = CARTESIAN_POINT ( 'NONE',  ( -1.011271242968693862, 0.7347315653655780432, 10.00000000000000000 ) ) ;
#20782 = VERTEX_POINT ( 'NONE', #34429 ) ;
#20783 = DIRECTION ( 'NONE',  ( -1.000000000000000000, 0.000000000000000000, 0.000000000000000000 ) ) ;
#20784 = CARTESIAN_POINT ( 'NONE',  ( -164.9999999999984936, 17.00000000000000000, 35.00000000000000000 ) ) ;
#20785 = CARTESIAN_POINT ( 'NONE',  ( 152.2789002873379900, 1.750000000000009548, 161.8434138227750907 ) ) ;
#20786 = ORIENTED_EDGE ( 'NONE', *, *, #1844, .T. ) ;
#20787 = VERTEX_POINT ( 'NONE', #37778 ) ;
#20788 = CONTEXT_DEPENDENT_SHAPE_REPRESENTATION ( #9933, #3636 ) ;
#20789 = CARTESIAN_POINT ( 'NONE',  ( 35.05402655318504657, -1.025126265847089213, -160.9317124430720014 ) ) ;
#20790 = DIRECTION ( 'NONE',  ( 0.000000000000000000, 0.000000000000000000, 1.000000000000000000 ) ) ;
#20791 = ADVANCED_FACE ( 'NONE', ( #50007 ), #22349, .T. ) ;
#20792 = VECTOR ( 'NONE', #15912, 1000.000000000000000 ) ;
#20793 = CARTESIAN_POINT ( 'NONE',  ( 33.30402655318503946, 1.750000000000010214, -39.18171244307202983 ) ) ;
#20794 = LINE ( 'NONE', #36475, #47765 ) ;
#20795 = ORIENTED_EDGE ( 'NONE', *, *, #2101, .T. ) ;
#20796 = CARTESIAN_POINT ( 'NONE',  ( 181.0000000000000000, 10.00000000000006395, -350.0000000000001705 ) ) ;
#20797 = EDGE_CURVE ( 'NONE', #28550, #29366, #6854, .T. ) ;
#20798 = LINE ( 'NONE', #40068, #4011 ) ;
#20799 = DIRECTION ( 'NONE',  ( 1.000000000000000000, 0.000000000000000000, 0.000000000000000000 ) ) ;
#20800 = VECTOR ( 'NONE', #15343, 1000.000000000000000 ) ;
#20801 = EDGE_CURVE ( 'NONE', #11997, #49578, #19280, .T. ) ;
#20802 = DIRECTION ( 'NONE',  ( 0.000000000000000000, 0.000000000000000000, -1.000000000000000000 ) ) ;
#20803 = EDGE_CURVE ( 'NONE', #17104, #7818, #22616, .T. ) ;
#20804 = EDGE_LOOP ( 'NONE', ( #32977, #28766, #48811 ) ) ;
#20805 = CARTESIAN_POINT ( 'NONE',  ( 115.0540265531850395, 1.025126265847081886, -120.9317124430720440 ) ) ;
#20806 = EDGE_LOOP ( 'NONE', ( #7205, #4882, #4685, #42828 ) ) ;
#20807 = CARTESIAN_POINT ( 'NONE',  ( 12.97493236725083676, -11.05939663306990717, 8.953103998512858652 ) ) ;
#20808 = ORIENTED_EDGE ( 'NONE', *, *, #32856, .T. ) ;
#20809 = LINE ( 'NONE', #33146, #23787 ) ;
#20810 = CARTESIAN_POINT ( 'NONE',  ( -206.6959734468149463, 1.750000000000010658, -119.1817124430720440 ) ) ;
#20811 = EDGE_CURVE ( 'NONE', #1663, #25007, #31339, .T. ) ;
#20812 = DIRECTION ( 'NONE',  ( -0.000000000000000000, -1.000000000000000000, -0.000000000000000000 ) ) ;
#20813 = CARTESIAN_POINT ( 'NONE',  ( 210.0000000000000568, 0.000000000000000000, 160.8182875569279702 ) ) ;
#20814 = EDGE_LOOP ( 'NONE', ( #7974, #14165, #4608, #16589 ) ) ;
#20815 = AXIS2_PLACEMENT_3D ( 'NONE', #4012, #19409, #43761 ) ;
#20816 = CARTESIAN_POINT ( 'NONE',  ( -6.219530239386607207, 7.848697864701671634, 6.429802539306387565 ) ) ;
#20817 = EDGE_LOOP ( 'NONE', ( #19227, #25640, #28606, #33123, #15243, #49697 ) ) ;
#20818 = DIRECTION ( 'NONE',  ( -1.000000000000000000, -0.000000000000000000, -0.000000000000000000 ) ) ;
#20819 = CARTESIAN_POINT ( 'NONE',  ( 1.769963848780946369, -9.842115015280432644, 0.000000000000000000 ) ) ;
#20820 = CYLINDRICAL_SURFACE ( 'NONE', #22147, 1.750000000000015543 ) ;
#20821 = FACE_OUTER_BOUND ( 'NONE', #11623, .T. ) ;
#20822 = CARTESIAN_POINT ( 'NONE',  ( 14.29087950072012170, 9.652079258044652832, 8.727788335465566760 ) ) ;
#20823 = EDGE_LOOP ( 'NONE', ( #21714, #1808, #32843, #41081 ) ) ;
#20825 = EDGE_LOOP ( 'NONE', ( #12925, #42535, #12135, #31215, #46589, #45333 ) ) ;
#20824 = ADVANCED_FACE ( 'NONE', ( #39285 ), #11576, .T. ) ;
#20826 = DIRECTION ( 'NONE',  ( 0.000000000000000000, -1.000000000000000000, 0.000000000000000000 ) ) ;
#20827 = EDGE_CURVE ( 'NONE', #33640, #7390, #31076, .T. ) ;
#20828 = EDGE_CURVE ( 'NONE', #12798, #49396, #21068, .T. ) ;
#20829 = ADVANCED_FACE ( 'NONE', ( #28241 ), #12083, .F. ) ;
#20830 = ORIENTED_EDGE ( 'NONE', *, *, #30899, .F. ) ;
#20831 = LINE ( 'NONE', #1348, #23323 ) ;
#20832 = DIRECTION ( 'NONE',  ( -0.000000000000000000, -1.000000000000000000, -0.000000000000000000 ) ) ;
#20833 = AXIS2_PLACEMENT_3D ( 'NONE', #11188, #6061, #2218 ) ;
#20834 = LINE ( 'NONE', #11885, #45261 ) ;
#20835 = VERTEX_POINT ( 'NONE', #23624 ) ;
#20836 = DIRECTION ( 'NONE',  ( -0.000000000000000000, 1.000000000000000000, 1.224646799147353207E-16 ) ) ;
#20837 = EDGE_CURVE ( 'NONE', #22255, #290, #49195, .T. ) ;
#20838 = AXIS2_PLACEMENT_3D ( 'NONE', #35921, #34913, #39262 ) ;
#20839 = EDGE_CURVE ( 'NONE', #43085, #17801, #12571, .T. ) ;
#20840 = CARTESIAN_POINT ( 'NONE',  ( 341.6568542494924259, 164.9999999999999716, 339.9999999999998295 ) ) ;
#20841 = VECTOR ( 'NONE', #17926, 1000.000000000000000 ) ;
#20842 = CARTESIAN_POINT ( 'NONE',  ( 1.158497635116737312, -16.61944452314319420, -3.546734833711462365 ) ) ;
#20843 = DIRECTION ( 'NONE',  ( -1.000000000000000000, -0.000000000000000000, -0.000000000000000000 ) ) ;
#20844 = CYLINDRICAL_SURFACE ( 'NONE', #33172, 2.000000000000001776 ) ;
#20845 = DIRECTION ( 'NONE',  ( -0.000000000000000000, -0.000000000000000000, -1.000000000000000000 ) ) ;
#20846 = ORIENTED_EDGE ( 'NONE', *, *, #3635, .T. ) ;
#20847 = ORIENTED_EDGE ( 'NONE', *, *, #46939, .F. ) ;
#20848 = ORIENTED_EDGE ( 'NONE', *, *, #12488, .F. ) ;
#20849 = CARTESIAN_POINT ( 'NONE',  ( -5.000000000000000000, -175.0000000000000284, 350.0000000000002274 ) ) ;
#20850 = CARTESIAN_POINT ( 'NONE',  ( -165.0000000000000284, 16.00000000000000000, 90.00000000000000000 ) ) ;
#20851 = CARTESIAN_POINT ( 'NONE',  ( -4.999999999999948486, -214.9999999999999716, -230.2499999999999716 ) ) ;
#20852 = ORIENTED_EDGE ( 'NONE', *, *, #46631, .T. ) ;
#20853 = ADVANCED_FACE ( 'NONE', ( #31847 ), #39545, .T. ) ;
#20854 = DIRECTION ( 'NONE',  ( -0.000000000000000000, -0.000000000000000000, -1.000000000000000000 ) ) ;
#20855 = ORIENTED_EDGE ( 'NONE', *, *, #50220, .F. ) ;
#20856 = CARTESIAN_POINT ( 'NONE',  ( -3.229232847726260403, 16.57333684275945629, 9.178419661560148768 ) ) ;
#20857 = DIRECTION ( 'NONE',  ( -0.000000000000000000, -0.000000000000000000, -1.000000000000000000 ) ) ;
#20858 = CARTESIAN_POINT ( 'NONE',  ( -166.6959734468149463, 1.750000000000010658, -119.1817124430720440 ) ) ;
#20859 = CIRCLE ( 'NONE', #5327, 4.000000000000003553 ) ;
#20860 = ADVANCED_FACE ( 'NONE', ( #24147 ), #19506, .T. ) ;
#20861 = EDGE_CURVE ( 'NONE', #14457, #49709, #39797, .T. ) ;
#20862 = CARTESIAN_POINT ( 'NONE',  ( 23.79193388295309219, 28.98609808355011452, -9.422646554964176246 ) ) ;
#20863 =( BOUNDED_CURVE ( )  B_SPLINE_CURVE ( 3, ( #3167, #45499, #22682, #7287 ),
 .UNSPECIFIED., .F., .F. ) 
 B_SPLINE_CURVE_WITH_KNOTS ( ( 4, 4 ),
 ( 3.141592653589793116, 4.712388980384689674 ),
 .UNSPECIFIED. ) 
 CURVE ( )  GEOMETRIC_REPRESENTATION_ITEM ( )  RATIONAL_B_SPLINE_CURVE ( ( 1.000000000000000000, 0.8047378541243649375, 0.8047378541243649375, 1.000000000000000000 ) ) 
 REPRESENTATION_ITEM ( '' )  );
#20864 = CARTESIAN_POINT ( 'NONE',  ( 0.5672860446885946706, 37.53182223685058716, -6.568693074176339408 ) ) ;
#20865 = CIRCLE ( 'NONE', #43893, 1.750000000000015543 ) ;
#20866 = CARTESIAN_POINT ( 'NONE',  ( -128.4459734468149179, 0.000000000000000000, 79.06828755692799859 ) ) ;
#20867 = ORIENTED_EDGE ( 'NONE', *, *, #38385, .F. ) ;
#20868 = CARTESIAN_POINT ( 'NONE',  ( -46.69597344681494633, -1.750000000000009992, 0.8182875569279768335 ) ) ;
#20869 = CARTESIAN_POINT ( 'NONE',  ( -36.28567981536816234, -9.465698090293395595, -9.422646554964174470 ) ) ;
#20870 = CARTESIAN_POINT ( 'NONE',  ( -29.61572577327014955, -16.11461842845715253, 8.807470649214879543 ) ) ;
#20871 = EDGE_CURVE ( 'NONE', #13001, #42210, #21697, .T. ) ;
#20872 = CARTESIAN_POINT ( 'NONE',  ( -5.000000000000000000, -165.1999999999999602, 359.7999999999997840 ) ) ;
#20873 = ORIENTED_EDGE ( 'NONE', *, *, #2849, .T. ) ;
#20874 = VECTOR ( 'NONE', #40663, 1000.000000000000000 ) ;
#20875 = DIRECTION ( 'NONE',  ( -0.000000000000000000, 1.000000000000000000, 0.000000000000000000 ) ) ;
#20876 = ORIENTED_EDGE ( 'NONE', *, *, #19868, .F. ) ;
#20877 = CARTESIAN_POINT ( 'NONE',  ( -86.69597344681494633, -1.750000000000009992, 0.8182875569279768335 ) ) ;
#20878 = DIRECTION ( 'NONE',  ( -0.000000000000000000, -0.000000000000000000, -1.000000000000000000 ) ) ;
#20879 = VECTOR ( 'NONE', #34880, 1000.000000000000000 ) ;
#20880 = EDGE_LOOP ( 'NONE', ( #6368, #35779, #47023, #23583 ) ) ;
#20881 = ORIENTED_EDGE ( 'NONE', *, *, #3463, .T. ) ;
#20882 = DIRECTION ( 'NONE',  ( 0.000000000000000000, 2.537652627714642000E-15, 1.000000000000000000 ) ) ;
#20883 = PLANE ( 'NONE',  #9101 ) ;
#20884 = EDGE_CURVE ( 'NONE', #5777, #21583, #4892, .T. ) ;
#20885 = CARTESIAN_POINT ( 'NONE',  ( -31.93002621080269421, -9.285431160462335853, -2.408242355805840784 ) ) ;
#20886 = FACE_OUTER_BOUND ( 'NONE', #36908, .T. ) ;
#20887 = ORIENTED_EDGE ( 'NONE', *, *, #26455, .F. ) ;
#20888 = EDGE_LOOP ( 'NONE', ( #13858, #35015, #11582, #21326 ) ) ;
#20889 = PLANE ( 'NONE',  #4590 ) ;
#20890 = CARTESIAN_POINT ( 'NONE',  ( 13.92102703536701114, 30.85732372859822803, 8.356839323120299312 ) ) ;
#20891 = EDGE_CURVE ( 'NONE', #22581, #46920, #40047, .T. ) ;
#20892 = VECTOR ( 'NONE', #35367, 1000.000000000000000 ) ;
#20893 = EDGE_CURVE ( 'NONE', #47273, #18535, #27802, .T. ) ;
#20894 = EDGE_LOOP ( 'NONE', ( #33519, #38162, #12075, #4901 ) ) ;
#20895 = EDGE_LOOP ( 'NONE', ( #26443, #23655, #18714, #25204, #27955 ) ) ;
#20896 = CARTESIAN_POINT ( 'NONE',  ( 10.49999999999996092, 13.59802227364768967, -19.51251772323705325 ) ) ;
#20897 = CARTESIAN_POINT ( 'NONE',  ( -206.6959734468149463, -1.750000000000010658, 80.81828755692798438 ) ) ;
#20898 = CARTESIAN_POINT ( 'NONE',  ( 75.05402655318509630, 2.143131898507880377E-16, -160.9317124430720582 ) ) ;
#20899 = ORIENTED_EDGE ( 'NONE', *, *, #40874, .F. ) ;
#20900 = TOROIDAL_SURFACE ( 'NONE', #41376, 4.250000000000000000, 0.5000000000000000000 ) ;
#20901 = VERTEX_POINT ( 'NONE', #46930 ) ;
#20902 = ORIENTED_EDGE ( 'NONE', *, *, #32619, .F. ) ;
#20903 = EDGE_CURVE ( 'NONE', #34748, #39727, #548, .T. ) ;
#20904 = ADVANCED_FACE ( 'NONE', ( #20532 ), #289, .T. ) ;
#20905 = DIRECTION ( 'NONE',  ( -0.000000000000000000, -1.000000000000000000, -0.000000000000000000 ) ) ;
#20906 = EDGE_CURVE ( 'NONE', #28949, #13072, #10184, .T. ) ;
#20907 = MECHANICAL_DESIGN_GEOMETRIC_PRESENTATION_REPRESENTATION (  '', ( #25019 ), #18440 ) ;
#20908 = LINE ( 'NONE', #41607, #13956 ) ;
#20909 = VECTOR ( 'NONE', #47869, 1000.000000000000000 ) ;
#20910 = ORIENTED_EDGE ( 'NONE', *, *, #5481, .T. ) ;
#20911 = ORIENTED_EDGE ( 'NONE', *, *, #6149, .F. ) ;
#20912 = CARTESIAN_POINT ( 'NONE',  ( 2.462075149652696027, -16.57295996686994499, 9.403735324607438884 ) ) ;
#20913 = DIRECTION ( 'NONE',  ( -0.000000000000000000, -1.000000000000000000, -0.000000000000000000 ) ) ;
#20914 = PRODUCT_DEFINITION_FORMATION_WITH_SPECIFIED_SOURCE ( 'ANY', '', #37631, .NOT_KNOWN. ) ;
#20915 = ORIENTED_EDGE ( 'NONE', *, *, #8552, .T. ) ;
#20916 = B_SPLINE_CURVE_WITH_KNOTS ( 'NONE', 3,
 ( #38332, #18791, #50568, #23159 ),
 .UNSPECIFIED., .F., .F.,
 ( 4, 4 ),
 ( 0.000000000000000000, 0.001246897409371945480 ),
 .UNSPECIFIED. ) ;
#20917 = ORIENTED_EDGE ( 'NONE', *, *, #10442, .T. ) ;
#20918 = AXIS2_PLACEMENT_3D ( 'NONE', #35788, #39877, #24215 ) ;
#20919 = CARTESIAN_POINT ( 'NONE',  ( -64.99999999999783995, 17.00000000000000000, 95.00000000000000000 ) ) ;
#20920 = CARTESIAN_POINT ( 'NONE',  ( -8.760073316077733097, 197.4999999999999432, -228.6347188485896140 ) ) ;
#20921 = ORIENTED_EDGE ( 'NONE', *, *, #3598, .T. ) ;
#20922 =( BOUNDED_CURVE ( )  B_SPLINE_CURVE ( 3, ( #13842, #6412, #10510, #33133 ),
 .UNSPECIFIED., .F., .F. ) 
 B_SPLINE_CURVE_WITH_KNOTS ( ( 4, 4 ),
 ( 1.570796326794896558, 3.141592653589793116 ),
 .UNSPECIFIED. ) 
 CURVE ( )  GEOMETRIC_REPRESENTATION_ITEM ( )  RATIONAL_B_SPLINE_CURVE ( ( 1.000000000000000000, 0.8047378541243649375, 0.8047378541243649375, 1.000000000000000000 ) ) 
 REPRESENTATION_ITEM ( '' )  );
#20923 = LINE ( 'NONE', #37102, #23789 ) ;
#20924 = CARTESIAN_POINT ( 'NONE',  ( -1.780619886013952602, -1.041246721325602920, 9.886433018048069954 ) ) ;
#20925 = DIRECTION ( 'NONE',  ( 0.000000000000000000, 0.000000000000000000, 1.000000000000000000 ) ) ;
#20926 = EDGE_CURVE ( 'NONE', #13001, #27141, #38160, .T. ) ;
#20927 = CARTESIAN_POINT ( 'NONE',  ( 34.38425513258721367, -36.82177522737820397, 8.807470649214879543 ) ) ;
#20928 = ORIENTED_EDGE ( 'NONE', *, *, #5268, .T. ) ;
#20929 = CARTESIAN_POINT ( 'NONE',  ( -48.99656738986512039, 11.00747004110376182, 1.847720168420772691 ) ) ;
#20930 =( BOUNDED_CURVE ( )  B_SPLINE_CURVE ( 3, ( #12866, #16219, #35985, #47223 ),
 .UNSPECIFIED., .F., .F. ) 
 B_SPLINE_CURVE_WITH_KNOTS ( ( 4, 4 ),
 ( 3.141592653589793560, 4.712388980384696779 ),
 .UNSPECIFIED. ) 
 CURVE ( )  GEOMETRIC_REPRESENTATION_ITEM ( )  RATIONAL_B_SPLINE_CURVE ( ( 1.000000000000000000, 0.8047378541243634942, 0.8047378541243634942, 1.000000000000000000 ) ) 
 REPRESENTATION_ITEM ( '' )  );
#20931 = CARTESIAN_POINT ( 'NONE',  ( 15.62858259096121216, -5.755205073598614440, -9.683996418299976483 ) ) ;
#20932 = CARTESIAN_POINT ( 'NONE',  ( -165.0000000000000284, 16.00000000000000000, -30.00000000000000000 ) ) ;
#20933 = CARTESIAN_POINT ( 'NONE',  ( -36.02002318912981593, 10.56068015588366116, -3.721387749823083624 ) ) ;
#20934 = VECTOR ( 'NONE', #5674, 1000.000000000000000 ) ;
#20935 = VECTOR ( 'NONE', #40506, 1000.000000000000000 ) ;
#20936 = DIRECTION ( 'NONE',  ( -3.363195139050033768E-16, -0.7071067811865474617, -0.7071067811865475727 ) ) ;
#20937 = CARTESIAN_POINT ( 'NONE',  ( 181.0000000000000000, -81.49999999999997158, -340.0000000000001137 ) ) ;
#20938 = AXIS2_PLACEMENT_3D ( 'NONE', #37305, #22626, #37793 ) ;
#20940 = CARTESIAN_POINT ( 'NONE',  ( -5.000000000000000000, -184.7999999999999545, 340.1999999999997044 ) ) ;
#20939 =( BOUNDED_CURVE ( )  B_SPLINE_CURVE ( 3, ( #18622, #38657, #19395, #163 ),
 .UNSPECIFIED., .F., .F. ) 
 B_SPLINE_CURVE_WITH_KNOTS ( ( 4, 4 ),
 ( 4.712388980384689674, 6.283185307179586232 ),
 .UNSPECIFIED. ) 
 CURVE ( )  GEOMETRIC_REPRESENTATION_ITEM ( )  RATIONAL_B_SPLINE_CURVE ( ( 1.000000000000000000, 0.8047378541243649375, 0.8047378541243649375, 1.000000000000000000 ) ) 
 REPRESENTATION_ITEM ( '' )  );
#20941 = LINE ( 'NONE', #5025, #49197 ) ;
#20942 = EDGE_LOOP ( 'NONE', ( #40682, #16348, #15447, #24808 ) ) ;
#20943 = CARTESIAN_POINT ( 'NONE',  ( -6.508636631827791064, -15.75743548351446854, 8.953103998512858652 ) ) ;
#20944 = PRESENTATION_LAYER_ASSIGNMENT (  '', '', ( #29957 ) ) ;
#20945 = CARTESIAN_POINT ( 'NONE',  ( 0.000000000000000000, 28.48684210526315752, 0.000000000000000000 ) ) ;
#20946 = VECTOR ( 'NONE', #28984, 1000.000000000000000 ) ;
#20947 = VERTEX_POINT ( 'NONE', #2231 ) ;
#20948 = FACE_OUTER_BOUND ( 'NONE', #28598, .T. ) ;
#20949 = CARTESIAN_POINT ( 'NONE',  ( 25.61277432017878297, -22.36370378792834757, 7.906207997025717304 ) ) ;
#20950 = CARTESIAN_POINT ( 'NONE',  ( 341.9999999999999432, 181.0000000000001705, -356.0000000000003411 ) ) ;
#20951 = VERTEX_POINT ( 'NONE', #49386 ) ;
#20952 = CARTESIAN_POINT ( 'NONE',  ( -1.565927753002675615, 1.491090762200759423, 9.882710035074767418 ) ) ;
#20953 = ORIENTED_EDGE ( 'NONE', *, *, #48405, .F. ) ;
#20954 = CIRCLE ( 'NONE', #4589, 5.000000000000000000 ) ;
#20955 = DIRECTION ( 'NONE',  ( 0.000000000000000000, -1.000000000000000000, 1.822804496942679766E-16 ) ) ;
#20956 = VECTOR ( 'NONE', #19873, 1000.000000000000000 ) ;
#20957 = CARTESIAN_POINT ( 'NONE',  ( 1.224837355096363156, 1.100071488488148619, 9.927568724237747944 ) ) ;
#20958 = ADVANCED_FACE ( 'NONE', ( #6336 ), #26081, .F. ) ;
#20959 = EDGE_CURVE ( 'NONE', #6771, #43286, #22882, .T. ) ;
#20960 = ORIENTED_EDGE ( 'NONE', *, *, #32808, .F. ) ;
#20961 = DIRECTION ( 'NONE',  ( 0.000000000000000000, 1.000000000000000000, 0.000000000000000000 ) ) ;
#20962 = CARTESIAN_POINT ( 'NONE',  ( 181.0000000000000000, -5.999999999999950262, -350.0000000000001705 ) ) ;
#20963 = VERTEX_POINT ( 'NONE', #2481 ) ;
#20964 = ORIENTED_EDGE ( 'NONE', *, *, #12681, .F. ) ;
#20965 = ADVANCED_FACE ( 'NONE', ( #22235 ), #45799, .T. ) ;
#20966 = CARTESIAN_POINT ( 'NONE',  ( 181.0000000000000000, -79.49999999999997158, -340.0000000000001137 ) ) ;
#20967 = ORIENTED_EDGE ( 'NONE', *, *, #50436, .T. ) ;
#20969 = EDGE_CURVE ( 'NONE', #11192, #5304, #17868, .T. ) ;
#20968 = CARTESIAN_POINT ( 'NONE',  ( 0.5359691244547075684, -1.100286284792932889, 9.966990753365129407 ) ) ;
#20970 = CARTESIAN_POINT ( 'NONE',  ( -5.000000000000000000, -184.7999999999999545, 359.7999999999997840 ) ) ;
#20971 = ADVANCED_FACE ( 'NONE', ( #14527 ), #6839, .T. ) ;
#20972 = DIRECTION ( 'NONE',  ( 1.000000000000000000, 0.000000000000000000, 0.000000000000000000 ) ) ;
#20973 = VECTOR ( 'NONE', #7851, 1000.000000000000000 ) ;
#20974 = ORIENTED_EDGE ( 'NONE', *, *, #47148, .T. ) ;
#20975 = CARTESIAN_POINT ( 'NONE',  ( -50.13037131770489907, 47.08801056904012228, 741.9425600500172777 ) ) ;
#20976 =( LENGTH_UNIT ( ) NAMED_UNIT ( * ) SI_UNIT ( .MILLI., .METRE. ) );
#20977 = EDGE_LOOP ( 'NONE', ( #12058, #19908, #34286, #1685 ) ) ;
#20978 = CIRCLE ( 'NONE', #42246, 4.000000000000003553 ) ;
#20979 = EDGE_LOOP ( 'NONE', ( #4363, #21459, #37154, #34652 ) ) ;
#20980 = VERTEX_POINT ( 'NONE', #40292 ) ;
#20981 = CARTESIAN_POINT ( 'NONE',  ( 24.39427009665985224, 44.07992421011656603, 8.807470649214879543 ) ) ;
#20982 = EDGE_CURVE ( 'NONE', #6876, #6581, #24697, .T. ) ;
#20983 = LINE ( 'NONE', #17374, #8653 ) ;
#20984 = ORIENTED_EDGE ( 'NONE', *, *, #50038, .T. ) ;
#20985 = DIRECTION ( 'NONE',  ( 1.110223024625156171E-16, -0.7071067811865474617, 0.7071067811865474617 ) ) ;
#20986 = CARTESIAN_POINT ( 'NONE',  ( -5.670847180967843570, -1.750000000000023315, -0.2068387089191201234 ) ) ;
#20987 = VECTOR ( 'NONE', #37644, 1000.000000000000000 ) ;
#20988 = CARTESIAN_POINT ( 'NONE',  ( -45.67084718096785423, 1.750000000000009548, 41.84341382277508359 ) ) ;
#20989 = FACE_OUTER_BOUND ( 'NONE', #35829, .T. ) ;
#20990 = CARTESIAN_POINT ( 'NONE',  ( 165.0000000000000000, -180.9999999999999716, -115.0000000000001421 ) ) ;
#20991 = CARTESIAN_POINT ( 'NONE',  ( 15.80799809827373004, -29.65358618225706522, -8.016098858316199838 ) ) ;
#20992 = CARTESIAN_POINT ( 'NONE',  ( -86.69597344681494633, 1.750000000000010658, -119.1817124430720440 ) ) ;
#20993 = CARTESIAN_POINT ( 'NONE',  ( -206.6959734468149463, 1.750000000000009992, -159.1817124430720298 ) ) ;
#20994 = LINE ( 'NONE', #24845, #1495 ) ;
#20995 = VECTOR ( 'NONE', #30421, 1000.000000000000000 ) ;
#20996 = LINE ( 'NONE', #12785, #29823 ) ;
#20997 = ORIENTED_EDGE ( 'NONE', *, *, #8468, .T. ) ;
#20998 = LINE ( 'NONE', #23845, #32734 ) ;
#20999 = CARTESIAN_POINT ( 'NONE',  ( -6.695973446814940111, 1.750000000000024203, -119.1817124430720440 ) ) ;
#21000 = CARTESIAN_POINT ( 'NONE',  ( 210.0000000000000568, 2.143131898507880377E-16, 159.0682875569279702 ) ) ;
#21001 = DIRECTION ( 'NONE',  ( -0.000000000000000000, -0.000000000000000000, -1.000000000000000000 ) ) ;
#21002 = ADVANCED_FACE ( 'NONE', ( #20778 ), #36458, .T. ) ;
#21003 = ORIENTED_EDGE ( 'NONE', *, *, #18964, .F. ) ;
#21004 = VECTOR ( 'NONE', #17050, 1000.000000000000000 ) ;
#21005 = CARTESIAN_POINT ( 'NONE',  ( -4.999999999999948486, -204.9999999999999716, -234.7500000000000000 ) ) ;
#21006 = AXIS2_PLACEMENT_3D ( 'NONE', #16238, #599, #31899 ) ;
#21007 = DIRECTION ( 'NONE',  ( 1.000000000000000000, 0.000000000000000000, -0.000000000000000000 ) ) ;
#21008 = ORIENTED_EDGE ( 'NONE', *, *, #29580, .T. ) ;
#21009 = B_SPLINE_CURVE_WITH_KNOTS ( 'NONE', 3,
 ( #20927, #28879, #21417, #9376 ),
 .UNSPECIFIED., .F., .F.,
 ( 4, 4 ),
 ( 0.000000000000000000, 0.2562577668812813236 ),
 .UNSPECIFIED. ) ;
#21010 = CARTESIAN_POINT ( 'NONE',  ( -22.18397680750705092, -25.02304503454527662, -8.917361510505369182 ) ) ;
#21011 = CARTESIAN_POINT ( 'NONE',  ( 27.33593271309472073, -41.94268121623323253, -9.367992836599951190 ) ) ;
#21012 = CARTESIAN_POINT ( 'NONE',  ( -48.44597344681496054, 1.025126265847088991, 2.568287556927986159 ) ) ;
#21013 = ORIENTED_EDGE ( 'NONE', *, *, #49926, .T. ) ;
#21014 = LINE ( 'NONE', #37193, #354 ) ;
#21015 = EDGE_LOOP ( 'NONE', ( #24682, #4256, #11227 ) ) ;
#21016 = ORIENTED_EDGE ( 'NONE', *, *, #17201, .T. ) ;
#21017 = AXIS2_PLACEMENT_3D ( 'NONE', #49754, #14652, #30313 ) ;
#21018 = ORIENTED_EDGE ( 'NONE', *, *, #12100, .F. ) ;
#21019 = DIRECTION ( 'NONE',  ( -1.000000000000000000, -0.000000000000000000, -0.000000000000000000 ) ) ;
#21020 = CARTESIAN_POINT ( 'NONE',  ( -86.69597344681494633, 1.750000000000010658, 120.8182875569279702 ) ) ;
#21021 = ORIENTED_EDGE ( 'NONE', *, *, #32344, .F. ) ;
#21022 = CARTESIAN_POINT ( 'NONE',  ( -114.9999999999994031, 17.00000000000000000, -54.99999999999999289 ) ) ;
#21023 = CARTESIAN_POINT ( 'NONE',  ( 10.00000000000000000, 0.000000000000000000, 0.000000000000000000 ) ) ;
#21024 = DIRECTION ( 'NONE',  ( 1.000000000000000000, 0.000000000000000000, 0.000000000000000000 ) ) ;
#21025 = CARTESIAN_POINT ( 'NONE',  ( 21.23829395927641883, 7.611558401714507482, 230.0000000000000000 ) ) ;
#21026 = ORIENTED_EDGE ( 'NONE', *, *, #50584, .T. ) ;
#21027 = AXIS2_PLACEMENT_3D ( 'NONE', #38837, #42905, #39095 ) ;
#21028 = DIRECTION ( 'NONE',  ( 0.000000000000000000, 0.000000000000000000, -1.000000000000000000 ) ) ;
#21029 = ORIENTED_EDGE ( 'NONE', *, *, #39037, .F. ) ;
#21030 = DIRECTION ( 'NONE',  ( -0.000000000000000000, -0.000000000000000000, 1.000000000000000000 ) ) ;
#21031 = DIRECTION ( 'NONE',  ( 3.364279341222521245E-16, 0.7071067811865474617, -0.7071067811865476838 ) ) ;
#21032 = ORIENTED_EDGE ( 'NONE', *, *, #37452, .T. ) ;
#21033 = APPLICATION_CONTEXT ( 'automotive_design' ) ;
#21034 = ORIENTED_EDGE ( 'NONE', *, *, #14239, .F. ) ;
#21035 = ORIENTED_EDGE ( 'NONE', *, *, #21829, .T. ) ;
#21036 = CARTESIAN_POINT ( 'NONE',  ( 85.00000000000123634, 16.00000000000000000, 30.00000000000000000 ) ) ;
#21037 = EDGE_CURVE ( 'NONE', #23031, #39985, #47422, .T. ) ;
#21038 = DIRECTION ( 'NONE',  ( 1.156482317317870492E-16, -1.000000000000000000, -0.000000000000000000 ) ) ;
#21039 = ORIENTED_EDGE ( 'NONE', *, *, #25309, .T. ) ;
#21040 = CARTESIAN_POINT ( 'NONE',  ( 153.3040265531850537, -1.750000000000009992, -159.1817124430720298 ) ) ;
#21041 =( LENGTH_UNIT ( ) NAMED_UNIT ( * ) SI_UNIT ( .MILLI., .METRE. ) );
#21042 = CARTESIAN_POINT ( 'NONE',  ( 0.1291293981302941152, 10.01396644373391887, 3.215203646305365925 ) ) ;
#21043 = VECTOR ( 'NONE', #409, 1000.000000000000000 ) ;
#21044 = ORIENTED_EDGE ( 'NONE', *, *, #2486, .F. ) ;
#21045 = FACE_OUTER_BOUND ( 'NONE', #29811, .T. ) ;
#21046 = LINE ( 'NONE', #36730, #10369 ) ;
#21047 = CARTESIAN_POINT ( 'NONE',  ( -17.34922095635781147, -33.24536858281880569, 8.914903342594564961 ) ) ;
#21048 = ORIENTED_EDGE ( 'NONE', *, *, #22804, .F. ) ;
#21049 = EDGE_LOOP ( 'NONE', ( #33567, #23405, #4801, #26032 ) ) ;
#21050 = PRODUCT_CONTEXT ( 'NONE', #48559, 'mechanical' ) ;
#21051 = CARTESIAN_POINT ( 'NONE',  ( 33.30402655318503946, 0.000000000000000000, -165.0000000000000000 ) ) ;
#21052 = CARTESIAN_POINT ( 'NONE',  ( 84.99999999999997158, 16.00000000000000000, -90.00000000000000000 ) ) ;
#21053 = CARTESIAN_POINT ( 'NONE',  ( -45.64490844644706868, -21.32281559348764333, 8.807470649214879543 ) ) ;
#21054 = CYLINDRICAL_SURFACE ( 'NONE', #26491, 4.000000000000003553 ) ;
#21055 = ORIENTED_EDGE ( 'NONE', *, *, #46925, .T. ) ;
#21056 = DIRECTION ( 'NONE',  ( -1.860490536778032451E-50, 0.000000000000000000, -1.000000000000000000 ) ) ;
#21057 = DIRECTION ( 'NONE',  ( 0.000000000000000000, 0.000000000000000000, 1.000000000000000000 ) ) ;
#21058 = PLANE ( 'NONE',  #5331 ) ;
#21059 = CARTESIAN_POINT ( 'NONE',  ( 0.1265591857323814795, 1.213367045380162823, 9.963925895596176474 ) ) ;
#21060 = ADVANCED_FACE ( 'NONE', ( #45050 ), #33543, .T. ) ;
#21061 = ORIENTED_EDGE ( 'NONE', *, *, #29955, .F. ) ;
#21062 = CARTESIAN_POINT ( 'NONE',  ( -86.69597344681494633, -1.750000000000010658, 80.81828755692798438 ) ) ;
#21063 = ORIENTED_EDGE ( 'NONE', *, *, #35359, .T. ) ;
#21064 = CARTESIAN_POINT ( 'NONE',  ( 24.47767542868285062, -23.18653802921781448, 8.807470649214879543 ) ) ;
#21065 = ORIENTED_EDGE ( 'NONE', *, *, #49935, .T. ) ;
#21066 = DIRECTION ( 'NONE',  ( 0.000000000000000000, -1.000000000000000000, 3.469446951953611033E-15 ) ) ;
#21067 = CARTESIAN_POINT ( 'NONE',  ( -8.864235763825252690, -4.693841405978048442, 9.516222621873129839 ) ) ;
#21068 = B_SPLINE_CURVE_WITH_KNOTS ( 'NONE', 3,
 ( #43875, #42856, #47186, #27482 ),
 .UNSPECIFIED., .F., .F.,
 ( 4, 4 ),
 ( 4.114257970988321555E-18, 0.0004072981213154478700 ),
 .UNSPECIFIED. ) ;
#21069 = DIRECTION ( 'NONE',  ( -0.000000000000000000, -1.000000000000000000, -0.000000000000000000 ) ) ;
#21070 = ORIENTED_EDGE ( 'NONE', *, *, #43141, .F. ) ;
#21071 = VECTOR ( 'NONE', #7672, 1000.000000000000000 ) ;
#21072 = EDGE_LOOP ( 'NONE', ( #5758, #15253, #25172, #30273, #47260, #7802 ) ) ;
#21073 = CARTESIAN_POINT ( 'NONE',  ( 0.7603004677395120980, -1.297166976433627550, 9.936141075690075652 ) ) ;
#21074 = CARTESIAN_POINT ( 'NONE',  ( 50.11058929355270664, -7.578863168071591438, 7.455576670931136185 ) ) ;
#21075 = CARTESIAN_POINT ( 'NONE',  ( -48.44597344681496054, -1.025126265847089435, -40.93171244307204404 ) ) ;
#21076 = LINE ( 'NONE', #14125, #37009 ) ;
#21077 =( BOUNDED_CURVE ( )  B_SPLINE_CURVE ( 3, ( #36504, #5173, #45149, #6192 ),
 .UNSPECIFIED., .F., .F. ) 
 B_SPLINE_CURVE_WITH_KNOTS ( ( 4, 4 ),
 ( 3.141592653589793116, 4.712388980384689674 ),
 .UNSPECIFIED. ) 
 CURVE ( )  GEOMETRIC_REPRESENTATION_ITEM ( )  RATIONAL_B_SPLINE_CURVE ( ( 1.000000000000000000, 0.8047378541243649375, 0.8047378541243649375, 1.000000000000000000 ) ) 
 REPRESENTATION_ITEM ( '' )  );
#21078 = ORIENTED_EDGE ( 'NONE', *, *, #47118, .T. ) ;
#21079 = EDGE_LOOP ( 'NONE', ( #41563, #13299 ) ) ;
#21080 = CARTESIAN_POINT ( 'NONE',  ( 344.0000000000000568, 165.0000000000000000, 349.9999999999998295 ) ) ;
#21081 = ORIENTED_EDGE ( 'NONE', *, *, #22075, .T. ) ;
#21082 = CYLINDRICAL_SURFACE ( 'NONE', #24286, 1.750000000000015543 ) ;
#21083 = DIRECTION ( 'NONE',  ( -1.000000000000000000, -0.000000000000000000, -0.000000000000000000 ) ) ;
#21084 = EDGE_LOOP ( 'NONE', ( #23155, #13661, #41346 ) ) ;
#21085 = DIRECTION ( 'NONE',  ( -1.000000000000000000, 1.156482317317871478E-16, 0.000000000000000000 ) ) ;
#21086 = EDGE_CURVE ( 'NONE', #31054, #13689, #30029, .T. ) ;
#21087 = DIRECTION ( 'NONE',  ( 1.368455531567204171E-48, -1.000000000000000000, -2.265761274745217480E-16 ) ) ;
#21088 = B_SPLINE_SURFACE_WITH_KNOTS ( 'NONE', 3, 3, ( 
 ( #21288, #48937, #37472, #13823 ),
 ( #41292, #6394, #44859, #1797 ),
 ( #37715, #17443, #33115, #40794 ),
 ( #18185, #41047, #5887, #22042 ) ),
 .UNSPECIFIED., .F., .F., .F.,
 ( 4, 4 ),
 ( 4, 4 ),
 ( 0.000000000000000000, 1.000000000000000000 ),
 ( 0.000000000000000000, 1.000000000000000000 ),
 .UNSPECIFIED. ) ;
#21089 = ORIENTED_EDGE ( 'NONE', *, *, #8935, .T. ) ;
#21090 = DIRECTION ( 'NONE',  ( 4.625929269271584521E-16, -0.000000000000000000, 1.000000000000000000 ) ) ;
#21091 = CARTESIAN_POINT ( 'NONE',  ( -19.99999999999940670, 16.00000000000000000, -54.99999999999999289 ) ) ;
#21092 = DIRECTION ( 'NONE',  ( 0.000000000000000000, 0.000000000000000000, 1.000000000000000000 ) ) ;
#21093 = DIRECTION ( 'NONE',  ( -1.000000000000000000, 0.000000000000000000, 0.000000000000000000 ) ) ;
#21094 = ORIENTED_EDGE ( 'NONE', *, *, #46000, .F. ) ;
#21095 = ORIENTED_EDGE ( 'NONE', *, *, #46223, .T. ) ;
#21096 = ORIENTED_EDGE ( 'NONE', *, *, #28205, .T. ) ;
#21097 = CARTESIAN_POINT ( 'NONE',  ( -167.4999999999999432, -62.49999999999998579, -18.87174264961130987 ) ) ;
#21098 = B_SPLINE_CURVE_WITH_KNOTS ( 'NONE', 3,
 ( #28443, #32298, #1989, #45057 ),
 .UNSPECIFIED., .F., .F.,
 ( 4, 4 ),
 ( 0.000000000000000000, 0.002466147708923232748 ),
 .UNSPECIFIED. ) ;
#21099 = DIRECTION ( 'NONE',  ( -1.000000000000000000, 0.000000000000000000, 0.000000000000000000 ) ) ;
#21100 = EDGE_CURVE ( 'NONE', #14002, #9039, #20939, .T. ) ;
#21101 = DIRECTION ( 'NONE',  ( 0.8637789008984335659, -0.000000000000000000, 0.5038710255240859137 ) ) ;
#21102 = EDGE_CURVE ( 'NONE', #7456, #18807, #40278, .T. ) ;
#21103 = CARTESIAN_POINT ( 'NONE',  ( -8.277096487746778308, 33.14818118907697198, 7.455576670931136185 ) ) ;
#21104 = ORIENTED_EDGE ( 'NONE', *, *, #39511, .T. ) ;
#21105 = FACE_OUTER_BOUND ( 'NONE', #23992, .T. ) ;
#21106 = ORIENTED_EDGE ( 'NONE', *, *, #33550, .F. ) ;
#21107 = EDGE_CURVE ( 'NONE', #47806, #6245, #26484, .T. ) ;
#21108 = LINE ( 'NONE', #5211, #26120 ) ;
#21109 = CARTESIAN_POINT ( 'NONE',  ( 1.448406091252584238, -0.9360325558322883932, 9.928159647716132241 ) ) ;
#21110 = DIRECTION ( 'NONE',  ( 1.000000000000000000, 0.000000000000000000, 0.000000000000000000 ) ) ;
#21111 = AXIS2_PLACEMENT_3D ( 'NONE', #12650, #28058, #24724 ) ;
#21112 = CYLINDRICAL_SURFACE ( 'NONE', #48727, 1.750000000000015543 ) ;
#21113 = DIRECTION ( 'NONE',  ( -1.000000000000000000, 0.000000000000000000, 0.000000000000000000 ) ) ;
#21114 = CARTESIAN_POINT ( 'NONE',  ( 32.27890028733795447, 1.750000000000009548, 81.84341382277507648 ) ) ;
#21115 = ORIENTED_EDGE ( 'NONE', *, *, #36055, .F. ) ;
#21116 = CARTESIAN_POINT ( 'NONE',  ( 73.30402655318508209, 1.750000000000009992, 0.8182875569279768335 ) ) ;
#21117 = CARTESIAN_POINT ( 'NONE',  ( 35.05402655318504657, 2.143131898507880377E-16, -40.93171244307205825 ) ) ;
#21118 = CARTESIAN_POINT ( 'NONE',  ( -30.77287599203642188, -12.70002479445974686, 3.199614146704519602 ) ) ;
#21119 = ADVANCED_FACE ( 'NONE', ( #19650 ), #22735, .T. ) ;
#21120 = EDGE_CURVE ( 'NONE', #16449, #18930, #23763, .T. ) ;
#21121 = EDGE_CURVE ( 'NONE', #32184, #35676, #3998, .T. ) ;
#21122 = EDGE_CURVE ( 'NONE', #16798, #46080, #17749, .T. ) ;
#21123 = DIRECTION ( 'NONE',  ( 1.000000000000000000, -4.758098676964957447E-16, 2.958228394578795584E-31 ) ) ;
#21124 = ORIENTED_EDGE ( 'NONE', *, *, #44448, .F. ) ;
#21125 = DIRECTION ( 'NONE',  ( 1.333906992743555050E-23, -1.000000000000000000, 0.000000000000000000 ) ) ;
#21126 = ORIENTED_EDGE ( 'NONE', *, *, #29025, .T. ) ;
#21127 = CARTESIAN_POINT ( 'NONE',  ( -5.670847180967843570, 1.750000000000023537, -78.15658617722490931 ) ) ;
#21128 = CARTESIAN_POINT ( 'NONE',  ( 75.05402655318509630, 2.143131898507880377E-16, 2.568287556928006143 ) ) ;
#21129 = AXIS2_PLACEMENT_3D ( 'NONE', #6292, #29880, #11149 ) ;
#21130 = EDGE_CURVE ( 'NONE', #22165, #15558, #2061, .T. ) ;
#21131 = CARTESIAN_POINT ( 'NONE',  ( 4.204997580903516941, 7.611558401714507482, 229.0000000000000000 ) ) ;
#21132 = VERTEX_POINT ( 'NONE', #38409 ) ;
#21133 = CARTESIAN_POINT ( 'NONE',  ( 5.888214538810389698, 16.20866436362417673, 8.727788335465566760 ) ) ;
#21134 = FACE_OUTER_BOUND ( 'NONE', #49456, .T. ) ;
#21135 = CARTESIAN_POINT ( 'NONE',  ( 358.0000000000000000, 167.8284271247464972, -342.8284271247466108 ) ) ;
#21136 = LINE ( 'NONE', #49296, #16033 ) ;
#21137 = VERTEX_POINT ( 'NONE', #3221 ) ;
#21138 = ORIENTED_EDGE ( 'NONE', *, *, #45707, .F. ) ;
#21139 = EDGE_CURVE ( 'NONE', #4734, #24760, #38341, .T. ) ;
#21140 = CYLINDRICAL_SURFACE ( 'NONE', #6240, 1.750000000000001554 ) ;
#21141 = CARTESIAN_POINT ( 'NONE',  ( 44.99506233596247995, 23.32283626942318833, 7.455576670931136185 ) ) ;
#21142 = EDGE_CURVE ( 'NONE', #25272, #2948, #46551, .T. ) ;
#21143 = VERTEX_POINT ( 'NONE', #22981 ) ;
#21144 = EDGE_CURVE ( 'NONE', #11740, #45663, #31749, .T. ) ;
#21145 = ORIENTED_EDGE ( 'NONE', *, *, #2475, .F. ) ;
#21146 = DIRECTION ( 'NONE',  ( 0.000000000000000000, -1.000000000000000000, 3.469446951953611033E-15 ) ) ;
#21147 = LINE ( 'NONE', #28594, #46211 ) ;
#21148 = CARTESIAN_POINT ( 'NONE',  ( -167.7210997126620384, 1.750000000000009548, 159.7931612910809065 ) ) ;
#21149 = MANIFOLD_SOLID_BREP ( 'Square tube 20 X 20 X 2(1)[15]', #14630 ) ;
#21150 = CARTESIAN_POINT ( 'NONE',  ( -1.721971274562257515, -0.09408549481333014497, 9.928159647716187308 ) ) ;
#21151 = VERTEX_POINT ( 'NONE', #47815 ) ;
#21152 = ORIENTED_EDGE ( 'NONE', *, *, #48039, .T. ) ;
#21153 = EDGE_CURVE ( 'NONE', #34586, #30983, #15311, .T. ) ;
#21154 = EDGE_LOOP ( 'NONE', ( #6664, #32116, #3563, #24625 ) ) ;
#21155 = ADVANCED_FACE ( 'NONE', ( #661 ), #40045, .T. ) ;
#21156 = DIRECTION ( 'NONE',  ( -0.000000000000000000, -0.000000000000000000, -1.000000000000000000 ) ) ;
#21157 = DIRECTION ( 'NONE',  ( 0.000000000000000000, 0.7071067811865473507, -0.7071067811865476838 ) ) ;
#21158 = ORIENTED_EDGE ( 'NONE', *, *, #32264, .T. ) ;
#21159 = VERTEX_POINT ( 'NONE', #28113 ) ;
#21160 = CARTESIAN_POINT ( 'NONE',  ( 34.32915281903212446, -1.750000000000009548, -0.2068387089191121020 ) ) ;
#21161 = LINE ( 'NONE', #1674, #46970 ) ;
#21162 = VERTEX_POINT ( 'NONE', #13207 ) ;
#21163 = ORIENTED_EDGE ( 'NONE', *, *, #35294, .T. ) ;
#21164 = FACE_OUTER_BOUND ( 'NONE', #12205, .T. ) ;
#21165 = CARTESIAN_POINT ( 'NONE',  ( -46.55190821232856280, 18.53135734581249139, -8.917361510505369182 ) ) ;
#21166 = ORIENTED_EDGE ( 'NONE', *, *, #34413, .F. ) ;
#21167 = CARTESIAN_POINT ( 'NONE',  ( -0.4166666666666669072, 0.000000000000000000, 10.00000000000000000 ) ) ;
#21168 = CARTESIAN_POINT ( 'NONE',  ( 9.696760411815720460, 2.443938934556958653, 0.000000000000000000 ) ) ;
#21169 = DIRECTION ( 'NONE',  ( -0.000000000000000000, -1.000000000000000000, -0.000000000000000000 ) ) ;
#21170 = CARTESIAN_POINT ( 'NONE',  ( 166.9999999999999716, -164.9999999999999432, -344.0000000000001137 ) ) ;
#21171 = EDGE_CURVE ( 'NONE', #387, #40469, #24538, .T. ) ;
#21172 = DIRECTION ( 'NONE',  ( 0.000000000000000000, 0.000000000000000000, 1.000000000000000000 ) ) ;
#21173 = ORIENTED_EDGE ( 'NONE', *, *, #3266, .F. ) ;
#21174 = CARTESIAN_POINT ( 'NONE',  ( -7.372990760266265653, 0.000000000000000000, 0.000000000000000000 ) ) ;
#21175 = CYLINDRICAL_SURFACE ( 'NONE', #35547, 1.750000000000001554 ) ;
#21176 = LINE ( 'NONE', #39941, #20371 ) ;
#21177 = CARTESIAN_POINT ( 'NONE',  ( 22.93339884797969930, -29.71580813607141636, -3.721387749823079627 ) ) ;
#21178 = ADVANCED_FACE ( 'NONE', ( #923 ), #44488, .T. ) ;
#21179 = ADVANCED_FACE ( 'NONE', ( #20397 ), #16267, .T. ) ;
#21180 = VECTOR ( 'NONE', #18578, 1000.000000000000000 ) ;
#21181 = DIRECTION ( 'NONE',  ( -1.000000000000000000, 0.000000000000000000, 6.938893903907223447E-16 ) ) ;
#21182 = EDGE_CURVE ( 'NONE', #980, #42696, #33396, .T. ) ;
#21183 = CARTESIAN_POINT ( 'NONE',  ( 6.174150299305392053, -50.00000000000000711, 8.807470649214879543 ) ) ;
#21184 = DIRECTION ( 'NONE',  ( 0.000000000000000000, 0.000000000000000000, -1.000000000000000000 ) ) ;
#21185 = EDGE_CURVE ( 'NONE', #18535, #2268, #14865, .T. ) ;
#21186 = CLOSED_SHELL ( 'NONE', ( #33785, #45718, #47504, #3627, #5841, #44016, #46307, #29959, #44168, #5413, #33531, #33127, #34508, #5741, #26187, #2058, #13287, #34707 ) ) ;
#21187 = CARTESIAN_POINT ( 'NONE',  ( -124.9459734468149463, 2.143131898507847836E-16, 165.0000000000000000 ) ) ;
#21188 = EDGE_CURVE ( 'NONE', #9702, #27396, #38634, .T. ) ;
#21189 = ORIENTED_EDGE ( 'NONE', *, *, #34638, .F. ) ;
#21190 = DIRECTION ( 'NONE',  ( -1.000000000000000000, 0.000000000000000000, 0.000000000000000000 ) ) ;
#21191 = CARTESIAN_POINT ( 'NONE',  ( -47.87295225382221275, -14.46560184742400423, -2.408242355805840784 ) ) ;
#21192 = DIRECTION ( 'NONE',  ( 0.000000000000000000, 0.000000000000000000, 1.000000000000000000 ) ) ;
#21193 = LINE ( 'NONE', #28403, #46215 ) ;
#21194 = FACE_OUTER_BOUND ( 'NONE', #13103, .T. ) ;
#21195 = ORIENTED_EDGE ( 'NONE', *, *, #28847, .F. ) ;
#21196 = FACE_OUTER_BOUND ( 'NONE', #38858, .T. ) ;
#21197 = B_SPLINE_SURFACE_WITH_KNOTS ( 'NONE', 3, 3, ( 
 ( #19507, #39287, #549, #23882 ),
 ( #35195, #8493, #11832, #27483 ),
 ( #42602, #24148, #3869, #20282 ),
 ( #19255, #4133, #26965, #19772 ) ),
 .UNSPECIFIED., .F., .F., .F.,
 ( 4, 4 ),
 ( 4, 4 ),
 ( 0.000000000000000000, 1.000000000000000000 ),
 ( 0.000000000000000000, 1.000000000000000000 ),
 .UNSPECIFIED. ) ;
#21198 = ORIENTED_EDGE ( 'NONE', *, *, #22745, .F. ) ;
#21199 = CARTESIAN_POINT ( 'NONE',  ( 1.780432407520001536, 1.041450996408479046, 9.894754715216729224 ) ) ;
#21200 = CYLINDRICAL_SURFACE ( 'NONE', #40229, 1.750000000000008438 ) ;
#21201 = ORIENTED_EDGE ( 'NONE', *, *, #11103, .T. ) ;
#21202 = EDGE_CURVE ( 'NONE', #34395, #34063, #43859, .T. ) ;
#21203 = CARTESIAN_POINT ( 'NONE',  ( -165.6708471809677974, 1.750000000000009548, -160.2068387089191219 ) ) ;
#21204 = DIRECTION ( 'NONE',  ( 0.000000000000000000, 0.000000000000000000, 1.000000000000000000 ) ) ;
#21205 = ORIENTED_EDGE ( 'NONE', *, *, #35919, .T. ) ;
#21206 = ORIENTED_EDGE ( 'NONE', *, *, #40246, .F. ) ;
#21207 = CARTESIAN_POINT ( 'NONE',  ( 210.0000000000000568, 0.000000000000000000, 0.8182875569279768335 ) ) ;
#21208 = CARTESIAN_POINT ( 'NONE',  ( -1.655083081098053466, 7.799304653815004151, 2.264627287779097387E-14 ) ) ;
#21209 = FACE_OUTER_BOUND ( 'NONE', #40731, .T. ) ;
#21210 =( BOUNDED_CURVE ( )  B_SPLINE_CURVE ( 3, ( #22258, #22001, #34317, #41247 ),
 .UNSPECIFIED., .F., .F. ) 
 B_SPLINE_CURVE_WITH_KNOTS ( ( 4, 4 ),
 ( 4.712388980384689674, 6.283185307179586232 ),
 .UNSPECIFIED. ) 
 CURVE ( )  GEOMETRIC_REPRESENTATION_ITEM ( )  RATIONAL_B_SPLINE_CURVE ( ( 1.000000000000000000, 0.8047378541243649375, 0.8047378541243649375, 1.000000000000000000 ) ) 
 REPRESENTATION_ITEM ( '' )  );
#21211 = ORIENTED_EDGE ( 'NONE', *, *, #13583, .T. ) ;
#21212 = VECTOR ( 'NONE', #30856, 1000.000000000000000 ) ;
#21213 = CARTESIAN_POINT ( 'NONE',  ( 114.3291528190321173, -1.749999999999997113, 79.79316129108087807 ) ) ;
#21214 = CARTESIAN_POINT ( 'NONE',  ( -84.94597344681493212, 1.025126265847089435, -40.93171244307204404 ) ) ;
#21215 = CARTESIAN_POINT ( 'NONE',  ( -87.72109971266203843, -1.750000000000010214, -78.15658617722490931 ) ) ;
#21216 = ORIENTED_EDGE ( 'NONE', *, *, #22678, .T. ) ;
#21217 = ORIENTED_EDGE ( 'NONE', *, *, #6826, .F. ) ;
#21218 = ORIENTED_EDGE ( 'NONE', *, *, #26130, .T. ) ;
#21219 = CARTESIAN_POINT ( 'NONE',  ( -88.44597344681494633, 1.025126265847089657, 79.06828755692797017 ) ) ;
#21220 = AXIS2_PLACEMENT_3D ( 'NONE', #15683, #35463, #15949 ) ;
#21221 = VECTOR ( 'NONE', #20214, 1000.000000000000000 ) ;
#21222 = EDGE_CURVE ( 'NONE', #27700, #4361, #29477, .T. ) ;
#21223 =( BOUNDED_CURVE ( )  B_SPLINE_CURVE ( 3, ( #32376, #47974, #39838, #20062 ),
 .UNSPECIFIED., .F., .F. ) 
 B_SPLINE_CURVE_WITH_KNOTS ( ( 4, 4 ),
 ( 3.141592653589793116, 4.712388980384689674 ),
 .UNSPECIFIED. ) 
 CURVE ( )  GEOMETRIC_REPRESENTATION_ITEM ( )  RATIONAL_B_SPLINE_CURVE ( ( 1.000000000000000000, 0.8047378541243649375, 0.8047378541243649375, 1.000000000000000000 ) ) 
 REPRESENTATION_ITEM ( '' )  );
#21224 = DIRECTION ( 'NONE',  ( 0.000000000000000000, 0.000000000000000000, 1.000000000000000000 ) ) ;
#21225 = ORIENTED_EDGE ( 'NONE', *, *, #36562, .F. ) ;
#21226 = AXIS2_PLACEMENT_3D ( 'NONE', #8242, #40296, #39551 ) ;
#21227 = CARTESIAN_POINT ( 'NONE',  ( -44.94597344681493922, 2.143131898507880377E-16, 122.5682875569279702 ) ) ;
#21228 = DIRECTION ( 'NONE',  ( 1.000000000000000000, 0.000000000000000000, 0.000000000000000000 ) ) ;
#21229 = VECTOR ( 'NONE', #37867, 1000.000000000000000 ) ;
#21230 = DIRECTION ( 'NONE',  ( -0.000000000000000000, -1.000000000000000000, -0.000000000000000000 ) ) ;
#21231 = CARTESIAN_POINT ( 'NONE',  ( 40.86389006639091548, 8.513139889764598678, -8.080361901872240793 ) ) ;
#21232 = CARTESIAN_POINT ( 'NONE',  ( -204.9459734468148895, 1.025126265847089657, 42.56828755692799149 ) ) ;
#21233 = DIRECTION ( 'NONE',  ( 0.000000000000000000, -1.000000000000000000, 0.000000000000000000 ) ) ;
#21234 = CARTESIAN_POINT ( 'NONE',  ( -166.6959734468149463, 0.000000000000000000, 165.0000000000000000 ) ) ;
#21235 =( BOUNDED_CURVE ( )  B_SPLINE_CURVE ( 3, ( #46119, #42314, #30784, #38994 ),
 .UNSPECIFIED., .F., .F. ) 
 B_SPLINE_CURVE_WITH_KNOTS ( ( 4, 4 ),
 ( 1.570796326794896558, 3.141592653589793116 ),
 .UNSPECIFIED. ) 
 CURVE ( )  GEOMETRIC_REPRESENTATION_ITEM ( )  RATIONAL_B_SPLINE_CURVE ( ( 1.000000000000000000, 0.8047378541243649375, 0.8047378541243649375, 1.000000000000000000 ) ) 
 REPRESENTATION_ITEM ( '' )  );
#21236 = CARTESIAN_POINT ( 'NONE',  ( 0.3862712429686978033, -1.188820645368937834, -10.00000000000000000 ) ) ;
#21237 = CARTESIAN_POINT ( 'NONE',  ( -4.945973446814917018, 1.025126265847097207, 2.568287556927999926 ) ) ;
#21238 = EDGE_CURVE ( 'NONE', #14475, #16065, #37846, .T. ) ;
#21239 = EDGE_CURVE ( 'NONE', #10859, #14506, #43561, .T. ) ;
#21240 = CARTESIAN_POINT ( 'NONE',  ( 1.011271242968683648, 0.7347315653655930312, -3.333333333333333481 ) ) ;
#21241 = ORIENTED_EDGE ( 'NONE', *, *, #7513, .T. ) ;
#21242 = CARTESIAN_POINT ( 'NONE',  ( -126.6959734468149321, 0.000000000000000000, 165.0000000000000000 ) ) ;
#21243 = ADVANCED_FACE ( 'NONE', ( #2663 ), #40917, .F. ) ;
#21244 = CARTESIAN_POINT ( 'NONE',  ( 169.0000000000000000, 165.0000000000000000, 341.9999999999998863 ) ) ;
#21245 = DIRECTION ( 'NONE',  ( 1.156482317317870492E-16, -1.000000000000000000, 0.000000000000000000 ) ) ;
#21246 = FACE_OUTER_BOUND ( 'NONE', #17485, .T. ) ;
#21247 = EDGE_CURVE ( 'NONE', #4914, #39755, #49569, .T. ) ;
#21248 = AXIS2_PLACEMENT_3D ( 'NONE', #16331, #31748, #12728 ) ;
#21249 = EDGE_CURVE ( 'NONE', #970, #8813, #41158, .T. ) ;
#21250 = VERTEX_POINT ( 'NONE', #41421 ) ;
#21251 = LINE ( 'NONE', #36941, #48564 ) ;
#21252 = CIRCLE ( 'NONE', #49083, 1.750000000000001554 ) ;
#21253 = DIRECTION ( 'NONE',  ( -1.000000000000000000, 0.000000000000000000, 0.000000000000000000 ) ) ;
#21254 = ORIENTED_EDGE ( 'NONE', *, *, #16218, .F. ) ;
#21255 = COLOUR_RGB ( '',0.7921568627450980005, 0.8196078431372548767, 0.9333333333333333481 ) ;
#21256 = CARTESIAN_POINT ( 'NONE',  ( 47.88254548617766204, -14.43607691413525984, -3.760136334089591248 ) ) ;
#21257 = CARTESIAN_POINT ( 'NONE',  ( -126.6959734468149321, 0.000000000000000000, 165.0000000000000000 ) ) ;
#21258 = CARTESIAN_POINT ( 'NONE',  ( -46.69597344681494633, -1.750000000000010214, -39.18171244307202983 ) ) ;
#21259 = ADVANCED_FACE ( 'NONE', ( #30127 ), #37354, .F. ) ;
#21260 = ORIENTED_EDGE ( 'NONE', *, *, #49422, .F. ) ;
#21261 = SURFACE_SIDE_STYLE ('',( #5601 ) ) ;
#21262 = VERTEX_POINT ( 'NONE', #29618 ) ;
#21263 = ORIENTED_EDGE ( 'NONE', *, *, #29896, .F. ) ;
#21264 = FACE_OUTER_BOUND ( 'NONE', #15523, .T. ) ;
#21265 = VECTOR ( 'NONE', #7314, 1000.000000000000000 ) ;
#21266 = ORIENTED_EDGE ( 'NONE', *, *, #41129, .F. ) ;
#21267 = CARTESIAN_POINT ( 'NONE',  ( -1.011271242968688533, 0.7347315653655859258, 10.00000000000000000 ) ) ;
#21268 = ORIENTED_EDGE ( 'NONE', *, *, #8254, .F. ) ;
#21269 = CARTESIAN_POINT ( 'NONE',  ( 14.52758583651987223, 8.922352469211173087, 8.953103998512858652 ) ) ;
#21270 = DIRECTION ( 'NONE',  ( -1.000000000000000000, 0.000000000000000000, 0.000000000000000000 ) ) ;
#21271 = CARTESIAN_POINT ( 'NONE',  ( -5.670847180967843570, -1.750000000000023315, -78.15658617722490931 ) ) ;
#21272 = CARTESIAN_POINT ( 'NONE',  ( 0.3862712429686894766, -1.188820645368940276, 10.00000000000000000 ) ) ;
#21273 = VERTEX_POINT ( 'NONE', #13460 ) ;
#21274 = DIRECTION ( 'NONE',  ( 0.000000000000000000, 0.000000000000000000, 1.000000000000000000 ) ) ;
#21275 = ORIENTED_EDGE ( 'NONE', *, *, #19228, .F. ) ;
#21276 = CARTESIAN_POINT ( 'NONE',  ( -86.69597344681494633, 1.750000000000010214, -39.18171244307202983 ) ) ;
#21277 = LINE ( 'NONE', #29737, #22058 ) ;
#21278 = ORIENTED_EDGE ( 'NONE', *, *, #11709, .T. ) ;
#21279 = EDGE_LOOP ( 'NONE', ( #8144, #20454, #21096, #15674, #42355, #2072 ) ) ;
#21280 = ORIENTED_EDGE ( 'NONE', *, *, #17111, .F. ) ;
#21281 = CARTESIAN_POINT ( 'NONE',  ( -64.99999999999909051, 17.00000000000000000, -24.99999999999999289 ) ) ;
#21282 = CARTESIAN_POINT ( 'NONE',  ( 210.0000000000000568, 0.000000000000000000, -79.18171244307201562 ) ) ;
#21283 = ORIENTED_EDGE ( 'NONE', *, *, #16433, .T. ) ;
#21284 = AXIS2_PLACEMENT_3D ( 'NONE', #9970, #48917, #18417 ) ;
#21285 = ADVANCED_FACE ( 'NONE', ( #21406 ), #49319, .F. ) ;
#21286 = VECTOR ( 'NONE', #47154, 1000.000000000000000 ) ;
#21287 = PLANE ( 'NONE',  #32325 ) ;
#21288 = CARTESIAN_POINT ( 'NONE',  ( 4.641001526964560142, 50.00000000000000711, -8.016098858316199838 ) ) ;
#21289 = CARTESIAN_POINT ( 'NONE',  ( 214.9999999999999432, 164.9999999999999716, 252.0000000000000000 ) ) ;
#21290 = AXIS2_PLACEMENT_3D ( 'NONE', #25290, #6306, #18584 ) ;
#21291 = ORIENTED_EDGE ( 'NONE', *, *, #36236, .T. ) ;
#21292 = DIRECTION ( 'NONE',  ( -1.000000000000000000, 0.000000000000000000, 0.000000000000000000 ) ) ;
#21293 = LINE ( 'NONE', #32607, #29196 ) ;
#21294 = VECTOR ( 'NONE', #10306, 1000.000000000000000 ) ;
#21295 = DIRECTION ( 'NONE',  ( 0.000000000000000000, 1.000000000000000000, 0.000000000000000000 ) ) ;
#21296 = EDGE_LOOP ( 'NONE', ( #21851, #22119, #13518, #18774 ) ) ;
#21297 = ORIENTED_EDGE ( 'NONE', *, *, #41831, .F. ) ;
#21298 = SHAPE_DEFINITION_REPRESENTATION ( #33939, #8438 ) ;
#21299 = CARTESIAN_POINT ( 'NONE',  ( -14.99999999999845812, 16.00000000000000000, 35.00000000000000000 ) ) ;
#21300 = DIRECTION ( 'NONE',  ( 0.000000000000000000, -0.000000000000000000, -1.000000000000000000 ) ) ;
#21301 = EDGE_CURVE ( 'NONE', #43558, #42084, #21925, .T. ) ;
#21302 = CARTESIAN_POINT ( 'NONE',  ( 1.290940757014967355, -0.08848829412275825701, 9.947020512645421420 ) ) ;
#21303 = CARTESIAN_POINT ( 'NONE',  ( -33.43156050989129824, 4.370686678976795747, 8.807470649214879543 ) ) ;
#21304 = VERTEX_POINT ( 'NONE', #29872 ) ;
#21305 = CARTESIAN_POINT ( 'NONE',  ( 194.3291528190321742, -1.750000000000009548, 41.84341382277508359 ) ) ;
#21306 = CARTESIAN_POINT ( 'NONE',  ( -44.99506233596264337, -23.32283626942287214, 7.455576670931136185 ) ) ;
#21307 = DIRECTION ( 'NONE',  ( -0.000000000000000000, -0.000000000000000000, -1.000000000000000000 ) ) ;
#21308 = PLANE ( 'NONE',  #50329 ) ;
#21309 = LINE ( 'NONE', #5150, #34497 ) ;
#21310 = EDGE_CURVE ( 'NONE', #2541, #38591, #6283, .T. ) ;
#21311 = ADVANCED_FACE ( 'NONE', ( #48819 ), #9863, .T. ) ;
#21312 = EDGE_LOOP ( 'NONE', ( #38392, #8073, #26626, #17671 ) ) ;
#21313 = CARTESIAN_POINT ( 'NONE',  ( 360.0000000000000000, 169.0000000000001990, -344.0000000000002842 ) ) ;
#21314 = ORIENTED_EDGE ( 'NONE', *, *, #37138, .T. ) ;
#21315 = CARTESIAN_POINT ( 'NONE',  ( 1.011271242968677653, 0.7347315653656002477, 10.00000000000000000 ) ) ;
#21316 = ORIENTED_EDGE ( 'NONE', *, *, #22169, .T. ) ;
#21317 = EDGE_CURVE ( 'NONE', #22263, #11094, #2176, .T. ) ;
#21318 = FACE_OUTER_BOUND ( 'NONE', #17627, .T. ) ;
#21319 = DIRECTION ( 'NONE',  ( 1.000000000000000000, -0.000000000000000000, 0.000000000000000000 ) ) ;
#21320 = CARTESIAN_POINT ( 'NONE',  ( -4.945973446814903696, 2.143131898507912917E-16, -80.93171244307204404 ) ) ;
#21321 = VECTOR ( 'NONE', #28412, 1000.000000000000000 ) ;
#21322 = ORIENTED_EDGE ( 'NONE', *, *, #45119, .T. ) ;
#21323 = AXIS2_PLACEMENT_3D ( 'NONE', #45708, #19043, #3653 ) ;
#21324 = CIRCLE ( 'NONE', #17228, 4.000000000000003553 ) ;
#21325 = CARTESIAN_POINT ( 'NONE',  ( -86.69597344681494633, -1.750000000000009992, 0.8182875569279768335 ) ) ;
#21326 = ORIENTED_EDGE ( 'NONE', *, *, #18051, .T. ) ;
#21327 = DIRECTION ( 'NONE',  ( -1.000000000000000000, -0.000000000000000000, -0.000000000000000000 ) ) ;
#21328 = FACE_OUTER_BOUND ( 'NONE', #4617, .T. ) ;
#21329 = LINE ( 'NONE', #37513, #30318 ) ;
#21330 = DIRECTION ( 'NONE',  ( -1.000000000000000000, -0.000000000000000000, -0.000000000000000000 ) ) ;
#21331 = VECTOR ( 'NONE', #4570, 1000.000000000000000 ) ;
#21332 = CARTESIAN_POINT ( 'NONE',  ( 16.02661358026014327, 4.530191650547718218, -9.683996418299976483 ) ) ;
#21333 = VERTEX_POINT ( 'NONE', #14980 ) ;
#21334 = ORIENTED_EDGE ( 'NONE', *, *, #40382, .F. ) ;
#21335 = VERTEX_POINT ( 'NONE', #23449 ) ;
#21336 = DIRECTION ( 'NONE',  ( -0.000000000000000000, 0.8962124318248270161, 0.4436251537532894806 ) ) ;
#21337 = CARTESIAN_POINT ( 'NONE',  ( 0.1425549192113746144, -1.238581250503543618, 9.981352469109934233 ) ) ;
#21338 = ORIENTED_EDGE ( 'NONE', *, *, #40856, .F. ) ;
#21339 = PLANE ( 'NONE',  #45036 ) ;
#21340 = DIRECTION ( 'NONE',  ( -1.000000000000000000, 0.000000000000000000, 0.000000000000000000 ) ) ;
#21341 = ORIENTED_EDGE ( 'NONE', *, *, #20, .T. ) ;
#21342 = CARTESIAN_POINT ( 'NONE',  ( 8.277096487746778308, -33.14818118907697198, 7.455576670931136185 ) ) ;
#21343 = EDGE_CURVE ( 'NONE', #49858, #50040, #47168, .T. ) ;
#21344 = CARTESIAN_POINT ( 'NONE',  ( -31.28977333267361871, 11.25592690310926969, -2.408242355805840784 ) ) ;
#21345 = PLANE ( 'NONE',  #21645 ) ;
#21346 = LINE ( 'NONE', #10316, #5077 ) ;
#21347 = VERTEX_POINT ( 'NONE', #50331 ) ;
#21348 = ORIENTED_EDGE ( 'NONE', *, *, #19327, .F. ) ;
#21349 = EDGE_LOOP ( 'NONE', ( #31839, #28534, #30799, #11116 ) ) ;
#21350 = CARTESIAN_POINT ( 'NONE',  ( -168.4459734468149747, -1.025126265847089879, -117.4317124430720156 ) ) ;
#21351 = CARTESIAN_POINT ( 'NONE',  ( 370.7621192902014968, -98.56198943095992604, -17.65743994998275213 ) ) ;
#21352 = FACE_OUTER_BOUND ( 'NONE', #10698, .T. ) ;
#21353 = CARTESIAN_POINT ( 'NONE',  ( 2.538055338523177440, 33.28424297489108596, -9.367992836599954742 ) ) ;
#21354 = EDGE_LOOP ( 'NONE', ( #41513, #25081, #28028, #49908 ) ) ;
#21355 = CARTESIAN_POINT ( 'NONE',  ( 4.204997580903516941, -7.388441598285492518, 225.0000000000000000 ) ) ;
#21356 = VERTEX_POINT ( 'NONE', #30384 ) ;
#21357 = CARTESIAN_POINT ( 'NONE',  ( -14.99999999999812594, 17.00000000000000000, 65.00000000000000000 ) ) ;
#21358 = DIRECTION ( 'NONE',  ( -1.000000000000000000, -0.000000000000000000, -0.000000000000000000 ) ) ;
#21359 = CARTESIAN_POINT ( 'NONE',  ( 0.000000000000000000, 0.000000000000000000, 900.0000000000000000 ) ) ;
#21360 = VECTOR ( 'NONE', #23422, 1000.000000000000000 ) ;
#21361 = DIRECTION ( 'NONE',  ( -1.000000000000000000, 0.000000000000000000, 0.000000000000000000 ) ) ;
#21362 = LINE ( 'NONE', #10335, #2820 ) ;
#21363 = DIRECTION ( 'NONE',  ( 1.000000000000000000, 0.000000000000000000, 1.612977847700450206E-50 ) ) ;
#21364 = ORIENTED_EDGE ( 'NONE', *, *, #35625, .T. ) ;
#21365 = DIRECTION ( 'NONE',  ( 1.860490536778032451E-50, 0.000000000000000000, -1.000000000000000000 ) ) ;
#21367 = VECTOR ( 'NONE', #1820, 1000.000000000000000 ) ;
#21366 = CYLINDRICAL_SURFACE ( 'NONE', #711, 4.000000000000003553 ) ;
#21368 = DIRECTION ( 'NONE',  ( 0.000000000000000000, 0.000000000000000000, -1.000000000000000000 ) ) ;
#21369 = DIRECTION ( 'NONE',  ( -5.551115123125782702E-17, 0.7071067811865477948, 0.7071067811865473507 ) ) ;
#21370 = ORIENTED_EDGE ( 'NONE', *, *, #26542, .T. ) ;
#21371 = CARTESIAN_POINT ( 'NONE',  ( 181.0000000000000000, 175.0000000000000284, -356.0000000000001705 ) ) ;
#21372 = ORIENTED_EDGE ( 'NONE', *, *, #29595, .T. ) ;
#21373 = EDGE_CURVE ( 'NONE', #36910, #12217, #34513, .T. ) ;
#21374 = FACE_OUTER_BOUND ( 'NONE', #10166, .T. ) ;
#21375 = CARTESIAN_POINT ( 'NONE',  ( -206.6959734468149463, 0.000000000000000000, -165.0000000000000000 ) ) ;
#21376 =( BOUNDED_CURVE ( )  B_SPLINE_CURVE ( 3, ( #5544, #21696, #25810, #9649 ),
 .UNSPECIFIED., .F., .F. ) 
 B_SPLINE_CURVE_WITH_KNOTS ( ( 4, 4 ),
 ( 3.141592653589793116, 4.712388980384689674 ),
 .UNSPECIFIED. ) 
 CURVE ( )  GEOMETRIC_REPRESENTATION_ITEM ( )  RATIONAL_B_SPLINE_CURVE ( ( 1.000000000000000000, 0.8047378541243649375, 0.8047378541243649375, 1.000000000000000000 ) ) 
 REPRESENTATION_ITEM ( '' )  );
#21377 = CARTESIAN_POINT ( 'NONE',  ( 181.0000000000000000, -272.4999999999999432, -339.9999999999998863 ) ) ;
#21378 = VERTEX_POINT ( 'NONE', #30639 ) ;
#21379 = ORIENTED_EDGE ( 'NONE', *, *, #16776, .F. ) ;
#21380 = CARTESIAN_POINT ( 'NONE',  ( 185.0000000000000000, -272.5000000000000000, -110.9999999999999005 ) ) ;
#21381 = CARTESIAN_POINT ( 'NONE',  ( 10.69268279052430159, 12.77266927778462779, -2.870787844569587133 ) ) ;
#21382 = CARTESIAN_POINT ( 'NONE',  ( -64.99999999999971578, 16.00000000000000000, -84.99999999999998579 ) ) ;
#21383 = CARTESIAN_POINT ( 'NONE',  ( -164.9459734468149463, -1.025126265847089435, 82.56828755692798438 ) ) ;
#21384 = VERTEX_POINT ( 'NONE', #10871 ) ;
#21385 = ORIENTED_EDGE ( 'NONE', *, *, #12343, .T. ) ;
#21386 = CARTESIAN_POINT ( 'NONE',  ( 152.2789002873379900, -1.750000000000010214, -118.1565861772249519 ) ) ;
#21387 = EDGE_CURVE ( 'NONE', #32533, #43849, #38604, .T. ) ;
#21388 = CARTESIAN_POINT ( 'NONE',  ( -128.4459734468149179, 0.000000000000000000, -157.4317124430720582 ) ) ;
#21389 = AXIS2_PLACEMENT_3D ( 'NONE', #9349, #20641, #32700 ) ;
#21390 = ORIENTED_EDGE ( 'NONE', *, *, #11745, .F. ) ;
#21391 = VERTEX_POINT ( 'NONE', #46243 ) ;
#21392 = CARTESIAN_POINT ( 'NONE',  ( 168.9999999999999716, -268.5000000000000000, -114.9999999999999147 ) ) ;
#21393 = CARTESIAN_POINT ( 'NONE',  ( -204.9459734468149463, 2.143131898507880377E-16, 79.06828755692797017 ) ) ;
#21394 = CARTESIAN_POINT ( 'NONE',  ( 35.05402655318504657, 2.143131898507880377E-16, 159.0682875569279702 ) ) ;
#21395 = MANIFOLD_SOLID_BREP ( 'Square tube 20 X 20 X 2(1)[12]', #48174 ) ;
#21396 = DIRECTION ( 'NONE',  ( -1.000000000000000000, 0.000000000000000000, 0.000000000000000000 ) ) ;
#21397 =( REPRESENTATION_RELATIONSHIP ('NONE','NONE', #45699, #15926 ) REPRESENTATION_RELATIONSHIP_WITH_TRANSFORMATION ( #36216 )SHAPE_REPRESENTATION_RELATIONSHIP( ) );
#21398 = EDGE_LOOP ( 'NONE', ( #46540, #15511, #28830, #27435 ) ) ;
#21399 = VERTEX_POINT ( 'NONE', #2903 ) ;
#21400 = VERTEX_POINT ( 'NONE', #3680 ) ;
#21401 = EDGE_CURVE ( 'NONE', #12244, #7115, #19069, .T. ) ;
#21402 = CARTESIAN_POINT ( 'NONE',  ( 339.9999999999998863, -164.9999999999999432, 343.9999999999997726 ) ) ;
#21403 = DIRECTION ( 'NONE',  ( 1.000000000000000000, 1.156482317317871478E-16, 0.000000000000000000 ) ) ;
#21404 = ORIENTED_EDGE ( 'NONE', *, *, #1218, .F. ) ;
#21405 = VERTEX_POINT ( 'NONE', #14723 ) ;
#21406 = FACE_OUTER_BOUND ( 'NONE', #25443, .T. ) ;
#21407 = CARTESIAN_POINT ( 'NONE',  ( -208.4459734468148611, 1.025126265847088991, -157.4317124430720582 ) ) ;
#21408 = VERTEX_POINT ( 'NONE', #50588 ) ;
#21409 = ORIENTED_EDGE ( 'NONE', *, *, #46519, .F. ) ;
#21410 = CARTESIAN_POINT ( 'NONE',  ( -168.4459734468149463, 0.000000000000000000, 165.0000000000000000 ) ) ;
#21411 = CARTESIAN_POINT ( 'NONE',  ( -6.695973446814940111, 0.000000000000000000, 165.0000000000000000 ) ) ;
#21412 = ORIENTED_EDGE ( 'NONE', *, *, #43149, .T. ) ;
#21413 = CARTESIAN_POINT ( 'NONE',  ( 341.9999999999999432, -174.9999999999999432, 343.9999999999998295 ) ) ;
#21414 = CARTESIAN_POINT ( 'NONE',  ( 130.0000000000012221, 17.00000000000000000, 30.00000000000000000 ) ) ;
#21415 = CARTESIAN_POINT ( 'NONE',  ( 114.3291528190321173, -1.749999999999997113, -80.20683870891909351 ) ) ;
#21416 = DIRECTION ( 'NONE',  ( 0.000000000000000000, 1.000000000000000000, 1.544785076050074834E-48 ) ) ;
#21417 = CARTESIAN_POINT ( 'NONE',  ( 29.12062022658201244, -29.99172060348948321, 8.846626183609803462 ) ) ;
#21418 = VERTEX_POINT ( 'NONE', #30905 ) ;
#21419 = CARTESIAN_POINT ( 'NONE',  ( 10.01251772323701772, 8.486842105263161073, 18.46084505325461578 ) ) ;
#21420 = VECTOR ( 'NONE', #22414, 999.9999999999998863 ) ;
#21421 = CARTESIAN_POINT ( 'NONE',  ( 210.0000000000000568, 0.000000000000000000, 120.8182875569279702 ) ) ;
#21422 = LINE ( 'NONE', #47017, #35130 ) ;
#21423 = DIRECTION ( 'NONE',  ( 0.000000000000000000, -2.969158215481698263E-48, 1.000000000000000000 ) ) ;
#21424 = EDGE_CURVE ( 'NONE', #11094, #44375, #49063, .T. ) ;
#21425 = DIRECTION ( 'NONE',  ( -0.000000000000000000, -0.000000000000000000, -1.000000000000000000 ) ) ;
#21427 = B_SPLINE_CURVE_WITH_KNOTS ( 'NONE', 3,
 ( #3591, #31323, #15914, #22839 ),
 .UNSPECIFIED., .F., .F.,
 ( 4, 4 ),
 ( 5.210275057513392971E-05, 0.0002352737929598119979 ),
 .UNSPECIFIED. ) ;
#21426 = CARTESIAN_POINT ( 'NONE',  ( 192.2789002873380184, -1.750000000000010214, -118.1565861772249519 ) ) ;
#21428 = CARTESIAN_POINT ( 'NONE',  ( 33.30402655318503946, -1.750000000000010658, 120.8182875569279702 ) ) ;
#21429 = EDGE_CURVE ( 'NONE', #5197, #44630, #47278, .T. ) ;
#21430 = CYLINDRICAL_SURFACE ( 'NONE', #15581, 10.00000000000000000 ) ;
#21431 = VECTOR ( 'NONE', #26496, 1000.000000000000000 ) ;
#21432 = CARTESIAN_POINT ( 'NONE',  ( -167.4999999999999432, -102.5000000000000142, -10.00000000000000000 ) ) ;
#21433 = EDGE_CURVE ( 'NONE', #48435, #42421, #3538, .T. ) ;
#21434 = ORIENTED_EDGE ( 'NONE', *, *, #6406, .T. ) ;
#21435 = EDGE_CURVE ( 'NONE', #29552, #46590, #7034, .T. ) ;
#21436 = CARTESIAN_POINT ( 'NONE',  ( -119.9999999999984652, 17.00000000000000000, 60.00000000000000000 ) ) ;
#21437 = PLANE ( 'NONE',  #39369 ) ;
#21438 = CARTESIAN_POINT ( 'NONE',  ( -8.445973446814976526, 0.000000000000000000, -117.4317124430720156 ) ) ;
#21439 = CARTESIAN_POINT ( 'NONE',  ( -14.99999999999970868, 16.00000000000000000, -84.99999999999998579 ) ) ;
#21440 = CARTESIAN_POINT ( 'NONE',  ( 33.30402655318503946, 1.750000000000010214, 40.81828755692798438 ) ) ;
#21441 = ORIENTED_EDGE ( 'NONE', *, *, #33152, .F. ) ;
#21442 = CARTESIAN_POINT ( 'NONE',  ( -215.0000000000000568, 164.9999999999999716, 500.0000000000000000 ) ) ;
#21443 = ORIENTED_EDGE ( 'NONE', *, *, #43046, .T. ) ;
#21444 = CARTESIAN_POINT ( 'NONE',  ( 357.9999999999998863, -182.1715728752539860, -357.1715728752541281 ) ) ;
#21445 = LINE ( 'NONE', #9654, #32037 ) ;
#21446 = ORIENTED_EDGE ( 'NONE', *, *, #8974, .T. ) ;
#21447 = CARTESIAN_POINT ( 'NONE',  ( -13.59579750444763668, 10.60877755095910935, 8.727788335465566760 ) ) ;
#21448 = FACE_OUTER_BOUND ( 'NONE', #39101, .T. ) ;
#21449 =( BOUNDED_CURVE ( )  B_SPLINE_CURVE ( 3, ( #1890, #45454, #24741, #5727 ),
 .UNSPECIFIED., .F., .F. ) 
 B_SPLINE_CURVE_WITH_KNOTS ( ( 4, 4 ),
 ( 1.570796326794896558, 3.141592653589793116 ),
 .UNSPECIFIED. ) 
 CURVE ( )  GEOMETRIC_REPRESENTATION_ITEM ( )  RATIONAL_B_SPLINE_CURVE ( ( 1.000000000000000000, 0.8047378541243649375, 0.8047378541243649375, 1.000000000000000000 ) ) 
 REPRESENTATION_ITEM ( '' )  );
#21450 = ORIENTED_EDGE ( 'NONE', *, *, #11410, .F. ) ;
#21451 = ORIENTED_EDGE ( 'NONE', *, *, #20893, .T. ) ;
#21452 = VECTOR ( 'NONE', #38980, 1000.000000000000000 ) ;
#21453 = ADVANCED_FACE ( 'NONE', ( #103 ), #15737, .F. ) ;
#21454 = EDGE_CURVE ( 'NONE', #3211, #32080, #20092, .T. ) ;
#21455 = DIRECTION ( 'NONE',  ( -1.000000000000000000, -0.000000000000000000, -0.000000000000000000 ) ) ;
#21456 = CARTESIAN_POINT ( 'NONE',  ( -86.69597344681494633, -1.750000000000009992, 0.8182875569279768335 ) ) ;
#21457 = DIRECTION ( 'NONE',  ( 0.000000000000000000, 0.000000000000000000, -1.000000000000000000 ) ) ;
#21458 = EDGE_CURVE ( 'NONE', #42814, #2953, #45481, .T. ) ;
#21459 = ORIENTED_EDGE ( 'NONE', *, *, #39950, .T. ) ;
#21460 = EDGE_CURVE ( 'NONE', #7318, #24424, #26182, .T. ) ;
#21461 = CARTESIAN_POINT ( 'NONE',  ( 135.0000000000019043, 17.00000000000000000, 65.00000000000000000 ) ) ;
#21462 = AXIS2_PLACEMENT_3D ( 'NONE', #39130, #46757, #3953 ) ;
#21463 = DIRECTION ( 'NONE',  ( 1.000000000000000000, -4.758098676964957447E-16, 2.958228394578795584E-31 ) ) ;
#21464 = PRESENTATION_STYLE_ASSIGNMENT (( #25324 ) ) ;
#21465 = ORIENTED_EDGE ( 'NONE', *, *, #26928, .T. ) ;
#21466 = VERTEX_POINT ( 'NONE', #27557 ) ;
#21467 = EDGE_LOOP ( 'NONE', ( #3663, #26686, #15654, #3932, #7922 ) ) ;
#21468 = DIRECTION ( 'NONE',  ( -0.000000000000000000, -1.000000000000000000, -0.000000000000000000 ) ) ;
#21469 = EDGE_CURVE ( 'NONE', #19127, #10318, #23698, .T. ) ;
#21470 = ADVANCED_FACE ( 'NONE', ( #47255 ), #4198, .F. ) ;
#21471 = CARTESIAN_POINT ( 'NONE',  ( 342.8284271247460993, -183.0000000000001137, -358.0000000000003411 ) ) ;
#21472 = EDGE_LOOP ( 'NONE', ( #49867, #20522, #29845, #4125, #17579 ) ) ;
#21473 = CARTESIAN_POINT ( 'NONE',  ( -14.99999999999970868, 17.00000000000000000, -84.99999999999998579 ) ) ;
#21474 = CARTESIAN_POINT ( 'NONE',  ( 0.000000000000000000, -165.1999999999999602, -340.2000000000001592 ) ) ;
#21475 = DIRECTION ( 'NONE',  ( -0.7233555441435720601, -0.6904757466825006684, 0.000000000000000000 ) ) ;
#21476 = DIRECTION ( 'NONE',  ( -1.000000000000000000, 0.000000000000000000, 0.000000000000000000 ) ) ;
#21477 = MANIFOLD_SOLID_BREP ( 'Square tube 20 X 20 X 2(1)[16]', #50667 ) ;
#21478 = FACE_OUTER_BOUND ( 'NONE', #14759, .T. ) ;
#21479 = CARTESIAN_POINT ( 'NONE',  ( -48.44597344681495343, 0.000000000000000000, -0.9317124430720247208 ) ) ;
#21480 = FACE_OUTER_BOUND ( 'NONE', #36933, .T. ) ;
#21481 = AXIS2_PLACEMENT_3D ( 'NONE', #38080, #30371, #18797 ) ;
#21482 = DIRECTION ( 'NONE',  ( 0.000000000000000000, 0.000000000000000000, -1.000000000000000000 ) ) ;
#21483 = PLANE ( 'NONE',  #3115 ) ;
#21484 = EDGE_CURVE ( 'NONE', #30864, #22009, #31440, .T. ) ;
#21485 = CARTESIAN_POINT ( 'NONE',  ( 16.69947034530964913, -2.312583065866261389, 2.590526750877053086 ) ) ;
#21486 = EDGE_CURVE ( 'NONE', #4602, #10114, #16003, .T. ) ;
#21487 = ADVANCED_FACE ( 'NONE', ( #8810 ), #27799, .T. ) ;
#21488 = CARTESIAN_POINT ( 'NONE',  ( 169.0000000000000000, -174.9999999999999716, -95.00000000000014211 ) ) ;
#21489 = CIRCLE ( 'NONE', #25603, 1.750000000000001554 ) ;
#21490 = ORIENTED_EDGE ( 'NONE', *, *, #40312, .F. ) ;
#21491 = PLANE ( 'NONE',  #41732 ) ;
#21492 = VECTOR ( 'NONE', #47883, 1000.000000000000000 ) ;
#21493 = CARTESIAN_POINT ( 'NONE',  ( -29.18392875402943432, -17.44843138996582965, 7.906207997025717304 ) ) ;
#21494 = ORIENTED_EDGE ( 'NONE', *, *, #113, .F. ) ;
#21495 = DIRECTION ( 'NONE',  ( -0.000000000000000000, -0.000000000000000000, -1.000000000000000000 ) ) ;
#21496 = VECTOR ( 'NONE', #647, 1000.000000000000000 ) ;
#21497 = DIRECTION ( 'NONE',  ( -0.000000000000000000, -0.000000000000000000, -1.000000000000000000 ) ) ;
#21498 = VERTEX_POINT ( 'NONE', #32156 ) ;
#21499 = DIRECTION ( 'NONE',  ( 1.000000000000000000, 0.000000000000000000, 0.000000000000000000 ) ) ;
#21501 = EDGE_CURVE ( 'NONE', #48877, #25305, #3237, .T. ) ;
#21500 = CARTESIAN_POINT ( 'NONE',  ( 350.0000000000000000, -184.9999999999999716, -356.0000000000002274 ) ) ;
#21502 = DIRECTION ( 'NONE',  ( -1.000000000000000000, 0.000000000000000000, -0.000000000000000000 ) ) ;
#21503 = VERTEX_POINT ( 'NONE', #4448 ) ;
#21504 = DIRECTION ( 'NONE',  ( -0.000000000000000000, -1.000000000000000000, -0.000000000000000000 ) ) ;
#21505 = B_SPLINE_SURFACE_WITH_KNOTS ( 'NONE', 3, 3, ( 
 ( #3244, #14806, #42501, #19669 ),
 ( #30202, #22758, #18643, #46574 ),
 ( #15063, #30726, #34315, #45813 ),
 ( #38185, #30461, #7889, #3494 ) ),
 .UNSPECIFIED., .F., .F., .F.,
 ( 4, 4 ),
 ( 4, 4 ),
 ( 0.000000000000000000, 1.000000000000000000 ),
 ( 0.000000000000000000, 1.000000000000000000 ),
 .UNSPECIFIED. ) ;
#21506 = EDGE_LOOP ( 'NONE', ( #40574, #191, #3848, #20795, #28641, #2804 ) ) ;
#21507 = ORIENTED_EDGE ( 'NONE', *, *, #30899, .T. ) ;
#21508 = DIRECTION ( 'NONE',  ( -1.586032892321652236E-16, -1.000000000000000000, -6.853681917100419162E-49 ) ) ;
#21509 =( BOUNDED_CURVE ( )  B_SPLINE_CURVE ( 3, ( #17588, #2197, #41180, #2687 ),
 .UNSPECIFIED., .F., .F. ) 
 B_SPLINE_CURVE_WITH_KNOTS ( ( 4, 4 ),
 ( 1.570796326794896558, 3.141592653589793116 ),
 .UNSPECIFIED. ) 
 CURVE ( )  GEOMETRIC_REPRESENTATION_ITEM ( )  RATIONAL_B_SPLINE_CURVE ( ( 1.000000000000000000, 0.8047378541243649375, 0.8047378541243649375, 1.000000000000000000 ) ) 
 REPRESENTATION_ITEM ( '' )  );
#21510 = ORIENTED_EDGE ( 'NONE', *, *, #24041, .F. ) ;
#21511 = CARTESIAN_POINT ( 'NONE',  ( 135.0000000000021600, 16.00000000000000000, 95.00000000000000000 ) ) ;
#21512 = CARTESIAN_POINT ( 'NONE',  ( -87.72109971266203843, 1.750000000000009548, 121.8434138227750623 ) ) ;
#21513 = EDGE_CURVE ( 'NONE', #17122, #43110, #16753, .T. ) ;
#21514 = VERTEX_POINT ( 'NONE', #33671 ) ;
#21515 = FACE_OUTER_BOUND ( 'NONE', #44925, .T. ) ;
#21516 = CARTESIAN_POINT ( 'NONE',  ( 342.0000000000000000, 169.0000000000000000, 343.9999999999998863 ) ) ;
#21517 = CARTESIAN_POINT ( 'NONE',  ( -352.5903097982607051, 2.688010569040066411, 225.2259797391364771 ) ) ;
#21518 =( BOUNDED_CURVE ( )  B_SPLINE_CURVE ( 3, ( #28583, #6256, #36308, #24751 ),
 .UNSPECIFIED., .F., .F. ) 
 B_SPLINE_CURVE_WITH_KNOTS ( ( 4, 4 ),
 ( 1.570796326794896558, 3.141592653589793116 ),
 .UNSPECIFIED. ) 
 CURVE ( )  GEOMETRIC_REPRESENTATION_ITEM ( )  RATIONAL_B_SPLINE_CURVE ( ( 1.000000000000000000, 0.8047378541243649375, 0.8047378541243649375, 1.000000000000000000 ) ) 
 REPRESENTATION_ITEM ( '' )  );
#21519 = CIRCLE ( 'NONE', #19061, 3.750000000000000000 ) ;
#21520 = DIRECTION ( 'NONE',  ( 0.000000000000000000, 0.000000000000000000, 1.000000000000000000 ) ) ;
#21521 = ORIENTED_EDGE ( 'NONE', *, *, #48527, .F. ) ;
#21522 = LINE ( 'NONE', #20519, #44414 ) ;
#21523 = ADVANCED_FACE ( 'NONE', ( #21604, #14144 ), #22114, .F. ) ;
#21524 = EDGE_LOOP ( 'NONE', ( #22930, #49173, #14758, #27943 ) ) ;
#21525 = EDGE_CURVE ( 'NONE', #16093, #6443, #38183, .T. ) ;
#21526 = DIRECTION ( 'NONE',  ( 0.000000000000000000, 0.000000000000000000, -1.000000000000000000 ) ) ;
#21527 = DIRECTION ( 'NONE',  ( -1.000000000000000000, -0.000000000000000000, -0.000000000000000000 ) ) ;
#21528 = ORIENTED_EDGE ( 'NONE', *, *, #47704, .T. ) ;
#21529 = VERTEX_POINT ( 'NONE', #17508 ) ;
#21530 = ORIENTED_EDGE ( 'NONE', *, *, #19620, .F. ) ;
#21531 = CARTESIAN_POINT ( 'NONE',  ( -6.695973446814940111, 1.750000000000023315, -159.1817124430720298 ) ) ;
#21532 = EDGE_CURVE ( 'NONE', #22974, #12746, #48508, .T. ) ;
#21533 = ORIENTED_EDGE ( 'NONE', *, *, #49351, .F. ) ;
#21534 = ADVANCED_FACE ( 'NONE', ( #45426 ), #41363, .F. ) ;
#21535 = LINE ( 'NONE', #12834, #28218 ) ;
#21536 = FACE_OUTER_BOUND ( 'NONE', #6694, .T. ) ;
#21537 = EDGE_CURVE ( 'NONE', #16851, #18292, #17259, .T. ) ;
#21538 = DIRECTION ( 'NONE',  ( 1.000000000000000000, 0.000000000000000000, 0.000000000000000000 ) ) ;
#21539 = CARTESIAN_POINT ( 'NONE',  ( 0.000000000000000000, 0.000000000000000000, 10.00000000000000000 ) ) ;
#21540 = CIRCLE ( 'NONE', #13333, 0.5000000000000004441 ) ;
#21541 = ORIENTED_EDGE ( 'NONE', *, *, #13026, .F. ) ;
#21542 = DIRECTION ( 'NONE',  ( 1.000000000000000000, 0.000000000000000000, -0.000000000000000000 ) ) ;
#21543 = CARTESIAN_POINT ( 'NONE',  ( 75.05402655318509630, 2.143131898507880377E-16, 165.0000000000000000 ) ) ;
#21544 = ADVANCED_FACE ( 'NONE', ( #48257 ), #32661, .F. ) ;
#21545 = CARTESIAN_POINT ( 'NONE',  ( -14.29087950072019098, -9.652079258044555132, 8.727788335465566760 ) ) ;
#21546 = ADVANCED_BREP_SHAPE_REPRESENTATION ( '', ( #5361, #45486 ), #38147 ) ;
#21547 = ORIENTED_EDGE ( 'NONE', *, *, #23304, .F. ) ;
#21548 = ITEM_DEFINED_TRANSFORMATION ( 'NONE', 'NONE', #8659,  #45486 ) ;
#21549 = PLANE ( 'NONE',  #32294 ) ;
#21550 = CARTESIAN_POINT ( 'NONE',  ( 18.69789054174343690, -27.49790346457731616, -2.408242355805840784 ) ) ;
#21551 = CARTESIAN_POINT ( 'NONE',  ( -9.260964247899874380, 13.84230907185616744, -9.683996418299976483 ) ) ;
#21552 = CARTESIAN_POINT ( 'NONE',  ( -48.34672127938071640, 13.00749071703899773, 3.199614146704519602 ) ) ;
#21553 = ORIENTED_EDGE ( 'NONE', *, *, #30935, .T. ) ;
#21554 = CARTESIAN_POINT ( 'NONE',  ( 14.49999999999999822, 12.87566193687862715, -19.86060803177194956 ) ) ;
#21555 = DIRECTION ( 'NONE',  ( -1.000000000000000000, -0.000000000000000000, -0.000000000000000000 ) ) ;
#21556 = CARTESIAN_POINT ( 'NONE',  ( 360.0000000000001137, 171.9999999999998295, 3.000000000000003109 ) ) ;
#21557 = DIRECTION ( 'NONE',  ( 1.000000000000000000, -4.996003610813203446E-16, 1.033975765691284226E-24 ) ) ;
#21558 = DIRECTION ( 'NONE',  ( 1.000000000000000000, 0.000000000000000000, 0.000000000000000000 ) ) ;
#21559 = ORIENTED_EDGE ( 'NONE', *, *, #1371, .T. ) ;
#21560 = DIRECTION ( 'NONE',  ( -1.000000000000000000, 0.000000000000000000, 0.000000000000000000 ) ) ;
#21561 = EDGE_LOOP ( 'NONE', ( #20786, #44675, #27536, #47035 ) ) ;
#21562 = DIRECTION ( 'NONE',  ( 0.000000000000000000, 0.000000000000000000, -1.000000000000000000 ) ) ;
#21563 = AXIS2_PLACEMENT_3D ( 'NONE', #39200, #31499, #43527 ) ;
#21564 = ORIENTED_EDGE ( 'NONE', *, *, #20871, .T. ) ;
#21565 = CARTESIAN_POINT ( 'NONE',  ( -86.69597344681494633, 1.750000000000010658, 120.8182875569279702 ) ) ;
#21566 = VECTOR ( 'NONE', #34254, 1000.000000000000000 ) ;
#21567 = CARTESIAN_POINT ( 'NONE',  ( 356.0000000000001137, 165.0000000000000000, 339.9999999999998295 ) ) ;
#21568 = CARTESIAN_POINT ( 'NONE',  ( -164.9459734468149463, -1.025126265847089435, 162.5682875569279133 ) ) ;
#21569 = VERTEX_POINT ( 'NONE', #41612 ) ;
#21570 = ADVANCED_FACE ( 'NONE', ( #40614 ), #38782, .T. ) ;
#21571 = CARTESIAN_POINT ( 'NONE',  ( -215.0000000000000568, 164.9999999999999716, 352.0000000000000000 ) ) ;
#21572 = AXIS2_PLACEMENT_3D ( 'NONE', #26675, #22561, #3057 ) ;
#21573 = ORIENTED_EDGE ( 'NONE', *, *, #20505, .F. ) ;
#21574 = DIRECTION ( 'NONE',  ( 1.000000000000000000, 0.000000000000000000, -0.000000000000000000 ) ) ;
#21575 = DIRECTION ( 'NONE',  ( -1.000000000000000000, -0.000000000000000000, -0.000000000000000000 ) ) ;
#21576 = CARTESIAN_POINT ( 'NONE',  ( -166.6959734468149463, 1.750000000000010658, -79.18171244307201562 ) ) ;
#21577 = CARTESIAN_POINT ( 'NONE',  ( 135.0000000000021600, 17.00000000000000000, 115.0000000000000142 ) ) ;
#21578 = CARTESIAN_POINT ( 'NONE',  ( 14.86945752723346637, 7.944783388879009145, 2.590526750877053086 ) ) ;
#21579 = ORIENTED_EDGE ( 'NONE', *, *, #23968, .F. ) ;
#21580 = ORIENTED_EDGE ( 'NONE', *, *, #39450, .T. ) ;
#21581 = DIRECTION ( 'NONE',  ( -1.000000000000000000, -0.000000000000000000, -0.000000000000000000 ) ) ;
#21582 = EDGE_CURVE ( 'NONE', #22540, #47191, #25207, .T. ) ;
#21583 = VERTEX_POINT ( 'NONE', #37296 ) ;
#21584 = ADVANCED_FACE ( 'NONE', ( #40852 ), #5701, .T. ) ;
#21585 = CARTESIAN_POINT ( 'NONE',  ( -20.20970188815926250, -31.63128376650800533, 3.209567239418976481 ) ) ;
#21586 = DIRECTION ( 'NONE',  ( 1.000000000000000000, 0.000000000000000000, 0.000000000000000000 ) ) ;
#21587 = EDGE_LOOP ( 'NONE', ( #7793, #5501, #11735, #50367, #8891, #9997, #21854, #47987 ) ) ;
#21588 = CARTESIAN_POINT ( 'NONE',  ( 10.49999999999996447, 8.875661936878628921, -18.94832733001756253 ) ) ;
#21589 = EDGE_CURVE ( 'NONE', #16313, #24770, #41916, .T. ) ;
#21590 = DIRECTION ( 'NONE',  ( 0.000000000000000000, 0.000000000000000000, 1.000000000000000000 ) ) ;
#21591 = VERTEX_POINT ( 'NONE', #37537 ) ;
#21592 = DIRECTION ( 'NONE',  ( -0.000000000000000000, -0.000000000000000000, -1.000000000000000000 ) ) ;
#21593 = DIRECTION ( 'NONE',  ( 0.000000000000000000, 0.000000000000000000, 1.000000000000000000 ) ) ;
#21594 = EDGE_CURVE ( 'NONE', #48103, #41850, #12108, .T. ) ;
#21595 = LINE ( 'NONE', #16745, #15946 ) ;
#21596 = EDGE_CURVE ( 'NONE', #5763, #10383, #46520, .T. ) ;
#21597 = CARTESIAN_POINT ( 'NONE',  ( -204.9459734468149463, 2.143131898507880377E-16, 42.56828755692798438 ) ) ;
#21598 = ORIENTED_EDGE ( 'NONE', *, *, #13718, .F. ) ;
#21599 = ORIENTED_EDGE ( 'NONE', *, *, #16565, .F. ) ;
#21600 = AXIS2_PLACEMENT_3D ( 'NONE', #10532, #14387, #31061 ) ;
#21601 = DIRECTION ( 'NONE',  ( 0.000000000000000000, -2.969158215481698263E-48, 1.000000000000000000 ) ) ;
#21602 = CARTESIAN_POINT ( 'NONE',  ( -4.207128120815918256E-14, 3.058192377181588826E-14, 10.00000000000000000 ) ) ;
#21603 = EDGE_CURVE ( 'NONE', #2324, #23722, #50267, .T. ) ;
#21604 = FACE_BOUND ( 'NONE', #6592, .T. ) ;
#21605 = VECTOR ( 'NONE', #37489, 1000.000000000000000 ) ;
#21606 = DIRECTION ( 'NONE',  ( 0.000000000000000000, 0.000000000000000000, -1.000000000000000000 ) ) ;
#21607 = CARTESIAN_POINT ( 'NONE',  ( -4.672045878990125800, 33.19353511768168374, 1.847720168420772691 ) ) ;
#21608 = ORIENTED_EDGE ( 'NONE', *, *, #16309, .F. ) ;
#21609 = CIRCLE ( 'NONE', #46180, 0.5000000000000004441 ) ;
#21610 = CARTESIAN_POINT ( 'NONE',  ( 164.9999999999999716, 17.00000000000000000, 29.99999999999999289 ) ) ;
#21611 = ORIENTED_EDGE ( 'NONE', *, *, #5152, .T. ) ;
#21612 = VECTOR ( 'NONE', #28451, 1000.000000000000000 ) ;
#21613 = CARTESIAN_POINT ( 'NONE',  ( 14.49999999999999822, -46.51315789473684248, -5.916985404131818171 ) ) ;
#21614 = DIRECTION ( 'NONE',  ( -1.000000000000000000, -0.000000000000000000, -0.000000000000000000 ) ) ;
#21615 = DIRECTION ( 'NONE',  ( 1.000000000000000000, 0.000000000000000000, 1.612977847700450206E-50 ) ) ;
#21616 = DIRECTION ( 'NONE',  ( 1.000000000000000000, 0.000000000000000000, 0.000000000000000000 ) ) ;
#21617 = PLANE ( 'NONE',  #19193 ) ;
#21618 = DIRECTION ( 'NONE',  ( -0.000000000000000000, -1.000000000000000000, -0.000000000000000000 ) ) ;
#21619 = ORIENTED_EDGE ( 'NONE', *, *, #10479, .T. ) ;
#21620 = DIRECTION ( 'NONE',  ( 0.5877852522924685852, 0.8090169943749507819, 0.000000000000000000 ) ) ;
#21621 = B_SPLINE_SURFACE_WITH_KNOTS ( 'NONE', 3, 3, ( 
 ( #13776, #33311, #29440, #9938 ),
 ( #18134, #25595, #2240, #21736 ),
 ( #33557, #49145, #2989, #34306 ),
 ( #37664, #42493, #27633, #43260 ) ),
 .UNSPECIFIED., .F., .F., .F.,
 ( 4, 4 ),
 ( 4, 4 ),
 ( 0.000000000000000000, 1.000000000000000000 ),
 ( 0.000000000000000000, 1.000000000000000000 ),
 .UNSPECIFIED. ) ;
#21622 = DIRECTION ( 'NONE',  ( -1.000000000000000000, 0.000000000000000000, 0.000000000000000000 ) ) ;
#21623 = FACE_OUTER_BOUND ( 'NONE', #50629, .T. ) ;
#21624 = VECTOR ( 'NONE', #31289, 1000.000000000000000 ) ;
#21625 = FACE_OUTER_BOUND ( 'NONE', #21049, .T. ) ;
#21626 = ORIENTED_EDGE ( 'NONE', *, *, #7309, .T. ) ;
#21627 = CARTESIAN_POINT ( 'NONE',  ( 21.24469349090191983, -33.89193117067290473, 910.0000000000000000 ) ) ;
#21628 = ORIENTED_EDGE ( 'NONE', *, *, #16510, .T. ) ;
#21630 = EDGE_CURVE ( 'NONE', #17911, #32197, #7738, .T. ) ;
#21629 = CARTESIAN_POINT ( 'NONE',  ( 35.05402655318504657, 2.143131898507880377E-16, 165.0000000000000000 ) ) ;
#21631 = CARTESIAN_POINT ( 'NONE',  ( 0.7849184246612691540, -1.242376769536456704, 9.958264684458541183 ) ) ;
#21632 = B_SPLINE_CURVE_WITH_KNOTS ( 'NONE', 3,
 ( #6921, #26412, #46394, #15122 ),
 .UNSPECIFIED., .F., .F.,
 ( 4, 4 ),
 ( 1.105609816134553033E-15, 0.0004154657329505368596 ),
 .UNSPECIFIED. ) ;
#21633 = CARTESIAN_POINT ( 'NONE',  ( 26.76882631152636094, -42.35470813487675201, -8.917361510505369182 ) ) ;
#21634 = EDGE_CURVE ( 'NONE', #15862, #7447, #15428, .T. ) ;
#21635 = FACE_OUTER_BOUND ( 'NONE', #25302, .T. ) ;
#21636 = AXIS2_PLACEMENT_3D ( 'NONE', #28971, #40527, #5615 ) ;
#21637 = DIRECTION ( 'NONE',  ( 0.000000000000000000, 0.000000000000000000, -1.000000000000000000 ) ) ;
#21638 = VECTOR ( 'NONE', #14769, 1000.000000000000000 ) ;
#21639 = DIRECTION ( 'NONE',  ( 0.000000000000000000, 0.000000000000000000, 1.000000000000000000 ) ) ;
#21640 = CARTESIAN_POINT ( 'NONE',  ( -8.032723559237163968, 41.13077784380362090, 7.544061037322996377 ) ) ;
#21641 = VECTOR ( 'NONE', #44980, 1000.000000000000000 ) ;
#21642 = VERTEX_POINT ( 'NONE', #26729 ) ;
#21643 = VERTEX_POINT ( 'NONE', #18246 ) ;
#21644 = CARTESIAN_POINT ( 'NONE',  ( 350.0000000000000000, 175.0000000000000284, -350.0000000000001705 ) ) ;
#21645 = AXIS2_PLACEMENT_3D ( 'NONE', #37034, #1858, #10313 ) ;
#21646 = FACE_OUTER_BOUND ( 'NONE', #45195, .T. ) ;
#21647 = ORIENTED_EDGE ( 'NONE', *, *, #2406, .F. ) ;
#21648 = VERTEX_POINT ( 'NONE', #3106 ) ;
#21649 = CARTESIAN_POINT ( 'NONE',  ( 153.3040265531850537, 1.750000000000010658, -79.18171244307201562 ) ) ;
#21650 = CARTESIAN_POINT ( 'NONE',  ( 350.0000000000001137, 181.0000000000000284, 355.9999999999997726 ) ) ;
#21651 = PLANE ( 'NONE',  #27577 ) ;
#21652 = MANIFOLD_SOLID_BREP ( 'Cut-Extrude1[3]', #35172 ) ;
#21653 = LINE ( 'NONE', #5746, #27250 ) ;
#21654 = VERTEX_POINT ( 'NONE', #50521 ) ;
#21655 = ORIENTED_EDGE ( 'NONE', *, *, #19614, .F. ) ;
#21656 = LINE ( 'NONE', #25768, #16035 ) ;
#21657 =( BOUNDED_CURVE ( )  B_SPLINE_CURVE ( 3, ( #24061, #4549, #20196, #35870 ),
 .UNSPECIFIED., .F., .F. ) 
 B_SPLINE_CURVE_WITH_KNOTS ( ( 4, 4 ),
 ( 4.712388980384689674, 6.283185307179586232 ),
 .UNSPECIFIED. ) 
 CURVE ( )  GEOMETRIC_REPRESENTATION_ITEM ( )  RATIONAL_B_SPLINE_CURVE ( ( 1.000000000000000000, 0.8047378541243649375, 0.8047378541243649375, 1.000000000000000000 ) ) 
 REPRESENTATION_ITEM ( '' )  );
#21658 = LINE ( 'NONE', #48311, #13397 ) ;
#21659 = VECTOR ( 'NONE', #35032, 1000.000000000000000 ) ;
#21660 = ORIENTED_EDGE ( 'NONE', *, *, #12940, .F. ) ;
#21661 = ORIENTED_EDGE ( 'NONE', *, *, #15300, .F. ) ;
#21662 = ADVANCED_FACE ( 'NONE', ( #46689 ), #14921, .F. ) ;
#21663 = CARTESIAN_POINT ( 'NONE',  ( -165.6708471809677974, -1.750000000000009548, -0.2068387089191121020 ) ) ;
#21664 = CARTESIAN_POINT ( 'NONE',  ( -194.9999999999999432, -173.0000000000000000, 112.0000000000000284 ) ) ;
#21665 = ORIENTED_EDGE ( 'NONE', *, *, #10053, .F. ) ;
#21666 = ORIENTED_EDGE ( 'NONE', *, *, #32494, .T. ) ;
#21667 = CARTESIAN_POINT ( 'NONE',  ( 14.49999999999999822, 12.98684210526315930, -19.37312575500900280 ) ) ;
#21668 = DIRECTION ( 'NONE',  ( -0.000000000000000000, -0.000000000000000000, -1.000000000000000000 ) ) ;
#21669 = ORIENTED_EDGE ( 'NONE', *, *, #17045, .T. ) ;
#21670 = CARTESIAN_POINT ( 'NONE',  ( -168.4459734468149463, 0.000000000000000000, 165.0000000000000000 ) ) ;
#21671 = DIRECTION ( 'NONE',  ( -0.000000000000000000, -0.000000000000000000, -1.000000000000000000 ) ) ;
#21672 = CARTESIAN_POINT ( 'NONE',  ( 154.1026953830863420, -98.56198943095992604, 22.84256005001721945 ) ) ;
#21673 = DIRECTION ( 'NONE',  ( -1.000000000000000000, 0.000000000000000000, 0.000000000000000000 ) ) ;
#21674 = AXIS2_PLACEMENT_3D ( 'NONE', #17556, #33227, #44227 ) ;
#21675 = CARTESIAN_POINT ( 'NONE',  ( -166.6959734468149463, -1.750000000000010658, 80.81828755692798438 ) ) ;
#21676 = ORIENTED_EDGE ( 'NONE', *, *, #40268, .T. ) ;
#21677 = CARTESIAN_POINT ( 'NONE',  ( 193.3040265531851105, -1.750000000000009992, 160.8182875569279702 ) ) ;
#21678 = CARTESIAN_POINT ( 'NONE',  ( 155.0540265531850537, 0.000000000000000000, 162.5682875569279702 ) ) ;
#21679 =( BOUNDED_CURVE ( )  B_SPLINE_CURVE ( 3, ( #21440, #33016, #1706, #48601 ),
 .UNSPECIFIED., .F., .F. ) 
 B_SPLINE_CURVE_WITH_KNOTS ( ( 4, 4 ),
 ( 4.712388980384689674, 6.283185307179586232 ),
 .UNSPECIFIED. ) 
 CURVE ( )  GEOMETRIC_REPRESENTATION_ITEM ( )  RATIONAL_B_SPLINE_CURVE ( ( 1.000000000000000000, 0.8047378541243649375, 0.8047378541243649375, 1.000000000000000000 ) ) 
 REPRESENTATION_ITEM ( '' )  );
#21680 = CARTESIAN_POINT ( 'NONE',  ( 0.000000000000000000, 15.00000000000000000, 0.000000000000000000 ) ) ;
#21681 = DIRECTION ( 'NONE',  ( -1.000000000000000000, 0.000000000000000000, 0.000000000000000000 ) ) ;
#21682 = CARTESIAN_POINT ( 'NONE',  ( 0.2458784654125734381, 0.3384226744270686926, 9.992713367193012175 ) ) ;
#21683 = LINE ( 'NONE', #17836, #8963 ) ;
#21684 = CARTESIAN_POINT ( 'NONE',  ( 228.9999999999999716, -169.9999999999999716, 444.9999999999998295 ) ) ;
#21685 = CARTESIAN_POINT ( 'NONE',  ( 339.9999999999998863, 183.3431457505076594, -358.3431457505078583 ) ) ;
#21686 = CARTESIAN_POINT ( 'NONE',  ( 4.204997580903516941, 7.611558401714507482, 225.0000000000000000 ) ) ;
#21687 = ADVANCED_FACE ( 'NONE', ( #11585 ), #42436, .T. ) ;
#21688 = EDGE_LOOP ( 'NONE', ( #2621, #7284, #3145, #31976 ) ) ;
#21689 = FACE_OUTER_BOUND ( 'NONE', #26892, .T. ) ;
#21690 = VECTOR ( 'NONE', #13549, 1000.000000000000000 ) ;
#21691 = CARTESIAN_POINT ( 'NONE',  ( -15.57957361750255565, -5.755602074545403291, 3.266473740018926541 ) ) ;
#21692 = APPLICATION_CONTEXT ( 'automotive_design' ) ;
#21693 = AXIS2_PLACEMENT_3D ( 'NONE', #13171, #48024, #40871 ) ;
#21694 = LINE ( 'NONE', #29650, #15517 ) ;
#21695 = CARTESIAN_POINT ( 'NONE',  ( -204.9459734468149463, 2.143131898507880377E-16, -160.9317124430720014 ) ) ;
#21696 = CARTESIAN_POINT ( 'NONE',  ( -44.94597344681493922, -1.025126265847089213, -37.43171244307202272 ) ) ;
#21697 = B_SPLINE_CURVE_WITH_KNOTS ( 'NONE', 3,
 ( #4382, #27979, #37, #15932 ),
 .UNSPECIFIED., .F., .F.,
 ( 4, 4 ),
 ( 0.000000000000000000, 0.2545280377015987638 ),
 .UNSPECIFIED. ) ;
#21698 = ORIENTED_EDGE ( 'NONE', *, *, #6484, .F. ) ;
#21699 = DIRECTION ( 'NONE',  ( 0.000000000000000000, 0.000000000000000000, -1.000000000000000000 ) ) ;
#21700 = ORIENTED_EDGE ( 'NONE', *, *, #14056, .F. ) ;
#21701 = CARTESIAN_POINT ( 'NONE',  ( -164.9459734468149463, 2.143131898507880377E-16, -120.9317124430720156 ) ) ;
#21702 = CARTESIAN_POINT ( 'NONE',  ( 168.9999999999999716, -254.5000000000000000, -114.9999999999999574 ) ) ;
#21703 = VERTEX_POINT ( 'NONE', #11066 ) ;
#21704 = CARTESIAN_POINT ( 'NONE',  ( -46.69597344681494633, 1.750000000000009992, 160.8182875569279702 ) ) ;
#21705 = CARTESIAN_POINT ( 'NONE',  ( 85.00000000000184741, 17.00000000000000000, 65.00000000000000000 ) ) ;
#21706 = VECTOR ( 'NONE', #28168, 1000.000000000000000 ) ;
#21707 = VERTEX_POINT ( 'NONE', #38547 ) ;
#21708 = ORIENTED_EDGE ( 'NONE', *, *, #24647, .T. ) ;
#21709 = EDGE_LOOP ( 'NONE', ( #21126, #23371, #11943, #1926, #46747, #37337 ) ) ;
#21710 = CIRCLE ( 'NONE', #42992, 2.000000000000001776 ) ;
#21711 = FACE_OUTER_BOUND ( 'NONE', #27334, .T. ) ;
#21712 = CARTESIAN_POINT ( 'NONE',  ( 33.43156050989131955, -4.370686678976570150, 8.807470649214879543 ) ) ;
#21713 = CARTESIAN_POINT ( 'NONE',  ( -69.99999999999783995, 16.00000000000000000, 95.00000000000000000 ) ) ;
#21714 = ORIENTED_EDGE ( 'NONE', *, *, #15577, .T. ) ;
#21715 = CARTESIAN_POINT ( 'NONE',  ( -582.5000000000000000, 57.49999999999996447, -58.60000000000003695 ) ) ;
#21716 = CARTESIAN_POINT ( 'NONE',  ( -84.94597344681494633, 2.143131898507880377E-16, -40.93171244307202983 ) ) ;
#21717 = CARTESIAN_POINT ( 'NONE',  ( 23.82716369509147825, 44.49195112876006419, 8.356839323120299312 ) ) ;
#21718 = VERTEX_POINT ( 'NONE', #3359 ) ;
#21719 = ORIENTED_EDGE ( 'NONE', *, *, #11882, .T. ) ;
#21720 = CARTESIAN_POINT ( 'NONE',  ( 193.3040265531851105, 0.000000000000000000, 165.0000000000000000 ) ) ;
#21721 = EDGE_CURVE ( 'NONE', #28407, #46472, #43624, .T. ) ;
#21722 = CARTESIAN_POINT ( 'NONE',  ( 356.0000000000001137, 169.0000000000000000, 349.9999999999998295 ) ) ;
#21723 = CARTESIAN_POINT ( 'NONE',  ( 1.238491169207262432, 5.772936915101642086, 9.586754400233969520 ) ) ;
#21724 = ORIENTED_EDGE ( 'NONE', *, *, #32868, .F. ) ;
#21725 = ADVANCED_FACE ( 'NONE', ( #35957 ), #28498, .T. ) ;
#21726 = CARTESIAN_POINT ( 'NONE',  ( 112.2789002873379758, -1.749999999999996669, 41.84341382277508359 ) ) ;
#21727 = LINE ( 'NONE', #37413, #14120 ) ;
#21728 = EDGE_CURVE ( 'NONE', #43044, #37083, #19121, .T. ) ;
#21729 = VECTOR ( 'NONE', #48855, 1000.000000000000000 ) ;
#21730 = CARTESIAN_POINT ( 'NONE',  ( 181.0000000000000000, 6.000000000000060396, -340.0000000000001137 ) ) ;
#21731 = DIRECTION ( 'NONE',  ( 0.000000000000000000, -0.000000000000000000, 1.000000000000000000 ) ) ;
#21732 = CARTESIAN_POINT ( 'NONE',  ( -168.4459734468149463, 0.000000000000000000, 165.0000000000000000 ) ) ;
#21733 = VECTOR ( 'NONE', #5050, 1000.000000000000000 ) ;
#21734 = DIRECTION ( 'NONE',  ( 0.000000000000000000, -1.604368532695312981E-16, -1.000000000000000000 ) ) ;
#21735 = ADVANCED_FACE ( 'NONE', ( #47948 ), #12091, .T. ) ;
#21736 = CARTESIAN_POINT ( 'NONE',  ( 1.011271242968694084, -0.7347315653655782652, -3.333333333333333481 ) ) ;
#21738 = AXIS2_PLACEMENT_3D ( 'NONE', #16015, #16260, #31925 ) ;
#21737 = DIRECTION ( 'NONE',  ( 0.000000000000000000, 0.000000000000000000, 1.000000000000000000 ) ) ;
#21739 = EDGE_CURVE ( 'NONE', #34745, #1405, #8997, .T. ) ;
#21740 = CARTESIAN_POINT ( 'NONE',  ( 10.00000000000000000, 249.9999999999999716, 225.0000000000000000 ) ) ;
#21741 = ADVANCED_FACE ( 'NONE', ( #3874 ), #23630, .T. ) ;
#21742 = CARTESIAN_POINT ( 'NONE',  ( -33.16902712922616558, 37.70469005304312304, 1.847720168420772691 ) ) ;
#21743 = VECTOR ( 'NONE', #18516, 1000.000000000000000 ) ;
#21744 = AXIS2_PLACEMENT_3D ( 'NONE', #48771, #47761, #1623 ) ;
#21746 = AXIS2_PLACEMENT_3D ( 'NONE', #28180, #24577, #33301 ) ;
#21745 = CARTESIAN_POINT ( 'NONE',  ( -18.69789054174323084, 27.49790346457746182, -2.408242355805840784 ) ) ;
#21747 = ORIENTED_EDGE ( 'NONE', *, *, #27593, .T. ) ;
#21748 = CARTESIAN_POINT ( 'NONE',  ( 0.3862712429686894766, -1.188820645368940276, 10.00000000000000000 ) ) ;
#21749 = LINE ( 'NONE', #6353, #41408 ) ;
#21750 = EDGE_CURVE ( 'NONE', #38840, #20771, #43132, .T. ) ;
#21751 = EDGE_CURVE ( 'NONE', #9008, #16851, #43881, .T. ) ;
#21752 = AXIS2_PLACEMENT_3D ( 'NONE', #30647, #38097, #31156 ) ;
#21753 = CARTESIAN_POINT ( 'NONE',  ( 155.0540265531850537, 2.143131898507880377E-16, -120.9317124430720156 ) ) ;
#21755 = ORIENTED_EDGE ( 'NONE', *, *, #15729, .F. ) ;
#21754 = ADVANCED_FACE ( 'NONE', ( #7998 ), #24057, .T. ) ;
#21756 = DIRECTION ( 'NONE',  ( 0.000000000000000000, -1.000000000000000000, -4.687818848539279227E-49 ) ) ;
#21757 = ADVANCED_FACE ( 'NONE', ( #40054 ), #8243, .F. ) ;
#21758 = LINE ( 'NONE', #48904, #4080 ) ;
#21759 =( BOUNDED_CURVE ( )  B_SPLINE_CURVE ( 3, ( #14637, #33900, #49493, #22837 ),
 .UNSPECIFIED., .F., .F. ) 
 B_SPLINE_CURVE_WITH_KNOTS ( ( 4, 4 ),
 ( 4.712388980384689674, 6.283185307179586232 ),
 .UNSPECIFIED. ) 
 CURVE ( )  GEOMETRIC_REPRESENTATION_ITEM ( )  RATIONAL_B_SPLINE_CURVE ( ( 1.000000000000000000, 0.8047378541243649375, 0.8047378541243649375, 1.000000000000000000 ) ) 
 REPRESENTATION_ITEM ( '' )  );
#21760 = ORIENTED_EDGE ( 'NONE', *, *, #29292, .F. ) ;
#21761 = EDGE_CURVE ( 'NONE', #39341, #27105, #30002, .T. ) ;
#21762 = CARTESIAN_POINT ( 'NONE',  ( 135.0000000000003411, 17.00000000000000000, -84.99999999999998579 ) ) ;
#21763 = CARTESIAN_POINT ( 'NONE',  ( 33.30402655318503946, 1.750000000000010214, -39.18171244307202983 ) ) ;
#21764 = ADVANCED_FACE ( 'NONE', ( #20288 ), #1047, .T. ) ;
#21765 = ORIENTED_EDGE ( 'NONE', *, *, #5797, .F. ) ;
#21766 = LINE ( 'NONE', #33578, #43726 ) ;
#21767 = ORIENTED_EDGE ( 'NONE', *, *, #35566, .F. ) ;
#21768 = ORIENTED_EDGE ( 'NONE', *, *, #36183, .F. ) ;
#21769 = FACE_BOUND ( 'NONE', #34096, .T. ) ;
#21770 = ORIENTED_EDGE ( 'NONE', *, *, #33138, .T. ) ;
#21771 = DIRECTION ( 'NONE',  ( -1.000000000000000000, 0.000000000000000000, -0.000000000000000000 ) ) ;
#21772 = FACE_OUTER_BOUND ( 'NONE', #12188, .T. ) ;
#21773 = VECTOR ( 'NONE', #31965, 1000.000000000000000 ) ;
#21774 = ORIENTED_EDGE ( 'NONE', *, *, #9846, .T. ) ;
#21775 = CARTESIAN_POINT ( 'NONE',  ( 79.99999999999997158, 16.00000000000000000, -114.9999999999999858 ) ) ;
#21776 = CARTESIAN_POINT ( 'NONE',  ( 4.339432828817248122, 37.24807810779213213, -8.192531242611266862 ) ) ;
#21777 = CARTESIAN_POINT ( 'NONE',  ( -4.999999999999948486, -204.9999999999999716, -230.2499999999999716 ) ) ;
#21778 = EDGE_CURVE ( 'NONE', #37670, #26648, #39804, .T. ) ;
#21779 = ORIENTED_EDGE ( 'NONE', *, *, #25874, .T. ) ;
#21780 = CARTESIAN_POINT ( 'NONE',  ( -19.99999999999971223, 17.00000000000000000, -60.00000000000000000 ) ) ;
#21781 = DIRECTION ( 'NONE',  ( 0.000000000000000000, 0.000000000000000000, 1.000000000000000000 ) ) ;
#21782 = DIRECTION ( 'NONE',  ( 0.000000000000000000, 0.000000000000000000, -1.000000000000000000 ) ) ;
#21783 = AXIS2_PLACEMENT_3D ( 'NONE', #7147, #33852, #6892 ) ;
#21784 = EDGE_CURVE ( 'NONE', #18218, #16294, #11531, .T. ) ;
#21785 = ORIENTED_EDGE ( 'NONE', *, *, #13439, .F. ) ;
#21786 = EDGE_CURVE ( 'NONE', #37517, #14294, #16434, .T. ) ;
#21787 = CARTESIAN_POINT ( 'NONE',  ( 343.9999999999999432, 183.0000000000002274, -358.0000000000003411 ) ) ;
#21788 = FACE_OUTER_BOUND ( 'NONE', #30942, .T. ) ;
#21789 = VERTEX_POINT ( 'NONE', #41300 ) ;
#21790 = VECTOR ( 'NONE', #40115, 1000.000000000000000 ) ;
#21791 = ORIENTED_EDGE ( 'NONE', *, *, #7694, .F. ) ;
#21792 = ORIENTED_EDGE ( 'NONE', *, *, #40853, .F. ) ;
#21793 = CARTESIAN_POINT ( 'NONE',  ( -167.4999999999999716, -102.8976013127941656, -7.208237214241163926 ) ) ;
#21794 = EDGE_CURVE ( 'NONE', #45431, #13237, #44612, .T. ) ;
#21795 = CARTESIAN_POINT ( 'NONE',  ( 12.78770032058947237, 31.68259716188277864, 7.455576670931136185 ) ) ;
#21796 = EDGE_LOOP ( 'NONE', ( #42577, #48095, #44096, #26816 ) ) ;
#21797 = EDGE_CURVE ( 'NONE', #1049, #46904, #23631, .T. ) ;
#21798 = AXIS2_PLACEMENT_3D ( 'NONE', #4240, #36059, #16291 ) ;
#21799 = CARTESIAN_POINT ( 'NONE',  ( -124.9459734468149463, 2.143131898507847836E-16, -40.93171244307202983 ) ) ;
#21800 = FACE_OUTER_BOUND ( 'NONE', #19442, .T. ) ;
#21801 = DIRECTION ( 'NONE',  ( 1.000000000000000000, 0.000000000000000000, -0.000000000000000000 ) ) ;
#21802 = CARTESIAN_POINT ( 'NONE',  ( -5.320787806781440921, 8.466948512633457824, -1.544988095791843818E-15 ) ) ;
#21803 = EDGE_LOOP ( 'NONE', ( #49047, #40901, #48963, #40056 ) ) ;
#21804 = DIRECTION ( 'NONE',  ( -1.000000000000000000, 0.000000000000000000, -7.793956916774525800E-48 ) ) ;
#21805 = CARTESIAN_POINT ( 'NONE',  ( -0.7658683902953777878, 0.9641952520609238242, 9.975326647350893694 ) ) ;
#21806 = CARTESIAN_POINT ( 'NONE',  ( -47.22310614333779455, -16.46562252335923660, -3.760136334089591248 ) ) ;
#21807 = EDGE_CURVE ( 'NONE', #31511, #47298, #29754, .T. ) ;
#21808 = ORIENTED_EDGE ( 'NONE', *, *, #46852, .F. ) ;
#21809 = CONTEXT_DEPENDENT_SHAPE_REPRESENTATION ( #47589, #392 ) ;
#21810 = CARTESIAN_POINT ( 'NONE',  ( -215.0000000000000568, 164.9999999999999716, 500.0000000000000000 ) ) ;
#21811 = CARTESIAN_POINT ( 'NONE',  ( 168.9999999999999716, -254.4999999999999432, -349.9999999999999432 ) ) ;
#21812 = AXIS2_PLACEMENT_3D ( 'NONE', #1589, #17236, #16983 ) ;
#21813 = AXIS2_PLACEMENT_3D ( 'NONE', #32083, #19765, #20016 ) ;
#21814 = EDGE_CURVE ( 'NONE', #17812, #21132, #23144, .T. ) ;
#21816 = AXIS2_PLACEMENT_3D ( 'NONE', #33798, #41985, #2726 ) ;
#21815 = CARTESIAN_POINT ( 'NONE',  ( 30.00000000000217781, 16.00000000000000000, 95.00000000000000000 ) ) ;
#21817 = CARTESIAN_POINT ( 'NONE',  ( -164.9459734468149463, 2.143131898507880377E-16, -120.9317124430720156 ) ) ;
#21818 = ORIENTED_EDGE ( 'NONE', *, *, #33759, .T. ) ;
#21819 = DIRECTION ( 'NONE',  ( -1.000000000000000000, 0.000000000000000000, 1.860490536778032451E-50 ) ) ;
#21820 = DIRECTION ( 'NONE',  ( -1.000000000000000000, -0.000000000000000000, -0.000000000000000000 ) ) ;
#21821 = DIRECTION ( 'NONE',  ( -1.000000000000000000, -0.000000000000000000, -0.000000000000000000 ) ) ;
#21822 = DIRECTION ( 'NONE',  ( 0.000000000000000000, 0.000000000000000000, 1.000000000000000000 ) ) ;
#21823 = CARTESIAN_POINT ( 'NONE',  ( 0.03684434657438797472, 1.221810944802236287, 9.969517326150310055 ) ) ;
#21824 =( BOUNDED_CURVE ( )  B_SPLINE_CURVE ( 3, ( #17051, #4492, #47805, #28596 ),
 .UNSPECIFIED., .F., .F. ) 
 B_SPLINE_CURVE_WITH_KNOTS ( ( 4, 4 ),
 ( 0.000000000000000000, 1.570796326794896558 ),
 .UNSPECIFIED. ) 
 CURVE ( )  GEOMETRIC_REPRESENTATION_ITEM ( )  RATIONAL_B_SPLINE_CURVE ( ( 1.000000000000000000, 0.8047378541243649375, 0.8047378541243649375, 1.000000000000000000 ) ) 
 REPRESENTATION_ITEM ( '' )  );
#21825 = VECTOR ( 'NONE', #33170, 1000.000000000000000 ) ;
#21827 = VERTEX_POINT ( 'NONE', #48447 ) ;
#21826 = EDGE_CURVE ( 'NONE', #37534, #17053, #6153, .T. ) ;
#21828 = DIRECTION ( 'NONE',  ( -1.000000000000000000, -0.000000000000000000, -0.000000000000000000 ) ) ;
#21829 = EDGE_CURVE ( 'NONE', #9096, #18355, #7251, .T. ) ;
#21830 = ORIENTED_EDGE ( 'NONE', *, *, #7025, .T. ) ;
#21831 = DIRECTION ( 'NONE',  ( -0.000000000000000000, -1.000000000000000000, -0.000000000000000000 ) ) ;
#21832 = VECTOR ( 'NONE', #20232, 1000.000000000000227 ) ;
#21833 = EDGE_LOOP ( 'NONE', ( #48062, #33600, #4242, #16646, #48895, #30843, #11878, #20308 ) ) ;
#21834 = EDGE_CURVE ( 'NONE', #36968, #5585, #45118, .T. ) ;
#21835 = CARTESIAN_POINT ( 'NONE',  ( 164.9999999999999716, 17.00000000000000000, -90.00000000000002842 ) ) ;
#21836 = CARTESIAN_POINT ( 'NONE',  ( -14.99999999999906919, 17.00000000000000000, -24.99999999999999289 ) ) ;
#21837 =( BOUNDED_CURVE ( )  B_SPLINE_CURVE ( 3, ( #23494, #35311, #11679, #19629 ),
 .UNSPECIFIED., .F., .F. ) 
 B_SPLINE_CURVE_WITH_KNOTS ( ( 4, 4 ),
 ( 3.141592653589793116, 4.712388980384689674 ),
 .UNSPECIFIED. ) 
 CURVE ( )  GEOMETRIC_REPRESENTATION_ITEM ( )  RATIONAL_B_SPLINE_CURVE ( ( 1.000000000000000000, 0.8047378541243649375, 0.8047378541243649375, 1.000000000000000000 ) ) 
 REPRESENTATION_ITEM ( '' )  );
#21838 = EDGE_CURVE ( 'NONE', #9213, #16293, #704, .T. ) ;
#21839 = SURFACE_STYLE_FILL_AREA ( #45397 ) ;
#21840 = B_SPLINE_CURVE_WITH_KNOTS ( 'NONE', 3,
 ( #25334, #33801, #41737, #37657 ),
 .UNSPECIFIED., .F., .F.,
 ( 4, 4 ),
 ( 0.000000000000000000, 0.2562577668812811571 ),
 .UNSPECIFIED. ) ;
#21841 = ORIENTED_EDGE ( 'NONE', *, *, #9545, .T. ) ;
#21842 = VECTOR ( 'NONE', #42395, 1000.000000000000000 ) ;
#21843 = EDGE_CURVE ( 'NONE', #46680, #14316, #21293, .T. ) ;
#21844 = CARTESIAN_POINT ( 'NONE',  ( -1.436574951976946402, 1.361596091069438463, 9.897807938190497978 ) ) ;
#21845 = ORIENTED_EDGE ( 'NONE', *, *, #39739, .T. ) ;
#21846 = CARTESIAN_POINT ( 'NONE',  ( 195.0540265531851105, 1.025126265847088991, 162.5682875569279133 ) ) ;
#21847 = DIRECTION ( 'NONE',  ( -1.000000000000000000, -0.000000000000000000, -0.000000000000000000 ) ) ;
#21848 = CARTESIAN_POINT ( 'NONE',  ( 177.5000000000000284, 112.5000000000000000, -10.00000000000000000 ) ) ;
#21849 = CARTESIAN_POINT ( 'NONE',  ( -543.5890838333644979, 53.53801056904005407, -176.2581102438216192 ) ) ;
#21850 = CARTESIAN_POINT ( 'NONE',  ( -119.9999999999978400, 17.00000000000000000, 95.00000000000000000 ) ) ;
#21851 = ORIENTED_EDGE ( 'NONE', *, *, #23764, .F. ) ;
#21852 = ORIENTED_EDGE ( 'NONE', *, *, #26447, .T. ) ;
#21853 = LINE ( 'NONE', #9776, #16938 ) ;
#21854 = ORIENTED_EDGE ( 'NONE', *, *, #16114, .F. ) ;
#21855 = VECTOR ( 'NONE', #47618, 1000.000000000000000 ) ;
#21856 = ADVANCED_FACE ( 'NONE', ( #17199 ), #10258, .T. ) ;
#21857 = FACE_OUTER_BOUND ( 'NONE', #7449, .T. ) ;
#21858 = DIRECTION ( 'NONE',  ( 0.000000000000000000, 1.000000000000000000, 0.000000000000000000 ) ) ;
#21859 = VECTOR ( 'NONE', #18062, 1000.000000000000000 ) ;
#21860 = EDGE_LOOP ( 'NONE', ( #25428, #966 ) ) ;
#21861 = CARTESIAN_POINT ( 'NONE',  ( -167.7210997126620384, -1.750000000000009548, -38.15658617722494483 ) ) ;
#21862 = CARTESIAN_POINT ( 'NONE',  ( 181.0000000000000000, -97.49999999999998579, -340.0000000000001137 ) ) ;
#21863 = ORIENTED_EDGE ( 'NONE', *, *, #47288, .F. ) ;
#21864 = CARTESIAN_POINT ( 'NONE',  ( 193.3040265531851105, 1.750000000000010658, -79.18171244307201562 ) ) ;
#21865 = CARTESIAN_POINT ( 'NONE',  ( -16.52264463346130796, 2.779753662172870232, 9.403735324607438884 ) ) ;
#21866 = LINE ( 'NONE', #29808, #6926 ) ;
#21867 = CARTESIAN_POINT ( 'NONE',  ( -126.6959734468149321, -1.749999999999996891, 160.8182875569279702 ) ) ;
#21868 = CARTESIAN_POINT ( 'NONE',  ( 339.9999999999999432, -171.9999999999999147, -347.0000000000001137 ) ) ;
#21869 = ORIENTED_EDGE ( 'NONE', *, *, #29694, .T. ) ;
#21870 = ORIENTED_EDGE ( 'NONE', *, *, #21778, .F. ) ;
#21871 = VERTEX_POINT ( 'NONE', #44371 ) ;
#21872 = EDGE_CURVE ( 'NONE', #7557, #17122, #44864, .T. ) ;
#21873 = CARTESIAN_POINT ( 'NONE',  ( -5.000000000000000000, -165.1999999999999602, -359.8000000000002387 ) ) ;
#21874 = CARTESIAN_POINT ( 'NONE',  ( -2.961022939495062900, 16.59676755884084187, 2.590526750877053086 ) ) ;
#21875 = ORIENTED_EDGE ( 'NONE', *, *, #46826, .F. ) ;
#21876 = CIRCLE ( 'NONE', #32547, 2.000000000000001776 ) ;
#21877 = DIRECTION ( 'NONE',  ( 1.333906992743555050E-23, -1.000000000000000000, 0.000000000000000000 ) ) ;
#21878 = ORIENTED_EDGE ( 'NONE', *, *, #18322, .F. ) ;
#21879 = CARTESIAN_POINT ( 'NONE',  ( 75.05402655318509630, -1.025126265847089213, -160.9317124430720014 ) ) ;
#21880 = DIRECTION ( 'NONE',  ( -1.000000000000000000, -0.000000000000000000, -0.000000000000000000 ) ) ;
#21881 = CARTESIAN_POINT ( 'NONE',  ( -0.3370904143228963812, 0.2449105217885287067, 10.00000000000000000 ) ) ;
#21882 = DIRECTION ( 'NONE',  ( -1.000000000000000000, -0.000000000000000000, -0.000000000000000000 ) ) ;
#21883 = DIRECTION ( 'NONE',  ( 0.000000000000000000, 0.000000000000000000, 1.000000000000000000 ) ) ;
#21884 = CARTESIAN_POINT ( 'NONE',  ( 33.30402655318503946, 1.750000000000010658, 80.81828755692798438 ) ) ;
#21885 = EDGE_LOOP ( 'NONE', ( #2619, #9492, #26470, #50435 ) ) ;
#21886 = CARTESIAN_POINT ( 'NONE',  ( -2.491056982571220324, 9.716321351877633461, 9.390253821402618328 ) ) ;
#21887 = DIRECTION ( 'NONE',  ( 0.000000000000000000, -0.000000000000000000, -1.000000000000000000 ) ) ;
#21888 = CARTESIAN_POINT ( 'NONE',  ( -168.4459734468149747, -1.025126265847089879, -77.43171244307200141 ) ) ;
#21889 = EDGE_CURVE ( 'NONE', #9188, #29536, #21046, .T. ) ;
#21890 = CARTESIAN_POINT ( 'NONE',  ( 16.99749102614301677, -1.320765928724307425, 8.953103998512858652 ) ) ;
#21891 = EDGE_CURVE ( 'NONE', #15960, #42459, #33615, .T. ) ;
#21893 = VERTEX_POINT ( 'NONE', #28993 ) ;
#21892 = VECTOR ( 'NONE', #21230, 1000.000000000000000 ) ;
#21894 = DIRECTION ( 'NONE',  ( 0.000000000000000000, 0.000000000000000000, -1.000000000000000000 ) ) ;
#21895 = ORIENTED_EDGE ( 'NONE', *, *, #18036, .T. ) ;
#21896 = PLANE ( 'NONE',  #45064 ) ;
#21897 = B_SPLINE_CURVE_WITH_KNOTS ( 'NONE', 3,
 ( #41453, #38378, #37385, #41191 ),
 .UNSPECIFIED., .F., .F.,
 ( 4, 4 ),
 ( 0.9688112071879398934, 0.9724175925769218409 ),
 .UNSPECIFIED. ) ;
#21898 = EDGE_CURVE ( 'NONE', #29622, #5743, #32867, .T. ) ;
#21899 = LINE ( 'NONE', #14687, #8343 ) ;
#21900 = ADVANCED_FACE ( 'NONE', ( #2054 ), #13828, .T. ) ;
#21901 = EDGE_CURVE ( 'NONE', #5114, #7869, #48004, .T. ) ;
#21902 = CYLINDRICAL_SURFACE ( 'NONE', #36105, 1.750000000000015543 ) ;
#21903 = ORIENTED_EDGE ( 'NONE', *, *, #2346, .T. ) ;
#21904 = CARTESIAN_POINT ( 'NONE',  ( 71.55402655318505367, 0.000000000000000000, 165.0000000000000000 ) ) ;
#21905 = CARTESIAN_POINT ( 'NONE',  ( 181.0000000000000000, -252.4999999999999432, -339.9999999999998863 ) ) ;
#21906 = DIRECTION ( 'NONE',  ( 0.000000000000000000, 0.000000000000000000, -1.000000000000000000 ) ) ;
#21907 = EDGE_CURVE ( 'NONE', #8209, #39875, #34371, .T. ) ;
#21908 = ORIENTED_EDGE ( 'NONE', *, *, #5545, .T. ) ;
#21909 = ORIENTED_EDGE ( 'NONE', *, *, #6454, .T. ) ;
#21910 = CARTESIAN_POINT ( 'NONE',  ( -33.14391172085785797, -37.72293746533094350, -8.016098858316205167 ) ) ;
#21911 = CARTESIAN_POINT ( 'NONE',  ( -64.99999999999815259, 17.00000000000000000, 65.00000000000000000 ) ) ;
#21912 = ORIENTED_EDGE ( 'NONE', *, *, #40592, .F. ) ;
#21913 = ORIENTED_EDGE ( 'NONE', *, *, #14351, .F. ) ;
#21914 = CARTESIAN_POINT ( 'NONE',  ( 0.8965959638259385356, 1.582931917743541028, 9.903764339332076005 ) ) ;
#21915 = DIRECTION ( 'NONE',  ( 0.000000000000000000, 1.000000000000000000, 0.000000000000000000 ) ) ;
#21916 = FACE_OUTER_BOUND ( 'NONE', #18158, .T. ) ;
#21917 = ORIENTED_EDGE ( 'NONE', *, *, #42816, .T. ) ;
#21918 = CARTESIAN_POINT ( 'NONE',  ( -114.9999999999984652, 17.00000000000000000, 35.00000000000000000 ) ) ;
#21919 = EDGE_LOOP ( 'NONE', ( #49318, #46459, #27070, #41369, #1620, #41400 ) ) ;
#21920 = DIRECTION ( 'NONE',  ( 0.9928768384869219865, 0.000000000000000000, 0.1191452206184307611 ) ) ;
#21921 = LINE ( 'NONE', #41414, #10141 ) ;
#21922 = AXIS2_PLACEMENT_3D ( 'NONE', #37364, #29131, #26039 ) ;
#21923 = ORIENTED_EDGE ( 'NONE', *, *, #5614, .T. ) ;
#21924 = ORIENTED_EDGE ( 'NONE', *, *, #17706, .F. ) ;
#21925 = LINE ( 'NONE', #45231, #4647 ) ;
#21926 = FACE_OUTER_BOUND ( 'NONE', #19555, .T. ) ;
#21927 = ORIENTED_EDGE ( 'NONE', *, *, #3520, .T. ) ;
#21928 = CARTESIAN_POINT ( 'NONE',  ( 358.0000000000000000, -167.8284271247461845, 342.8284271247460424 ) ) ;
#21929 = ORIENTED_EDGE ( 'NONE', *, *, #47227, .T. ) ;
#21930 = EDGE_CURVE ( 'NONE', #29168, #16294, #7167, .T. ) ;
#21931 = DIRECTION ( 'NONE',  ( 0.000000000000000000, -1.000000000000000000, 0.000000000000000000 ) ) ;
#21932 =( NAMED_UNIT ( * ) SI_UNIT ( $, .STERADIAN. ) SOLID_ANGLE_UNIT ( ) );
#21933 = ORIENTED_EDGE ( 'NONE', *, *, #43046, .F. ) ;
#21934 = CARTESIAN_POINT ( 'NONE',  ( -6.695973446814940111, 0.000000000000000000, 165.0000000000000000 ) ) ;
#21935 = CARTESIAN_POINT ( 'NONE',  ( 0.000000000000000000, 181.0000000000000284, 343.9999999999997726 ) ) ;
#21936 = LINE ( 'NONE', #37601, #39252 ) ;
#21937 = LINE ( 'NONE', #37604, #25770 ) ;
#21938 = VERTEX_POINT ( 'NONE', #45866 ) ;
#21939 = DIRECTION ( 'NONE',  ( 0.000000000000000000, 0.9545212652235329776, -0.2981428420003837121 ) ) ;
#21940 = CARTESIAN_POINT ( 'NONE',  ( 181.0000000000000000, 165.0000000000000000, -344.0000000000001137 ) ) ;
#21941 = DIRECTION ( 'NONE',  ( 0.000000000000000000, 0.000000000000000000, -1.000000000000000000 ) ) ;
#21942 = PLANE ( 'NONE',  #41334 ) ;
#21943 = DIRECTION ( 'NONE',  ( 0.000000000000000000, -1.000000000000000000, 0.000000000000000000 ) ) ;
#21944 = CARTESIAN_POINT ( 'NONE',  ( 153.3040265531850537, 0.000000000000000000, 165.0000000000000000 ) ) ;
#21945 = CARTESIAN_POINT ( 'NONE',  ( 342.0000000000000000, 2.999999999999780176, -172.0000000000003126 ) ) ;
#21946 = DIRECTION ( 'NONE',  ( 1.000000000000000000, 0.000000000000000000, -0.000000000000000000 ) ) ;
#21947 = CARTESIAN_POINT ( 'NONE',  ( 0.3862712429686978033, -1.188820645368937834, -3.333333333333333481 ) ) ;
#21948 = ADVANCED_FACE ( 'NONE', ( #31031 ), #15001, .T. ) ;
#21949 = EDGE_CURVE ( 'NONE', #829, #960, #7915, .T. ) ;
#21950 = VERTEX_POINT ( 'NONE', #34622 ) ;
#21951 = CARTESIAN_POINT ( 'NONE',  ( 0.2778388845795309314, -1.251314014313100520, 9.976582533991681601 ) ) ;
#21952 = CARTESIAN_POINT ( 'NONE',  ( -46.10908423965022251, -19.89422939639105437, 1.847720168420772691 ) ) ;
#21953 = LINE ( 'NONE', #46271, #13883 ) ;
#21954 = EDGE_CURVE ( 'NONE', #2747, #343, #41800, .T. ) ;
#21955 = CARTESIAN_POINT ( 'NONE',  ( 342.0000000000000000, -167.8284271247462414, -342.8284271247464972 ) ) ;
#21956 = CARTESIAN_POINT ( 'NONE',  ( 14.49999999999999822, 12.98684210526315930, -19.37312575500900280 ) ) ;
#21957 = ORIENTED_EDGE ( 'NONE', *, *, #18001, .T. ) ;
#21958 = ORIENTED_EDGE ( 'NONE', *, *, #29300, .F. ) ;
#21959 = DIRECTION ( 'NONE',  ( -1.586032892321652236E-16, -1.000000000000000000, -2.288264760618012091E-48 ) ) ;
#21960 = CARTESIAN_POINT ( 'NONE',  ( 181.0000000000000000, -174.9999999999999716, -356.0000000000001705 ) ) ;
#21961 =( BOUNDED_CURVE ( )  B_SPLINE_CURVE ( 3, ( #15071, #46074, #26871, #7896 ),
 .UNSPECIFIED., .F., .F. ) 
 B_SPLINE_CURVE_WITH_KNOTS ( ( 4, 4 ),
 ( 4.712388980384693227, 6.283185307179586232 ),
 .UNSPECIFIED. ) 
 CURVE ( )  GEOMETRIC_REPRESENTATION_ITEM ( )  RATIONAL_B_SPLINE_CURVE ( ( 1.000000000000000000, 0.8047378541243658256, 0.8047378541243658256, 1.000000000000000000 ) ) 
 REPRESENTATION_ITEM ( '' )  );
#21962 = ORIENTED_EDGE ( 'NONE', *, *, #23738, .T. ) ;
#21963 = CARTESIAN_POINT ( 'NONE',  ( -1.011271242968683426, -0.7347315653655928092, 10.00000000000000000 ) ) ;
#21964 = CARTESIAN_POINT ( 'NONE',  ( 168.9999999999999716, -174.9999999999999716, -356.0000000000001705 ) ) ;
#21965 = VERTEX_POINT ( 'NONE', #22048 ) ;
#21966 = ORIENTED_EDGE ( 'NONE', *, *, #50537, .F. ) ;
#21967 =( BOUNDED_CURVE ( )  B_SPLINE_CURVE ( 3, ( #31796, #39746, #12035, #46385 ),
 .UNSPECIFIED., .F., .F. ) 
 B_SPLINE_CURVE_WITH_KNOTS ( ( 4, 4 ),
 ( 3.141592653589793116, 4.712388980384689674 ),
 .UNSPECIFIED. ) 
 CURVE ( )  GEOMETRIC_REPRESENTATION_ITEM ( )  RATIONAL_B_SPLINE_CURVE ( ( 1.000000000000000000, 0.8047378541243649375, 0.8047378541243649375, 1.000000000000000000 ) ) 
 REPRESENTATION_ITEM ( '' )  );
#21968 = ORIENTED_EDGE ( 'NONE', *, *, #16489, .F. ) ;
#21969 = DIRECTION ( 'NONE',  ( -0.000000000000000000, 3.186989995019654210E-49, 1.000000000000000000 ) ) ;
#21970 = CARTESIAN_POINT ( 'NONE',  ( -1.543575080196365468, 5.756315878809935782, -4.878909776184769953E-16 ) ) ;
#21971 = LINE ( 'NONE', #22225, #35775 ) ;
#21972 = ORIENTED_EDGE ( 'NONE', *, *, #36167, .T. ) ;
#21973 = CARTESIAN_POINT ( 'NONE',  ( 350.0000000000001137, 169.0000000000000000, 343.9999999999997726 ) ) ;
#21974 = DIRECTION ( 'NONE',  ( 0.000000000000000000, 1.000000000000000000, 0.000000000000000000 ) ) ;
#21975 = CARTESIAN_POINT ( 'NONE',  ( -48.44597344681495343, 0.000000000000000000, -117.4317124430720156 ) ) ;
#21976 = EDGE_LOOP ( 'NONE', ( #1789, #4380, #17255, #25364 ) ) ;
#21977 = ORIENTED_EDGE ( 'NONE', *, *, #35748, .F. ) ;
#21978 = CARTESIAN_POINT ( 'NONE',  ( 356.0000000000000000, 175.0000000000000284, -108.0000000000002132 ) ) ;
#21979 = DIRECTION ( 'NONE',  ( 1.000000000000000000, 0.000000000000000000, 0.000000000000000000 ) ) ;
#21980 =( BOUNDED_CURVE ( )  B_SPLINE_CURVE ( 3, ( #19769, #46679, #35949, #27977 ),
 .UNSPECIFIED., .F., .F. ) 
 B_SPLINE_CURVE_WITH_KNOTS ( ( 4, 4 ),
 ( 4.712388980384689674, 6.283185307179586232 ),
 .UNSPECIFIED. ) 
 CURVE ( )  GEOMETRIC_REPRESENTATION_ITEM ( )  RATIONAL_B_SPLINE_CURVE ( ( 1.000000000000000000, 0.8047378541243649375, 0.8047378541243649375, 1.000000000000000000 ) ) 
 REPRESENTATION_ITEM ( '' )  );
#21981 = DIRECTION ( 'NONE',  ( 1.000000000000000000, 0.000000000000000000, 0.000000000000000000 ) ) ;
#21982 = VERTEX_POINT ( 'NONE', #50202 ) ;
#21983 = EDGE_CURVE ( 'NONE', #16166, #7390, #46384, .T. ) ;
#21984 = DIRECTION ( 'NONE',  ( 0.000000000000000000, -0.000000000000000000, 1.000000000000000000 ) ) ;
#21985 = CARTESIAN_POINT ( 'NONE',  ( -168.4459734468149463, 0.000000000000000000, 122.5682875569279702 ) ) ;
#21986 = DIRECTION ( 'NONE',  ( -1.000000000000000000, -0.000000000000000000, -0.000000000000000000 ) ) ;
#21987 = DIRECTION ( 'NONE',  ( -1.000000000000000000, 0.000000000000000000, 0.000000000000000000 ) ) ;
#21988 = CIRCLE ( 'NONE', #31863, 3.749999999999975575 ) ;
#21989 = MANIFOLD_SOLID_BREP ( 'Square tube 20 X 20 X 2(1)[11]', #3970 ) ;
#21990 = CARTESIAN_POINT ( 'NONE',  ( -47.55282581475773185, 15.45084971874723934, 0.000000000000000000 ) ) ;
#21991 = FACE_OUTER_BOUND ( 'NONE', #9893, .T. ) ;
#21992 = DIRECTION ( 'NONE',  ( 0.000000000000000000, 0.000000000000000000, 1.000000000000000000 ) ) ;
#21993 = CARTESIAN_POINT ( 'NONE',  ( -15.00000000000001421, 16.00000000000000000, -114.9999999999999858 ) ) ;
#21994 = B_SPLINE_CURVE_WITH_KNOTS ( 'NONE', 3,
 ( #25921, #37486, #14096, #45124 ),
 .UNSPECIFIED., .F., .F.,
 ( 4, 4 ),
 ( 0.8097120833243680593, 0.9322955464062552267 ),
 .UNSPECIFIED. ) ;
#21995 = CARTESIAN_POINT ( 'NONE',  ( 111.5540265531850679, 0.000000000000000000, -120.9317124430720156 ) ) ;
#21996 = CARTESIAN_POINT ( 'NONE',  ( 34.08355720199905647, -2.371364769369109116, 7.455576670931136185 ) ) ;
#21997 = CARTESIAN_POINT ( 'NONE',  ( 115.0540265531850395, -1.025126265847081664, 162.5682875569279133 ) ) ;
#21998 = VERTEX_POINT ( 'NONE', #18445 ) ;
#21999 = CARTESIAN_POINT ( 'NONE',  ( 339.9999999999999432, -169.0000000000001137, 344.0000000000000000 ) ) ;
#22000 = DIRECTION ( 'NONE',  ( -1.000000000000000000, 0.000000000000000000, -1.612977847700450206E-50 ) ) ;
#22001 = CARTESIAN_POINT ( 'NONE',  ( -5.670847180967843570, -1.750000000000023315, 39.79316129108089228 ) ) ;
#22002 = ORIENTED_EDGE ( 'NONE', *, *, #11198, .T. ) ;
#22003 = DIRECTION ( 'NONE',  ( -1.000000000000000000, -0.000000000000000000, -0.000000000000000000 ) ) ;
#22004 = ORIENTED_EDGE ( 'NONE', *, *, #49465, .F. ) ;
#22005 = CARTESIAN_POINT ( 'NONE',  ( -64.99999999999940314, 17.00000000000000000, -30.00000000000000000 ) ) ;
#22006 = ADVANCED_FACE ( 'NONE', ( #4076 ), #30776, .T. ) ;
#22007 = CARTESIAN_POINT ( 'NONE',  ( 0.000000000000000000, 185.0000000000000284, -344.0000000000001705 ) ) ;
#22008 = CARTESIAN_POINT ( 'NONE',  ( -7.822422304254325276, 2.683863964738837371, 229.0000000000000000 ) ) ;
#22009 = VERTEX_POINT ( 'NONE', #8184 ) ;
#22010 = ORIENTED_EDGE ( 'NONE', *, *, #26455, .T. ) ;
#22011 = ORIENTED_EDGE ( 'NONE', *, *, #21797, .F. ) ;
#22012 = CARTESIAN_POINT ( 'NONE',  ( 0.000000000000000000, 0.000000000000000000, 0.000000000000000000 ) ) ;
#22013 = VECTOR ( 'NONE', #6019, 1000.000000000000000 ) ;
#22014 = AXIS2_PLACEMENT_3D ( 'NONE', #14614, #19212, #2807 ) ;
#22015 = ORIENTED_EDGE ( 'NONE', *, *, #26230, .F. ) ;
#22016 = CARTESIAN_POINT ( 'NONE',  ( 0.000000000000000000, 0.000000000000000000, 1000.000000000000000 ) ) ;
#22017 = CARTESIAN_POINT ( 'NONE',  ( -31.94178169330213279, 9.256608784834037706, -3.760136334089591248 ) ) ;
#22018 =( BOUNDED_CURVE ( )  B_SPLINE_CURVE ( 3, ( #8996, #16953, #44121, #13086 ),
 .UNSPECIFIED., .F., .F. ) 
 B_SPLINE_CURVE_WITH_KNOTS ( ( 4, 4 ),
 ( 0.000000000000000000, 1.570796326794896558 ),
 .UNSPECIFIED. ) 
 CURVE ( )  GEOMETRIC_REPRESENTATION_ITEM ( )  RATIONAL_B_SPLINE_CURVE ( ( 1.000000000000000000, 0.8047378541243649375, 0.8047378541243649375, 1.000000000000000000 ) ) 
 REPRESENTATION_ITEM ( '' )  );
#22019 = PLANE ( 'NONE',  #15480 ) ;
#22020 = EDGE_CURVE ( 'NONE', #9657, #13193, #27427, .T. ) ;
#22021 = CARTESIAN_POINT ( 'NONE',  ( 168.9999999999999716, -254.4999999999999432, -339.9999999999998863 ) ) ;
#22022 = CARTESIAN_POINT ( 'NONE',  ( 341.9999999999999432, 169.0000000000000568, -344.0000000000002842 ) ) ;
#22023 = ORIENTED_EDGE ( 'NONE', *, *, #29379, .F. ) ;
#22024 = EDGE_CURVE ( 'NONE', #19380, #14899, #2337, .T. ) ;
#22025 = DIRECTION ( 'NONE',  ( -1.000000000000000000, 0.000000000000000000, 1.387778780781444413E-14 ) ) ;
#22026 = CARTESIAN_POINT ( 'NONE',  ( 195.0540265531851105, 2.143131898507880377E-16, -120.9317124430720156 ) ) ;
#22027 = LINE ( 'NONE', #49689, #30807 ) ;
#22028 = VECTOR ( 'NONE', #1079, 1000.000000000000000 ) ;
#22029 = ORIENTED_EDGE ( 'NONE', *, *, #31352, .T. ) ;
#22030 = CARTESIAN_POINT ( 'NONE',  ( -8.445973446814976526, 0.000000000000000000, 79.06828755692795596 ) ) ;
#22031 = LINE ( 'NONE', #42294, #20413 ) ;
#22032 = VERTEX_POINT ( 'NONE', #15878 ) ;
#22033 = ORIENTED_EDGE ( 'NONE', *, *, #35406, .F. ) ;
#22034 = ORIENTED_EDGE ( 'NONE', *, *, #44390, .T. ) ;
#22035 = LINE ( 'NONE', #49193, #48282 ) ;
#22036 = DIRECTION ( 'NONE',  ( 0.000000000000000000, 0.000000000000000000, -1.000000000000000000 ) ) ;
#22037 = B_SPLINE_SURFACE_WITH_KNOTS ( 'NONE', 3, 3, ( 
 ( #6782, #14479, #46249, #22428 ),
 ( #18569, #11148, #26537, #34245 ),
 ( #49824, #14733, #26794, #42176 ),
 ( #7044, #38355, #18819, #34501 ) ),
 .UNSPECIFIED., .F., .F., .F.,
 ( 4, 4 ),
 ( 4, 4 ),
 ( 0.000000000000000000, 1.000000000000000000 ),
 ( 0.000000000000000000, 1.000000000000000000 ),
 .UNSPECIFIED. ) ;
#22038 = EDGE_CURVE ( 'NONE', #3725, #18575, #20471, .T. ) ;
#22039 = EDGE_LOOP ( 'NONE', ( #22868, #7005, #34170, #35170, #13957, #4319, #43495, #37500 ) ) ;
#22040 = EDGE_CURVE ( 'NONE', #10853, #33462, #44730, .T. ) ;
#22041 = CARTESIAN_POINT ( 'NONE',  ( 210.0000000000000568, 0.000000000000000000, -37.43171244307202272 ) ) ;
#22042 = CARTESIAN_POINT ( 'NONE',  ( 1.250000000000000222, 0.000000000000000000, 10.00000000000000000 ) ) ;
#22043 = DIRECTION ( 'NONE',  ( -1.000000000000000000, 0.000000000000000000, 0.000000000000000000 ) ) ;
#22044 = ADVANCED_FACE ( 'NONE', ( #23313 ), #36550, .T. ) ;
#22045 = CYLINDRICAL_SURFACE ( 'NONE', #36678, 10.00000000000000000 ) ;
#22046 = EDGE_LOOP ( 'NONE', ( #8286, #41329, #50055, #33486, #43529, #39350 ) ) ;
#22047 = CARTESIAN_POINT ( 'NONE',  ( 35.05402655318504657, 2.143131898507880377E-16, -0.9317124430720247208 ) ) ;
#22048 = CARTESIAN_POINT ( 'NONE',  ( 195.0540265531851105, 2.143131898507880377E-16, 2.568287556927978166 ) ) ;
#22049 = CARTESIAN_POINT ( 'NONE',  ( 15.00000000000000000, -46.51315789473684248, -6.315789473684215949 ) ) ;
#22050 = ORIENTED_EDGE ( 'NONE', *, *, #46571, .T. ) ;
#22051 = CIRCLE ( 'NONE', #49861, 3.500000000000003109 ) ;
#22052 = CARTESIAN_POINT ( 'NONE',  ( 191.5540265531850537, -1.025126265847089435, -40.93171244307204404 ) ) ;
#22053 = LINE ( 'NONE', #22306, #33981 ) ;
#22054 =( BOUNDED_CURVE ( )  B_SPLINE_CURVE ( 3, ( #40673, #17563, #29116, #44737 ),
 .UNSPECIFIED., .F., .F. ) 
 B_SPLINE_CURVE_WITH_KNOTS ( ( 4, 4 ),
 ( 0.000000000000000000, 1.570796326794896558 ),
 .UNSPECIFIED. ) 
 CURVE ( )  GEOMETRIC_REPRESENTATION_ITEM ( )  RATIONAL_B_SPLINE_CURVE ( ( 1.000000000000000000, 0.8047378541243649375, 0.8047378541243649375, 1.000000000000000000 ) ) 
 REPRESENTATION_ITEM ( '' )  );
#22055 = CARTESIAN_POINT ( 'NONE',  ( -14.29087950072019098, -9.652079258044555132, 8.727788335465566760 ) ) ;
#22056 = CARTESIAN_POINT ( 'NONE',  ( -124.9459734468149463, 2.143131898507847836E-16, -117.4317124430720725 ) ) ;
#22057 = ORIENTED_EDGE ( 'NONE', *, *, #14350, .F. ) ;
#22058 = VECTOR ( 'NONE', #25386, 1000.000000000000000 ) ;
#22059 = FACE_OUTER_BOUND ( 'NONE', #1110, .T. ) ;
#22060 = CIRCLE ( 'NONE', #7306, 33.33601305720110020 ) ;
#22061 = CARTESIAN_POINT ( 'NONE',  ( -0.3370904143228978245, 0.2449105217885259589, 10.00000000000000000 ) ) ;
#22062 = CARTESIAN_POINT ( 'NONE',  ( 164.9999999999999716, 16.00000000000000000, -84.99999999999998579 ) ) ;
#22063 = LINE ( 'NONE', #2560, #9397 ) ;
#22064 = ADVANCED_FACE ( 'NONE', ( #12034 ), #39745, .F. ) ;
#22065 = VECTOR ( 'NONE', #42698, 1000.000000000000000 ) ;
#22066 = ORIENTED_EDGE ( 'NONE', *, *, #8410, .T. ) ;
#22067 = EDGE_CURVE ( 'NONE', #41009, #40604, #11524, .T. ) ;
#22068 = LINE ( 'NONE', #28767, #40385 ) ;
#22069 = ORIENTED_EDGE ( 'NONE', *, *, #40228, .F. ) ;
#22070 = EDGE_CURVE ( 'NONE', #15558, #30326, #13961, .T. ) ;
#22071 = CARTESIAN_POINT ( 'NONE',  ( 75.05402655318509630, -1.025126265847089435, -40.93171244307204404 ) ) ;
#22072 = MANIFOLD_SOLID_BREP ( 'Square tube 20 X 20 X 2(1)[14]', #10527 ) ;
#22073 = ORIENTED_EDGE ( 'NONE', *, *, #30216, .F. ) ;
#22074 = CARTESIAN_POINT ( 'NONE',  ( 166.9999999999999716, 6.000000000000060396, 339.9999999999998295 ) ) ;
#22075 = EDGE_CURVE ( 'NONE', #46476, #22371, #11776, .T. ) ;
#22076 = CYLINDRICAL_SURFACE ( 'NONE', #24120, 1.750000000000015543 ) ;
#22078 = CARTESIAN_POINT ( 'NONE',  ( 75.05402655318509630, 1.025126265847089657, 119.0682875569279560 ) ) ;
#22077 = B_SPLINE_CURVE_WITH_KNOTS ( 'NONE', 3,
 ( #26467, #22618, #50015, #49516 ),
 .UNSPECIFIED., .F., .F.,
 ( 4, 4 ),
 ( 2.557173108762071179E-16, 0.0001831559689937848462 ),
 .UNSPECIFIED. ) ;
#22079 = EDGE_LOOP ( 'NONE', ( #41674, #38648, #6216, #11793 ) ) ;
#22080 = EDGE_CURVE ( 'NONE', #20319, #18505, #8441, .T. ) ;
#22081 = DIRECTION ( 'NONE',  ( -1.000000000000000000, -0.000000000000000000, -0.000000000000000000 ) ) ;
#22082 = VERTEX_POINT ( 'NONE', #732 ) ;
#22083 = CARTESIAN_POINT ( 'NONE',  ( -114.9999999999978542, 17.00000000000000000, 95.00000000000000000 ) ) ;
#22084 = LINE ( 'NONE', #45656, #23245 ) ;
#22085 = CARTESIAN_POINT ( 'NONE',  ( -25.04522487443065160, 22.77512090857326754, 8.356839323120299312 ) ) ;
#22086 = DIRECTION ( 'NONE',  ( -0.000000000000000000, -1.000000000000000000, -0.000000000000000000 ) ) ;
#22087 = CARTESIAN_POINT ( 'NONE',  ( -4.256388337216303164, 5.377297509087435756, 9.753789706659947711 ) ) ;
#22088 = EDGE_LOOP ( 'NONE', ( #16857, #37770, #11056, #10157 ) ) ;
#22089 = ORIENTED_EDGE ( 'NONE', *, *, #19134, .T. ) ;
#22090 = CARTESIAN_POINT ( 'NONE',  ( 10.50000000000000178, -46.01315789473684248, 5.916985404131814619 ) ) ;
#22091 = AXIS2_PLACEMENT_3D ( 'NONE', #35687, #31060, #27711 ) ;
#22092 = VECTOR ( 'NONE', #47397, 1000.000000000000000 ) ;
#22093 = AXIS2_PLACEMENT_3D ( 'NONE', #7567, #23203, #19857 ) ;
#22094 = VERTEX_POINT ( 'NONE', #239 ) ;
#22095 = CARTESIAN_POINT ( 'NONE',  ( 35.00000000000061107, 17.00000000000000000, -54.99999999999999289 ) ) ;
#22096 = LINE ( 'NONE', #2584, #30539 ) ;
#22097 = ORIENTED_EDGE ( 'NONE', *, *, #39950, .F. ) ;
#22098 = CARTESIAN_POINT ( 'NONE',  ( -6.695973446814940111, 1.750000000000024203, -119.1817124430720440 ) ) ;
#22099 = VECTOR ( 'NONE', #13137, 1000.000000000000000 ) ;
#22100 = CARTESIAN_POINT ( 'NONE',  ( 155.0540265531850537, 1.025126265847089657, -80.93171244307201562 ) ) ;
#22101 = EDGE_CURVE ( 'NONE', #30683, #45850, #44878, .T. ) ;
#22102 = ORIENTED_EDGE ( 'NONE', *, *, #11250, .F. ) ;
#22103 = EDGE_CURVE ( 'NONE', #33964, #21965, #4613, .T. ) ;
#22104 = FACE_BOUND ( 'NONE', #37640, .T. ) ;
#22105 = CARTESIAN_POINT ( 'NONE',  ( 1.468713901642212161, 0.3220470327672588229, 9.927319414211225990 ) ) ;
#22106 = CARTESIAN_POINT ( 'NONE',  ( -11.73320209285699889, 11.96063479729179768, 9.403735324607438884 ) ) ;
#22107 = VECTOR ( 'NONE', #34664, 1000.000000000000000 ) ;
#22108 = CARTESIAN_POINT ( 'NONE',  ( 164.9999999999999716, -9.999999999999953815, -99.00000000000014211 ) ) ;
#22109 = EDGE_CURVE ( 'NONE', #18354, #23977, #44548, .T. ) ;
#22110 = EDGE_CURVE ( 'NONE', #29505, #11397, #25593, .T. ) ;
#22111 = VERTEX_POINT ( 'NONE', #1497 ) ;
#22112 = ORIENTED_EDGE ( 'NONE', *, *, #19728, .F. ) ;
#22113 = ADVANCED_FACE ( 'NONE', ( #37418 ), #9686, .F. ) ;
#22114 = PLANE ( 'NONE',  #39833 ) ;
#22115 = EDGE_CURVE ( 'NONE', #23986, #9366, #25584, .T. ) ;
#22116 = PLANE ( 'NONE',  #30512 ) ;
#22117 = VERTEX_POINT ( 'NONE', #2239 ) ;
#22118 = PLANE ( 'NONE',  #24231 ) ;
#22119 = ORIENTED_EDGE ( 'NONE', *, *, #45880, .T. ) ;
#22120 = DIRECTION ( 'NONE',  ( -1.000000000000000000, -0.000000000000000000, -0.000000000000000000 ) ) ;
#22121 =( BOUNDED_CURVE ( )  B_SPLINE_CURVE ( 3, ( #23875, #8982, #43866, #39280 ),
 .UNSPECIFIED., .F., .F. ) 
 B_SPLINE_CURVE_WITH_KNOTS ( ( 4, 4 ),
 ( 3.141592653589793116, 4.712388980384689674 ),
 .UNSPECIFIED. ) 
 CURVE ( )  GEOMETRIC_REPRESENTATION_ITEM ( )  RATIONAL_B_SPLINE_CURVE ( ( 1.000000000000000000, 0.8047378541243649375, 0.8047378541243649375, 1.000000000000000000 ) ) 
 REPRESENTATION_ITEM ( '' )  );
#22122 = CARTESIAN_POINT ( 'NONE',  ( -64.99999999999877787, 16.00000000000000000, 30.00000000000000000 ) ) ;
#22123 = CARTESIAN_POINT ( 'NONE',  ( -24.39427009666018265, -44.07992421011638129, 8.807470649214879543 ) ) ;
#22124 = DIRECTION ( 'NONE',  ( -1.000000000000000000, 0.000000000000000000, 1.860490536778032451E-50 ) ) ;
#22125 = CARTESIAN_POINT ( 'NONE',  ( 341.9999999999999432, -165.0000000000001137, -94.00000000000019895 ) ) ;
#22126 = LINE ( 'NONE', #10825, #42811 ) ;
#22127 = VERTEX_POINT ( 'NONE', #8934 ) ;
#22128 = PLANE ( 'NONE',  #12420 ) ;
#22129 =( BOUNDED_CURVE ( )  B_SPLINE_CURVE ( 3, ( #19998, #21012, #28711, #27954 ),
 .UNSPECIFIED., .F., .F. ) 
 B_SPLINE_CURVE_WITH_KNOTS ( ( 4, 4 ),
 ( 3.141592653589793116, 4.712388980384689674 ),
 .UNSPECIFIED. ) 
 CURVE ( )  GEOMETRIC_REPRESENTATION_ITEM ( )  RATIONAL_B_SPLINE_CURVE ( ( 1.000000000000000000, 0.8047378541243649375, 0.8047378541243649375, 1.000000000000000000 ) ) 
 REPRESENTATION_ITEM ( '' )  );
#22130 = CARTESIAN_POINT ( 'NONE',  ( 35.05402655318504657, -1.025126265847089435, -40.93171244307204404 ) ) ;
#22131 = FACE_OUTER_BOUND ( 'NONE', #5099, .T. ) ;
#22132 = EDGE_CURVE ( 'NONE', #30495, #5180, #6259, .T. ) ;
#22133 = AXIS2_PLACEMENT_3D ( 'NONE', #39451, #40453, #20425 ) ;
#22134 = AXIS2_PLACEMENT_3D ( 'NONE', #10643, #14495, #26557 ) ;
#22135 = ADVANCED_FACE ( 'NONE', ( #29439 ), #40238, .F. ) ;
#22136 = PLANE ( 'NONE',  #20768 ) ;
#22137 = ORIENTED_EDGE ( 'NONE', *, *, #37894, .T. ) ;
#22138 = ADVANCED_FACE ( 'NONE', ( #40746 ), #48636, .F. ) ;
#22139 = DIRECTION ( 'NONE',  ( -0.000000000000000000, -0.000000000000000000, -1.000000000000000000 ) ) ;
#22140 = ORIENTED_EDGE ( 'NONE', *, *, #21317, .T. ) ;
#22141 = VECTOR ( 'NONE', #19451, 1000.000000000000114 ) ;
#22142 = FACE_OUTER_BOUND ( 'NONE', #403, .T. ) ;
#22143 = DIRECTION ( 'NONE',  ( -0.000000000000000000, -0.000000000000000000, -1.000000000000000000 ) ) ;
#22144 = AXIS2_PLACEMENT_3D ( 'NONE', #20780, #36460, #1301 ) ;
#22145 = CARTESIAN_POINT ( 'NONE',  ( -206.6959734468149463, -1.750000000000010658, -79.18171244307201562 ) ) ;
#22146 = EDGE_LOOP ( 'NONE', ( #24913, #32768, #40911, #46587, #41195, #48445 ) ) ;
#22147 = AXIS2_PLACEMENT_3D ( 'NONE', #25183, #40828, #1340 ) ;
#22148 = CARTESIAN_POINT ( 'NONE',  ( 15.62858259096121216, -5.755205073598612664, -9.683996418299976483 ) ) ;
#22149 = ORIENTED_EDGE ( 'NONE', *, *, #24333, .F. ) ;
#22150 = LINE ( 'NONE', #21904, #4157 ) ;
#22151 = CARTESIAN_POINT ( 'NONE',  ( -1.637520033018239118, -0.1700351954323520154, 9.927568724237804787 ) ) ;
#22152 = DIRECTION ( 'NONE',  ( -1.000000000000000000, -0.000000000000000000, -0.000000000000000000 ) ) ;
#22153 = ADVANCED_FACE ( 'NONE', ( #44310 ), #1990, .T. ) ;
#22154 = ORIENTED_EDGE ( 'NONE', *, *, #19543, .F. ) ;
#22155 = EDGE_LOOP ( 'NONE', ( #10011, #35193, #5244, #47555, #41050 ) ) ;
#22156 = DIRECTION ( 'NONE',  ( -0.000000000000000000, -0.000000000000000000, -1.000000000000000000 ) ) ;
#22157 = CARTESIAN_POINT ( 'NONE',  ( 339.9999999999999432, 169.0000000000000000, -342.0000000000001705 ) ) ;
#22158 = ORIENTED_EDGE ( 'NONE', *, *, #23298, .T. ) ;
#22159 = ORIENTED_EDGE ( 'NONE', *, *, #50266, .F. ) ;
#22160 = CARTESIAN_POINT ( 'NONE',  ( -0.2774838294623820922, 1.251476322270256736, 9.957892297621016908 ) ) ;
#22161 = CARTESIAN_POINT ( 'NONE',  ( 111.5540265531850537, -1.025126265847081886, 79.06828755692797017 ) ) ;
#22162 = EDGE_CURVE ( 'NONE', #38611, #19150, #40990, .T. ) ;
#22163 = ORIENTED_EDGE ( 'NONE', *, *, #4094, .T. ) ;
#22164 = CARTESIAN_POINT ( 'NONE',  ( 340.0000000000000568, 183.0000000000000284, 355.9999999999997726 ) ) ;
#22165 = VERTEX_POINT ( 'NONE', #13528 ) ;
#22166 = CARTESIAN_POINT ( 'NONE',  ( -128.4459734468149179, 0.000000000000000000, -37.43171244307205825 ) ) ;
#22167 = VECTOR ( 'NONE', #33333, 1000.000000000000000 ) ;
#22168 = FACE_BOUND ( 'NONE', #34206, .T. ) ;
#22169 = EDGE_CURVE ( 'NONE', #39841, #2541, #1742, .T. ) ;
#22170 = CIRCLE ( 'NONE', #62, 4.000000000000003553 ) ;
#22171 = ADVANCED_FACE ( 'NONE', ( #40494 ), #8490, .T. ) ;
#22172 = ORIENTED_EDGE ( 'NONE', *, *, #18125, .F. ) ;
#22173 = ORIENTED_EDGE ( 'NONE', *, *, #39613, .T. ) ;
#22174 = CARTESIAN_POINT ( 'NONE',  ( -1.104609456715841986, -0.6504863887005195577, 9.948547179989617462 ) ) ;
#22175 = VECTOR ( 'NONE', #3741, 1000.000000000000000 ) ;
#22176 = CARTESIAN_POINT ( 'NONE',  ( 155.0540265531850537, 1.025126265847089213, -0.9317124430720324924 ) ) ;
#22177 = ADVANCED_FACE ( 'NONE', ( #21991 ), #2736, .F. ) ;
#22178 = ORIENTED_EDGE ( 'NONE', *, *, #48045, .F. ) ;
#22179 = FACE_OUTER_BOUND ( 'NONE', #10329, .T. ) ;
#22180 = AXIS2_PLACEMENT_3D ( 'NONE', #34388, #14368, #11026 ) ;
#22181 = VERTEX_POINT ( 'NONE', #41998 ) ;
#22182 = ADVANCED_FACE ( 'NONE', ( #6593 ), #6852, .F. ) ;
#22183 = DIRECTION ( 'NONE',  ( -1.586032892321652482E-16, 0.000000000000000000, -1.000000000000000000 ) ) ;
#22184 = CARTESIAN_POINT ( 'NONE',  ( 0.000000000000000000, 0.000000000000000000, 910.0000000000000000 ) ) ;
#22185 = ORIENTED_EDGE ( 'NONE', *, *, #33138, .F. ) ;
#22186 = ADVANCED_FACE ( 'NONE', ( #49144 ), #30191, .T. ) ;
#22187 = CARTESIAN_POINT ( 'NONE',  ( 344.0000000000000000, -165.0000000000001137, -349.9999999999998863 ) ) ;
#22188 = DIRECTION ( 'NONE',  ( 0.000000000000000000, 0.000000000000000000, 1.000000000000000000 ) ) ;
#22189 = CARTESIAN_POINT ( 'NONE',  ( 10.00000000000000000, 249.9999999999999716, -224.9999999999999716 ) ) ;
#22190 = CARTESIAN_POINT ( 'NONE',  ( 35.00000000000091660, 17.00000000000000000, -24.99999999999999289 ) ) ;
#22191 = CARTESIAN_POINT ( 'NONE',  ( 181.0000000000000284, -174.9999999999999716, -115.0000000000001563 ) ) ;
#22192 = ORIENTED_EDGE ( 'NONE', *, *, #41640, .T. ) ;
#22193 = DIRECTION ( 'NONE',  ( -0.000000000000000000, -0.000000000000000000, 1.000000000000000000 ) ) ;
#22194 = CARTESIAN_POINT ( 'NONE',  ( 72.27890028733797578, -1.750000000000009548, -40.20683870891912193 ) ) ;
#22195 = EDGE_CURVE ( 'NONE', #29367, #24694, #46320, .T. ) ;
#22196 = B_SPLINE_CURVE_WITH_KNOTS ( 'NONE', 3,
 ( #44185, #39870, #43939, #44430 ),
 .UNSPECIFIED., .F., .F.,
 ( 4, 4 ),
 ( 0.000000000000000000, 0.2545280377015988749 ),
 .UNSPECIFIED. ) ;
#22197 = PLANE ( 'NONE',  #48999 ) ;
#22198 = CARTESIAN_POINT ( 'NONE',  ( 0.3862712429686810944, 1.188820645368943607, -3.333333333333333481 ) ) ;
#22199 = DIRECTION ( 'NONE',  ( 0.000000000000000000, 5.664403186863042467E-17, 1.000000000000000000 ) ) ;
#22200 = DIRECTION ( 'NONE',  ( -1.000000000000000000, 0.000000000000000000, 0.000000000000000000 ) ) ;
#22201 = CARTESIAN_POINT ( 'NONE',  ( -165.0000000000000284, 17.00000000000000000, 115.0000000000000142 ) ) ;
#22202 = CARTESIAN_POINT ( 'NONE',  ( 9.999999999999964473, 8.486842105263161073, -18.38522261288946780 ) ) ;
#22203 = DIRECTION ( 'NONE',  ( 1.000000000000000000, 0.000000000000000000, 0.000000000000000000 ) ) ;
#22204 = CIRCLE ( 'NONE', #10728, 10.00000000000000000 ) ;
#22205 = ORIENTED_EDGE ( 'NONE', *, *, #21102, .F. ) ;
#22206 = CARTESIAN_POINT ( 'NONE',  ( 0.3370904143228981575, -0.2449105217885261532, -10.00000000000000000 ) ) ;
#22207 = VECTOR ( 'NONE', #17795, 1000.000000000000227 ) ;
#22208 = CARTESIAN_POINT ( 'NONE',  ( -0.3862712429686895876, 1.188820645368940720, 10.00000000000000000 ) ) ;
#22209 = CARTESIAN_POINT ( 'NONE',  ( -7.359817328027146388, -15.16751262232800102, 2.590526750877053086 ) ) ;
#22210 = CARTESIAN_POINT ( 'NONE',  ( 1.011271242968677653, 0.7347315653656002477, 10.00000000000000000 ) ) ;
#22211 = LINE ( 'NONE', #25554, #35685 ) ;
#22212 = VERTEX_POINT ( 'NONE', #6344 ) ;
#22213 = VECTOR ( 'NONE', #45765, 1000.000000000000114 ) ;
#22214 = ORIENTED_EDGE ( 'NONE', *, *, #41930, .F. ) ;
#22215 = CARTESIAN_POINT ( 'NONE',  ( -54.99999999999997868, 52.49999999999999289, 5.000000000000000000 ) ) ;
#22216 = EDGE_CURVE ( 'NONE', #5029, #49726, #11216, .T. ) ;
#22217 = ORIENTED_EDGE ( 'NONE', *, *, #45287, .T. ) ;
#22218 = CARTESIAN_POINT ( 'NONE',  ( 111.5540265531850679, 0.000000000000000000, 165.0000000000000000 ) ) ;
#22219 = CARTESIAN_POINT ( 'NONE',  ( 342.8284271247462129, 183.0000000000000000, -358.0000000000001137 ) ) ;
#22220 = ORIENTED_EDGE ( 'NONE', *, *, #26579, .T. ) ;
#22221 = EDGE_LOOP ( 'NONE', ( #6674, #31322, #6453, #20140 ) ) ;
#22222 = EDGE_LOOP ( 'NONE', ( #33587, #10319, #30751, #29918 ) ) ;
#22223 = CARTESIAN_POINT ( 'NONE',  ( -204.9459734468148895, 1.025126265847089657, -37.43171244307202272 ) ) ;
#22224 = CARTESIAN_POINT ( 'NONE',  ( 34.08355720199905647, -2.371364769369109116, 7.455576670931136185 ) ) ;
#22225 = CARTESIAN_POINT ( 'NONE',  ( 115.0540265531850395, 2.143131898507847836E-16, 165.0000000000000000 ) ) ;
#22226 = VERTEX_POINT ( 'NONE', #45307 ) ;
#22227 = EDGE_CURVE ( 'NONE', #21569, #23180, #45447, .T. ) ;
#22228 = DIRECTION ( 'NONE',  ( 0.000000000000000000, 0.000000000000000000, 1.000000000000000000 ) ) ;
#22229 = EDGE_CURVE ( 'NONE', #39414, #47971, #10193, .T. ) ;
#22230 = DIRECTION ( 'NONE',  ( 0.000000000000000000, 0.000000000000000000, 1.000000000000000000 ) ) ;
#22231 = DIRECTION ( 'NONE',  ( -0.000000000000000000, -1.000000000000000000, -0.000000000000000000 ) ) ;
#22232 = ORIENTED_EDGE ( 'NONE', *, *, #24401, .F. ) ;
#22233 = ORIENTED_EDGE ( 'NONE', *, *, #19676, .T. ) ;
#22234 = CARTESIAN_POINT ( 'NONE',  ( 85.00000000000152056, 17.00000000000000000, 60.00000000000000000 ) ) ;
#22235 = FACE_OUTER_BOUND ( 'NONE', #1184, .T. ) ;
#22236 = VECTOR ( 'NONE', #40977, 1000.000000000000000 ) ;
#22237 = CARTESIAN_POINT ( 'NONE',  ( 153.3040265531850537, -1.750000000000010658, 120.8182875569279702 ) ) ;
#22238 = ORIENTED_EDGE ( 'NONE', *, *, #6057, .T. ) ;
#22239 = VECTOR ( 'NONE', #19720, 1000.000000000000000 ) ;
#22240 = EDGE_CURVE ( 'NONE', #35337, #17816, #25847, .T. ) ;
#22241 = CARTESIAN_POINT ( 'NONE',  ( 191.5540265531850537, 1.025126265847089213, 42.56828755692799149 ) ) ;
#22242 = EDGE_CURVE ( 'NONE', #17311, #22032, #7361, .T. ) ;
#22243 = CARTESIAN_POINT ( 'NONE',  ( -22.82242230425432439, -2.816136035261162185, 226.0000000000000000 ) ) ;
#22244 = MANIFOLD_SOLID_BREP ( 'Square tube 20 X 20 X 2(1)[18]', #30197 ) ;
#22245 = CARTESIAN_POINT ( 'NONE',  ( -46.69597344681494633, -1.750000000000009992, 160.8182875569279702 ) ) ;
#22246 = ORIENTED_EDGE ( 'NONE', *, *, #45597, .T. ) ;
#22248 = EDGE_CURVE ( 'NONE', #46611, #23935, #41743, .T. ) ;
#22247 = CARTESIAN_POINT ( 'NONE',  ( 210.0000000000000568, 2.143131898507880377E-16, 159.0682875569279702 ) ) ;
#22249 = DIRECTION ( 'NONE',  ( -1.000000000000000000, -0.000000000000000000, -0.000000000000000000 ) ) ;
#22250 = CARTESIAN_POINT ( 'NONE',  ( -69.99999999999909051, 17.00000000000000000, -24.99999999999999289 ) ) ;
#22251 = VECTOR ( 'NONE', #41133, 1000.000000000000000 ) ;
#22252 = CARTESIAN_POINT ( 'NONE',  ( -168.4459734468149463, 0.000000000000000000, -0.9317124430720247208 ) ) ;
#22253 = CARTESIAN_POINT ( 'NONE',  ( 111.5540265531850537, 1.025126265847081219, -157.4317124430720582 ) ) ;
#22254 = CARTESIAN_POINT ( 'NONE',  ( 181.0000000000000284, -174.9999999999999716, -115.0000000000001563 ) ) ;
#22255 = VERTEX_POINT ( 'NONE', #20862 ) ;
#22256 = DIRECTION ( 'NONE',  ( -1.000000000000000000, 0.000000000000000000, 0.000000000000000000 ) ) ;
#22257 = CARTESIAN_POINT ( 'NONE',  ( -4.999999999999950262, -197.4999999999999432, -228.6347188485896140 ) ) ;
#22258 = CARTESIAN_POINT ( 'NONE',  ( -6.695973446814940111, -1.750000000000023759, 40.81828755692798438 ) ) ;
#22259 =( BOUNDED_CURVE ( )  B_SPLINE_CURVE ( 3, ( #1584, #28528, #40824, #44154 ),
 .UNSPECIFIED., .F., .F. ) 
 B_SPLINE_CURVE_WITH_KNOTS ( ( 4, 4 ),
 ( 3.141592653589793116, 4.712388980384689674 ),
 .UNSPECIFIED. ) 
 CURVE ( )  GEOMETRIC_REPRESENTATION_ITEM ( )  RATIONAL_B_SPLINE_CURVE ( ( 1.000000000000000000, 0.8047378541243649375, 0.8047378541243649375, 1.000000000000000000 ) ) 
 REPRESENTATION_ITEM ( '' )  );
#22260 = EDGE_LOOP ( 'NONE', ( #18216, #42890, #8094, #31726 ) ) ;
#22261 = CARTESIAN_POINT ( 'NONE',  ( 111.5540265531850537, 1.025126265847081664, -77.43171244307201562 ) ) ;
#22262 = CARTESIAN_POINT ( 'NONE',  ( 210.0000000000000568, 0.000000000000000000, 80.81828755692798438 ) ) ;
#22263 = VERTEX_POINT ( 'NONE', #4954 ) ;
#22264 = DIRECTION ( 'NONE',  ( -1.586032892321652236E-16, -1.000000000000000000, -2.288264760618012091E-48 ) ) ;
#22265 = CYLINDRICAL_SURFACE ( 'NONE', #98, 4.000000000000003553 ) ;
#22266 = CARTESIAN_POINT ( 'NONE',  ( -128.4459734468149463, 1.025126265847081664, -77.43171244307201562 ) ) ;
#22267 = LINE ( 'NONE', #15076, #36483 ) ;
#22268 =( BOUNDED_CURVE ( )  B_SPLINE_CURVE ( 3, ( #40991, #1498, #8697, #9180 ),
 .UNSPECIFIED., .F., .F. ) 
 B_SPLINE_CURVE_WITH_KNOTS ( ( 4, 4 ),
 ( 3.141592653589793116, 4.712388980384689674 ),
 .UNSPECIFIED. ) 
 CURVE ( )  GEOMETRIC_REPRESENTATION_ITEM ( )  RATIONAL_B_SPLINE_CURVE ( ( 1.000000000000000000, 0.8047378541243649375, 0.8047378541243649375, 1.000000000000000000 ) ) 
 REPRESENTATION_ITEM ( '' )  );
#22269 = VECTOR ( 'NONE', #39993, 1000.000000000000000 ) ;
#22270 = ORIENTED_EDGE ( 'NONE', *, *, #17707, .T. ) ;
#22271 = CARTESIAN_POINT ( 'NONE',  ( 0.000000000000000000, 165.2000000000000171, -359.8000000000002387 ) ) ;
#22272 = ORIENTED_EDGE ( 'NONE', *, *, #48045, .T. ) ;
#22273 = ORIENTED_EDGE ( 'NONE', *, *, #15009, .F. ) ;
#22274 = ADVANCED_FACE ( 'NONE', ( #28819 ), #12160, .F. ) ;
#22275 = DIRECTION ( 'NONE',  ( -1.000000000000000000, 0.000000000000000000, 1.860490536778032451E-50 ) ) ;
#22276 = ORIENTED_EDGE ( 'NONE', *, *, #26962, .T. ) ;
#22277 = LINE ( 'NONE', #26117, #14760 ) ;
#22278 = CARTESIAN_POINT ( 'NONE',  ( -16.69947034530963847, 2.312583065866374632, 2.590526750877053086 ) ) ;
#22279 = CARTESIAN_POINT ( 'NONE',  ( 154.3291528190321458, -1.750000000000010436, 79.79316129108087807 ) ) ;
#22280 = DIRECTION ( 'NONE',  ( -1.000000000000000000, -0.000000000000000000, -0.000000000000000000 ) ) ;
#22281 =( BOUNDED_CURVE ( )  B_SPLINE_CURVE ( 3, ( #2838, #22100, #30565, #10545 ),
 .UNSPECIFIED., .F., .F. ) 
 B_SPLINE_CURVE_WITH_KNOTS ( ( 4, 4 ),
 ( 0.000000000000000000, 1.570796326794896558 ),
 .UNSPECIFIED. ) 
 CURVE ( )  GEOMETRIC_REPRESENTATION_ITEM ( )  RATIONAL_B_SPLINE_CURVE ( ( 1.000000000000000000, 0.8047378541243649375, 0.8047378541243649375, 1.000000000000000000 ) ) 
 REPRESENTATION_ITEM ( '' )  );
#22282 = FACE_OUTER_BOUND ( 'NONE', #50708, .T. ) ;
#22283 = EDGE_LOOP ( 'NONE', ( #1344, #3806, #6157, #49934 ) ) ;
#22284 = DIRECTION ( 'NONE',  ( -1.000000000000000000, -0.000000000000000000, -0.000000000000000000 ) ) ;
#22285 = DIRECTION ( 'NONE',  ( -1.586032892321652236E-16, -1.000000000000000000, -6.853681917100419162E-49 ) ) ;
#22286 = ORIENTED_EDGE ( 'NONE', *, *, #38113, .F. ) ;
#22287 = LINE ( 'NONE', #34108, #27612 ) ;
#22288 = LINE ( 'NONE', #23038, #31084 ) ;
#22289 = EDGE_LOOP ( 'NONE', ( #38551, #37330, #35474, #45264 ) ) ;
#22290 = ORIENTED_EDGE ( 'NONE', *, *, #50621, .T. ) ;
#22291 = EDGE_LOOP ( 'NONE', ( #36495, #34495, #39904, #43641, #26264, #49388, #11147, #40958, #32514, #26245, #23913, #50298 ) ) ;
#22292 = CARTESIAN_POINT ( 'NONE',  ( -64.99999999999909051, 17.00000000000000000, -24.99999999999999289 ) ) ;
#22293 = LINE ( 'NONE', #6901, #43060 ) ;
#22294 = VERTEX_POINT ( 'NONE', #4717 ) ;
#22295 = CARTESIAN_POINT ( 'NONE',  ( -8.277096487746778308, 50.00000000000000711, 7.455576670931136185 ) ) ;
#22296 =( NAMED_UNIT ( * ) PLANE_ANGLE_UNIT ( ) SI_UNIT ( $, .RADIAN. ) );
#22297 = FACE_BOUND ( 'NONE', #38913, .T. ) ;
#22298 = CARTESIAN_POINT ( 'NONE',  ( -127.7210997126620242, -1.749999999999996669, 41.84341382277508359 ) ) ;
#22299 = ORIENTED_EDGE ( 'NONE', *, *, #8392, .F. ) ;
#22300 = CARTESIAN_POINT ( 'NONE',  ( -15.00000000000001421, 17.00000000000000000, -114.9999999999999858 ) ) ;
#22301 = AXIS2_PLACEMENT_3D ( 'NONE', #29127, #44749, #5768 ) ;
#22302 = ADVANCED_FACE ( 'NONE', ( #9070 ), #39883, .F. ) ;
#22303 = CARTESIAN_POINT ( 'NONE',  ( 30.00000000000153833, 17.00000000000000000, 35.00000000000000000 ) ) ;
#22304 = ORIENTED_EDGE ( 'NONE', *, *, #35606, .F. ) ;
#22305 = CARTESIAN_POINT ( 'NONE',  ( 50.24128791297869867, 41.04536285977714982, -5.000000000000000000 ) ) ;
#22306 = CARTESIAN_POINT ( 'NONE',  ( 210.0000000000000568, 0.000000000000000000, 82.56828755692799859 ) ) ;
#22307 = CIRCLE ( 'NONE', #6741, 1.750000000000008438 ) ;
#22308 = CARTESIAN_POINT ( 'NONE',  ( 6.000000000000000888, 7.347880794884120722E-16, 5.000000000000000000 ) ) ;
#22309 = DIRECTION ( 'NONE',  ( 0.000000000000000000, 0.000000000000000000, 1.000000000000000000 ) ) ;
#22310 = VERTEX_POINT ( 'NONE', #12904 ) ;
#22311 = DIRECTION ( 'NONE',  ( 1.000000000000000000, 0.000000000000000000, 0.000000000000000000 ) ) ;
#22312 = DIRECTION ( 'NONE',  ( 0.000000000000000000, 0.000000000000000000, 1.000000000000000000 ) ) ;
#22313 = CARTESIAN_POINT ( 'NONE',  ( 1.437255894074055185, -3.713052624461447682, -1.301042606982605321E-15 ) ) ;
#22314 = CARTESIAN_POINT ( 'NONE',  ( 72.27890028733797578, 1.750000000000009548, 161.8434138227750907 ) ) ;
#22315 = CARTESIAN_POINT ( 'NONE',  ( 183.0000000000000000, -164.9999999999999432, 343.9999999999998863 ) ) ;
#22316 = ORIENTED_EDGE ( 'NONE', *, *, #45625, .T. ) ;
#22317 =( LENGTH_UNIT ( ) NAMED_UNIT ( * ) SI_UNIT ( .MILLI., .METRE. ) );
#22318 = ORIENTED_EDGE ( 'NONE', *, *, #3846, .T. ) ;
#22319 = LINE ( 'NONE', #49727, #44203 ) ;
#22320 = MANIFOLD_SOLID_BREP ( 'Fillet1', #39230 ) ;
#22321 =( BOUNDED_CURVE ( )  B_SPLINE_CURVE ( 3, ( #3365, #19011, #40553, #1558 ),
 .UNSPECIFIED., .F., .F. ) 
 B_SPLINE_CURVE_WITH_KNOTS ( ( 4, 4 ),
 ( 3.141592653589793116, 4.712388980384689674 ),
 .UNSPECIFIED. ) 
 CURVE ( )  GEOMETRIC_REPRESENTATION_ITEM ( )  RATIONAL_B_SPLINE_CURVE ( ( 1.000000000000000000, 0.8047378541243649375, 0.8047378541243649375, 1.000000000000000000 ) ) 
 REPRESENTATION_ITEM ( '' )  );
#22322 = ORIENTED_EDGE ( 'NONE', *, *, #13266, .F. ) ;
#22323 = PLANE ( 'NONE',  #10658 ) ;
#22324 = FACE_OUTER_BOUND ( 'NONE', #48618, .T. ) ;
#22325 = VECTOR ( 'NONE', #44229, 1000.000000000000000 ) ;
#22326 = EDGE_LOOP ( 'NONE', ( #35611, #49086, #8168, #47366 ) ) ;
#22327 = EDGE_LOOP ( 'NONE', ( #23453, #38338, #45116, #3696, #32306 ) ) ;
#22328 = FACE_OUTER_BOUND ( 'NONE', #2707, .T. ) ;
#22329 = ORIENTED_EDGE ( 'NONE', *, *, #34146, .T. ) ;
#22330 = CARTESIAN_POINT ( 'NONE',  ( 73.30402655318508209, -1.750000000000010214, -39.18171244307202983 ) ) ;
#22331 = LINE ( 'NONE', #2824, #10944 ) ;
#22332 = CARTESIAN_POINT ( 'NONE',  ( -44.94597344681493922, 2.143131898507880377E-16, 2.568287556927978166 ) ) ;
#22333 = CARTESIAN_POINT ( 'NONE',  ( -87.72109971266203843, -1.750000000000010214, -118.1565861772249519 ) ) ;
#22334 = CIRCLE ( 'NONE', #201, 1.750000000000008438 ) ;
#22335 = LINE ( 'NONE', #15150, #3613 ) ;
#22336 = ORIENTED_EDGE ( 'NONE', *, *, #37492, .T. ) ;
#22337 = ORIENTED_EDGE ( 'NONE', *, *, #36641, .F. ) ;
#22338 = DIRECTION ( 'NONE',  ( -1.860490536778032451E-50, 0.000000000000000000, 1.000000000000000000 ) ) ;
#22339 = VECTOR ( 'NONE', #19476, 1000.000000000000000 ) ;
#22340 = ORIENTED_EDGE ( 'NONE', *, *, #46642, .T. ) ;
#22341 = CIRCLE ( 'NONE', #250, 2.000000000000001776 ) ;
#22342 = CARTESIAN_POINT ( 'NONE',  ( 196.8526953830863135, 160.1880105690400171, 472.8425600500171981 ) ) ;
#22343 = LINE ( 'NONE', #26956, #37118 ) ;
#22344 = ORIENTED_EDGE ( 'NONE', *, *, #15529, .T. ) ;
#22345 = LINE ( 'NONE', #30066, #21294 ) ;
#22346 = DIRECTION ( 'NONE',  ( -1.000000000000000000, -0.000000000000000000, -0.000000000000000000 ) ) ;
#22347 = B_SPLINE_SURFACE_WITH_KNOTS ( 'NONE', 3, 3, ( 
 ( #508, #39508, #46894, #39761 ),
 ( #24109, #4349, #47390, #19987 ),
 ( #16149, #32058, #19738, #11792 ),
 ( #8713, #43081, #27442, #19474 ) ),
 .UNSPECIFIED., .F., .F., .F.,
 ( 4, 4 ),
 ( 4, 4 ),
 ( 0.000000000000000000, 1.000000000000000000 ),
 ( 0.000000000000000000, 1.000000000000000000 ),
 .UNSPECIFIED. ) ;
#22348 = ORIENTED_EDGE ( 'NONE', *, *, #50105, .T. ) ;
#22349 = CYLINDRICAL_SURFACE ( 'NONE', #4607, 1.750000000000015543 ) ;
#22350 = CARTESIAN_POINT ( 'NONE',  ( 11.73320209285708415, -11.96063479729170886, 9.403735324607438884 ) ) ;
#22351 = DIRECTION ( 'NONE',  ( 1.000000000000000000, 0.000000000000000000, 0.000000000000000000 ) ) ;
#22352 = DIRECTION ( 'NONE',  ( 1.000000000000000000, -4.758098676964954489E-16, 2.958228394578795584E-31 ) ) ;
#22353 = EDGE_CURVE ( 'NONE', #14100, #11215, #15323, .T. ) ;
#22354 = ORIENTED_EDGE ( 'NONE', *, *, #24038, .F. ) ;
#22355 =( BOUNDED_CURVE ( )  B_SPLINE_CURVE ( 3, ( #16327, #8133, #20167, #35595 ),
 .UNSPECIFIED., .F., .F. ) 
 B_SPLINE_CURVE_WITH_KNOTS ( ( 4, 4 ),
 ( 4.712388980384689674, 6.283185307179586232 ),
 .UNSPECIFIED. ) 
 CURVE ( )  GEOMETRIC_REPRESENTATION_ITEM ( )  RATIONAL_B_SPLINE_CURVE ( ( 1.000000000000000000, 0.8047378541243649375, 0.8047378541243649375, 1.000000000000000000 ) ) 
 REPRESENTATION_ITEM ( '' )  );
#22356 = ORIENTED_EDGE ( 'NONE', *, *, #40715, .F. ) ;
#22357 = EDGE_CURVE ( 'NONE', #37670, #34164, #35794, .T. ) ;
#22358 = DIRECTION ( 'NONE',  ( -0.000000000000000000, -1.000000000000000000, 2.537652627714643577E-15 ) ) ;
#22359 = ORIENTED_EDGE ( 'NONE', *, *, #47440, .T. ) ;
#22360 = EDGE_CURVE ( 'NONE', #15143, #21583, #8212, .T. ) ;
#22361 = ORIENTED_EDGE ( 'NONE', *, *, #32411, .T. ) ;
#22362 = DIRECTION ( 'NONE',  ( -1.745740669421566678E-14, 1.462853032738780738E-28, -1.000000000000000000 ) ) ;
#22363 = EDGE_CURVE ( 'NONE', #21950, #48177, #13163, .T. ) ;
#22364 = CARTESIAN_POINT ( 'NONE',  ( -124.9459734468149463, 2.143131898507847836E-16, 159.0682875569279702 ) ) ;
#22365 = CARTESIAN_POINT ( 'NONE',  ( 2.322372356066598531, 2.286285436021770145, 9.799352050262459812 ) ) ;
#22366 = CARTESIAN_POINT ( 'NONE',  ( -12.78770032058971395, -31.68259716188267916, 7.455576670931136185 ) ) ;
#22367 = DIRECTION ( 'NONE',  ( 0.000000000000000000, 0.000000000000000000, 1.000000000000000000 ) ) ;
#22368 = VECTOR ( 'NONE', #10969, 1000.000000000000000 ) ;
#22369 = CARTESIAN_POINT ( 'NONE',  ( 356.0000000000000000, -165.0000000000001137, 339.9999999999999432 ) ) ;
#22370 = CARTESIAN_POINT ( 'NONE',  ( 35.00000000000091660, 16.00000000000000000, -24.99999999999999289 ) ) ;
#22371 = VERTEX_POINT ( 'NONE', #36289 ) ;
#22372 = CARTESIAN_POINT ( 'NONE',  ( 75.05402655318509630, -1.025126265847089435, 39.06828755692797728 ) ) ;
#22373 = VECTOR ( 'NONE', #1253, 1000.000000000000000 ) ;
#22374 = ADVANCED_FACE ( 'NONE', ( #1128 ), #9318, .F. ) ;
#22375 = LINE ( 'NONE', #38311, #33532 ) ;
#22376 = CARTESIAN_POINT ( 'NONE',  ( -1.228394325311288560, 1.341866297401936636, 9.903764339332077782 ) ) ;
#22377 = AXIS2_PLACEMENT_3D ( 'NONE', #48650, #24609, #40255 ) ;
#22378 = SURFACE_STYLE_USAGE ( .BOTH. , #50288 ) ;
#22379 = VERTEX_POINT ( 'NONE', #40375 ) ;
#22380 = AXIS2_PLACEMENT_3D ( 'NONE', #31358, #46949, #11850 ) ;
#22381 = CARTESIAN_POINT ( 'NONE',  ( 166.9999999999999716, 6.000000000000060396, -350.0000000000001705 ) ) ;
#22382 = EDGE_LOOP ( 'NONE', ( #2250, #15219, #6261, #31970, #46862 ) ) ;
#22383 = DIRECTION ( 'NONE',  ( 0.000000000000000000, -0.000000000000000000, -1.000000000000000000 ) ) ;
#22384 = DIRECTION ( 'NONE',  ( 0.000000000000000000, 0.000000000000000000, 1.000000000000000000 ) ) ;
#22385 = EDGE_CURVE ( 'NONE', #33144, #3012, #47525, .T. ) ;
#22386 = CARTESIAN_POINT ( 'NONE',  ( 1.011271242968677653, 0.7347315653656002477, -10.00000000000000000 ) ) ;
#22387 = EDGE_CURVE ( 'NONE', #29044, #7807, #24979, .T. ) ;
#22388 = ORIENTED_EDGE ( 'NONE', *, *, #45597, .F. ) ;
#22389 = EDGE_CURVE ( 'NONE', #27616, #27480, #31928, .T. ) ;
#22390 = EDGE_CURVE ( 'NONE', #42553, #23855, #14788, .T. ) ;
#22391 = CARTESIAN_POINT ( 'NONE',  ( -164.9999999999990905, 17.00000000000000000, 0.000000000000000000 ) ) ;
#22392 = VERTEX_POINT ( 'NONE', #8570 ) ;
#22393 = LINE ( 'NONE', #30877, #36145 ) ;
#22394 = CARTESIAN_POINT ( 'NONE',  ( -164.9459734468149463, 2.143131898507880377E-16, 122.5682875569279702 ) ) ;
#22395 = ADVANCED_FACE ( 'NONE', ( #14425 ), #1876, .F. ) ;
#22396 = CARTESIAN_POINT ( 'NONE',  ( -4.945973446814938335, 0.000000000000000000, 162.5682875569279702 ) ) ;
#22397 = ADVANCED_FACE ( 'NONE', ( #5462 ), #21112, .T. ) ;
#22398 = ORIENTED_EDGE ( 'NONE', *, *, #16460, .T. ) ;
#22399 = ORIENTED_EDGE ( 'NONE', *, *, #15184, .T. ) ;
#22400 = CARTESIAN_POINT ( 'NONE',  ( -6.174150299305392053, 50.00000000000000000, 8.807470649214879543 ) ) ;
#22401 = CARTESIAN_POINT ( 'NONE',  ( 0.4384698884932147211, 1.388183145050263745, 9.938560701278168708 ) ) ;
#22402 = ORIENTED_EDGE ( 'NONE', *, *, #4528, .T. ) ;
#22403 = ORIENTED_EDGE ( 'NONE', *, *, #46187, .F. ) ;
#22404 = CARTESIAN_POINT ( 'NONE',  ( -14.49999999999999822, 12.98684210526315930, 19.87312575500899925 ) ) ;
#22405 = FACE_OUTER_BOUND ( 'NONE', #13042, .T. ) ;
#22406 = CYLINDRICAL_SURFACE ( 'NONE', #33008, 3.749999999999975575 ) ;
#22407 = ORIENTED_EDGE ( 'NONE', *, *, #28379, .F. ) ;
#22408 = FACE_OUTER_BOUND ( 'NONE', #50069, .T. ) ;
#22409 = ORIENTED_EDGE ( 'NONE', *, *, #21239, .F. ) ;
#22410 = ADVANCED_FACE ( 'NONE', ( #18255 ), #17774, .T. ) ;
#22411 = AXIS2_PLACEMENT_3D ( 'NONE', #8526, #27765, #36239 ) ;
#22412 = CARTESIAN_POINT ( 'NONE',  ( 9.358026734184097251, 0.000000000000000000, 22.00000000000000000 ) ) ;
#22413 =( BOUNDED_CURVE ( )  B_SPLINE_CURVE ( 3, ( #44171, #24702, #23931, #40347 ),
 .UNSPECIFIED., .F., .F. ) 
 B_SPLINE_CURVE_WITH_KNOTS ( ( 4, 4 ),
 ( 4.712388980384689674, 6.283185307179586232 ),
 .UNSPECIFIED. ) 
 CURVE ( )  GEOMETRIC_REPRESENTATION_ITEM ( )  RATIONAL_B_SPLINE_CURVE ( ( 1.000000000000000000, 0.8047378541243649375, 0.8047378541243649375, 1.000000000000000000 ) ) 
 REPRESENTATION_ITEM ( '' )  );
#22414 = DIRECTION ( 'NONE',  ( 0.000000000000000000, -0.3846153846153845812, -0.9230769230769231282 ) ) ;
#22415 = EDGE_CURVE ( 'NONE', #1107, #32259, #49523, .T. ) ;
#22416 = ORIENTED_EDGE ( 'NONE', *, *, #189, .F. ) ;
#22417 = ADVANCED_FACE ( 'NONE', ( #13901 ), #29072, .T. ) ;
#22418 = EDGE_LOOP ( 'NONE', ( #20873, #13066, #37302, #40080 ) ) ;
#22419 = ORIENTED_EDGE ( 'NONE', *, *, #5158, .F. ) ;
#22420 =( BOUNDED_CURVE ( )  B_SPLINE_CURVE ( 3, ( #49337, #29888, #37864, #14490 ),
 .UNSPECIFIED., .F., .F. ) 
 B_SPLINE_CURVE_WITH_KNOTS ( ( 4, 4 ),
 ( 3.141592653589793116, 4.712388980384689674 ),
 .UNSPECIFIED. ) 
 CURVE ( )  GEOMETRIC_REPRESENTATION_ITEM ( )  RATIONAL_B_SPLINE_CURVE ( ( 1.000000000000000000, 0.8047378541243649375, 0.8047378541243649375, 1.000000000000000000 ) ) 
 REPRESENTATION_ITEM ( '' )  );
#22421 = CARTESIAN_POINT ( 'NONE',  ( 154.3291528190321458, 1.750000000000009548, -0.2068387089191121020 ) ) ;
#22422 = ORIENTED_EDGE ( 'NONE', *, *, #45901, .T. ) ;
#22423 = DIRECTION ( 'NONE',  ( 1.000000000000000000, 0.000000000000000000, 0.000000000000000000 ) ) ;
#22424 = ORIENTED_EDGE ( 'NONE', *, *, #17702, .F. ) ;
#22425 = EDGE_CURVE ( 'NONE', #24712, #28277, #25854, .T. ) ;
#22426 = DIRECTION ( 'NONE',  ( -1.000000000000000000, 0.000000000000000000, 0.000000000000000000 ) ) ;
#22427 = ORIENTED_EDGE ( 'NONE', *, *, #6548, .F. ) ;
#22428 = CARTESIAN_POINT ( 'NONE',  ( 1.011271242968683648, 0.7347315653655930312, 10.00000000000000000 ) ) ;
#22429 = CARTESIAN_POINT ( 'NONE',  ( -168.4459734468149747, -1.025126265847089435, -40.93171244307204404 ) ) ;
#22430 = CARTESIAN_POINT ( 'NONE',  ( -7.241383964640739634, -3.469446951953614189E-15, 5.000000000000000000 ) ) ;
#22431 = DIRECTION ( 'NONE',  ( -0.000000000000000000, -0.000000000000000000, 1.000000000000000000 ) ) ;
#22432 = VECTOR ( 'NONE', #24015, 1000.000000000000000 ) ;
#22433 = DIRECTION ( 'NONE',  ( 0.000000000000000000, -1.000000000000000000, 2.537652627714642000E-15 ) ) ;
#22434 = ORIENTED_EDGE ( 'NONE', *, *, #7955, .F. ) ;
#22435 = DIRECTION ( 'NONE',  ( 0.000000000000000000, -0.000000000000000000, -1.000000000000000000 ) ) ;
#22436 = DIRECTION ( 'NONE',  ( 0.000000000000000000, 1.000000000000000000, 0.000000000000000000 ) ) ;
#22437 = DIRECTION ( 'NONE',  ( 0.000000000000000000, -0.000000000000000000, -1.000000000000000000 ) ) ;
#22438 = CARTESIAN_POINT ( 'NONE',  ( 71.55402655318505367, 1.025126265847089213, -37.43171244307202272 ) ) ;
#22439 = EDGE_CURVE ( 'NONE', #1904, #4802, #30088, .T. ) ;
#22440 = DIRECTION ( 'NONE',  ( 1.000000000000000000, 0.000000000000000000, 0.000000000000000000 ) ) ;
#22441 = VECTOR ( 'NONE', #29476, 1000.000000000000000 ) ;
#22442 = VECTOR ( 'NONE', #25564, 1000.000000000000000 ) ;
#22443 = EDGE_CURVE ( 'NONE', #29288, #15030, #5974, .T. ) ;
#22444 = LINE ( 'NONE', #2931, #29420 ) ;
#22445 = VECTOR ( 'NONE', #40752, 1000.000000000000000 ) ;
#22446 = FACE_OUTER_BOUND ( 'NONE', #46744, .T. ) ;
#22447 = FACE_OUTER_BOUND ( 'NONE', #1840, .T. ) ;
#22448 = AXIS2_PLACEMENT_3D ( 'NONE', #33018, #13238, #29161 ) ;
#22449 = VERTEX_POINT ( 'NONE', #45689 ) ;
#22450 = CARTESIAN_POINT ( 'NONE',  ( -0.3370904143228978245, 0.2449105217885259589, -10.00000000000000000 ) ) ;
#22451 = EDGE_CURVE ( 'NONE', #50718, #1522, #16845, .T. ) ;
#22452 = ADVANCED_FACE ( 'NONE', ( #9572 ), #5964, .T. ) ;
#22453 = CARTESIAN_POINT ( 'NONE',  ( -165.6708471809677974, -1.750000000000009548, 41.84341382277508359 ) ) ;
#22454 = LINE ( 'NONE', #2207, #30277 ) ;
#22455 = CARTESIAN_POINT ( 'NONE',  ( 12.15085308559846844, -11.68662139125803989, 2.590526750877053086 ) ) ;
#22456 = CARTESIAN_POINT ( 'NONE',  ( -8.445973446814964092, 1.025126265847097207, -40.93171244307204404 ) ) ;
#22457 = ADVANCED_FACE ( 'NONE', ( #33686 ), #37049, .T. ) ;
#22458 = VERTEX_POINT ( 'NONE', #26231 ) ;
#22459 = B_SPLINE_SURFACE_WITH_KNOTS ( 'NONE', 3, 3, ( 
 ( #10751, #30513, #15116, #18191 ),
 ( #33872, #14352, #6912, #49459 ),
 ( #50204, #46386, #30020, #14602 ),
 ( #34891, #26913, #7168, #42310 ) ),
 .UNSPECIFIED., .F., .F., .F.,
 ( 4, 4 ),
 ( 4, 4 ),
 ( 0.000000000000000000, 1.000000000000000000 ),
 ( 0.000000000000000000, 1.000000000000000000 ),
 .UNSPECIFIED. ) ;
#22460 = ORIENTED_EDGE ( 'NONE', *, *, #43989, .F. ) ;
#22461 = CARTESIAN_POINT ( 'NONE',  ( -15.00199999999999712, -34.54492135858216528, -5.000000000000000000 ) ) ;
#22462 = EDGE_CURVE ( 'NONE', #37651, #12891, #32941, .T. ) ;
#22463 = CARTESIAN_POINT ( 'NONE',  ( -176.3085477938156487, -62.49999999999998579, -19.92876838486919411 ) ) ;
#22464 = ADVANCED_FACE ( 'NONE', ( #25986 ), #25730, .F. ) ;
#22465 = AXIS2_PLACEMENT_3D ( 'NONE', #31739, #47327, #27880 ) ;
#22466 = ORIENTED_EDGE ( 'NONE', *, *, #4921, .F. ) ;
#22467 = LINE ( 'NONE', #38140, #35266 ) ;
#22468 = CARTESIAN_POINT ( 'NONE',  ( 181.0000000000000000, -174.9999999999999716, -342.0000000000001137 ) ) ;
#22469 = CARTESIAN_POINT ( 'NONE',  ( -0.4166666666666664631, 0.000000000000000000, 10.00000000000000000 ) ) ;
#22470 = ORIENTED_EDGE ( 'NONE', *, *, #42843, .F. ) ;
#22471 = ORIENTED_EDGE ( 'NONE', *, *, #24322, .F. ) ;
#22472 = EDGE_LOOP ( 'NONE', ( #44391, #21792, #12067, #48910, #16881 ) ) ;
#22473 = FACE_OUTER_BOUND ( 'NONE', #10161, .T. ) ;
#22474 = PLANE ( 'NONE',  #475 ) ;
#22475 = CARTESIAN_POINT ( 'NONE',  ( 8.831420117243668599, 14.12636088103192655, -3.546734833711462365 ) ) ;
#22476 = VERTEX_POINT ( 'NONE', #48778 ) ;
#22477 = CARTESIAN_POINT ( 'NONE',  ( 210.0000000000000568, 0.000000000000000000, -79.18171244307201562 ) ) ;
#22478 = ADVANCED_FACE ( 'NONE', ( #13668 ), #44934, .T. ) ;
#22479 = CARTESIAN_POINT ( 'NONE',  ( 358.0000000000000568, 167.8284271247464972, 342.8284271247462129 ) ) ;
#22480 = CARTESIAN_POINT ( 'NONE',  ( 1.540526284687965264, -1.371707213411490267, 9.886433018048071730 ) ) ;
#22481 = ORIENTED_EDGE ( 'NONE', *, *, #42831, .F. ) ;
#22482 = ORIENTED_EDGE ( 'NONE', *, *, #30061, .F. ) ;
#22483 = DIRECTION ( 'NONE',  ( -1.000000000000000000, -0.000000000000000000, -0.000000000000000000 ) ) ;
#22484 = CARTESIAN_POINT ( 'NONE',  ( 1.111507796622770883, 1.112188257001374581, 9.945241992664893615 ) ) ;
#22485 = LINE ( 'NONE', #9926, #32427 ) ;
#22486 = ORIENTED_EDGE ( 'NONE', *, *, #43264, .F. ) ;
#22487 = ORIENTED_EDGE ( 'NONE', *, *, #17354, .F. ) ;
#22488 = AXIS2_PLACEMENT_3D ( 'NONE', #15670, #15169, #20024 ) ;
#22489 = CARTESIAN_POINT ( 'NONE',  ( -4.945973446814903696, 2.143131898507912917E-16, -37.43171244307200141 ) ) ;
#22490 = FACE_BOUND ( 'NONE', #31319, .T. ) ;
#22491 = DIRECTION ( 'NONE',  ( 1.000000000000000000, 0.000000000000000000, 0.000000000000000000 ) ) ;
#22492 = CARTESIAN_POINT ( 'NONE',  ( 350.0000000000001137, 181.0000000000000284, 339.9999999999997726 ) ) ;
#22493 = MANIFOLD_SOLID_BREP ( 'Square tube 20 X 20 X 2(1)[1]', #31872 ) ;
#22494 = LINE ( 'NONE', #45306, #8569 ) ;
#22495 = ORIENTED_EDGE ( 'NONE', *, *, #1171, .T. ) ;
#22496 = DIRECTION ( 'NONE',  ( 0.000000000000000000, -1.000000000000000000, 0.000000000000000000 ) ) ;
#22497 = CARTESIAN_POINT ( 'NONE',  ( -124.9459734468149463, 2.143131898507847836E-16, -160.9317124430720014 ) ) ;
#22498 = CARTESIAN_POINT ( 'NONE',  ( -48.44597344681495343, 0.000000000000000000, -80.93171244307204404 ) ) ;
#22499 = CYLINDRICAL_SURFACE ( 'NONE', #29611, 1.750000000000015543 ) ;
#22500 = CYLINDRICAL_SURFACE ( 'NONE', #49433, 1.750000000000036193 ) ;
#22501 = ORIENTED_EDGE ( 'NONE', *, *, #5454, .F. ) ;
#22502 = CARTESIAN_POINT ( 'NONE',  ( 7.576114424932982594, -33.14742743729794938, 7.906207997025717304 ) ) ;
#22503 = LINE ( 'NONE', #14037, #37342 ) ;
#22504 = LINE ( 'NONE', #22760, #8269 ) ;
#22505 = ORIENTED_EDGE ( 'NONE', *, *, #38200, .F. ) ;
#22506 = EDGE_CURVE ( 'NONE', #41895, #41913, #50277, .T. ) ;
#22507 = EDGE_CURVE ( 'NONE', #42464, #29500, #27548, .T. ) ;
#22508 = CARTESIAN_POINT ( 'NONE',  ( 181.0000000000000284, 2.775557561562891351E-14, -113.0000000000001563 ) ) ;
#22509 = VECTOR ( 'NONE', #48869, 1000.000000000000000 ) ;
#22510 = VERTEX_POINT ( 'NONE', #19014 ) ;
#22511 = CARTESIAN_POINT ( 'NONE',  ( -47.72109971266203132, -1.750000000000009548, 39.79316129108089228 ) ) ;
#22512 = DIRECTION ( 'NONE',  ( 0.000000000000000000, 0.000000000000000000, 1.000000000000000000 ) ) ;
#22513 = CARTESIAN_POINT ( 'NONE',  ( 31.55402655318503236, 1.025126265847089213, -37.43171244307202272 ) ) ;
#22514 = CYLINDRICAL_SURFACE ( 'NONE', #8638, 1.750000000000008438 ) ;
#22515 = EDGE_CURVE ( 'NONE', #9965, #19479, #42114, .T. ) ;
#22516 = ORIENTED_EDGE ( 'NONE', *, *, #20317, .F. ) ;
#22517 = VERTEX_POINT ( 'NONE', #19273 ) ;
#22518 = ORIENTED_EDGE ( 'NONE', *, *, #14345, .F. ) ;
#22519 = VECTOR ( 'NONE', #2671, 1000.000000000000000 ) ;
#22520 = ADVANCED_FACE ( 'NONE', ( #30849 ), #15685, .F. ) ;
#22521 = FACE_OUTER_BOUND ( 'NONE', #12750, .T. ) ;
#22522 = ADVANCED_FACE ( 'NONE', ( #50531 ), #10823, .T. ) ;
#22523 = EDGE_LOOP ( 'NONE', ( #14618, #31493, #29084, #22214, #23981, #49138 ) ) ;
#22524 = CYLINDRICAL_SURFACE ( 'NONE', #14727, 2.000000000000001776 ) ;
#22525 = CYLINDRICAL_SURFACE ( 'NONE', #11837, 6.000000000000000888 ) ;
#22526 = CARTESIAN_POINT ( 'NONE',  ( -50.00000000000000000, 0.000000000000000000, 900.0000000000000000 ) ) ;
#22527 = EDGE_CURVE ( 'NONE', #40407, #15139, #26477, .T. ) ;
#22528 = DIRECTION ( 'NONE',  ( 0.000000000000000000, -0.000000000000000000, -1.000000000000000000 ) ) ;
#22529 = VERTEX_POINT ( 'NONE', #42619 ) ;
#22530 = LINE ( 'NONE', #6131, #3471 ) ;
#22531 = DIRECTION ( 'NONE',  ( -1.000000000000000000, 0.000000000000000000, 0.000000000000000000 ) ) ;
#22532 = DIRECTION ( 'NONE',  ( -0.000000000000000000, -1.000000000000000000, -0.000000000000000000 ) ) ;
#22533 = CARTESIAN_POINT ( 'NONE',  ( 130.0000000000021032, 16.00000000000000000, 115.0000000000000142 ) ) ;
#22534 = AXIS2_PLACEMENT_3D ( 'NONE', #10154, #41709, #29908 ) ;
#22535 = ORIENTED_EDGE ( 'NONE', *, *, #17336, .T. ) ;
#22536 = DIRECTION ( 'NONE',  ( -1.000000000000000000, -0.000000000000000000, -0.000000000000000000 ) ) ;
#22537 = DIRECTION ( 'NONE',  ( -1.000000000000000000, 0.000000000000000000, 0.000000000000000000 ) ) ;
#22538 = EDGE_LOOP ( 'NONE', ( #45905, #30235, #35615, #9509 ) ) ;
#22539 = VECTOR ( 'NONE', #38502, 1000.000000000000000 ) ;
#22540 = VERTEX_POINT ( 'NONE', #3116 ) ;
#22541 = VERTEX_POINT ( 'NONE', #11078 ) ;
#22542 = LINE ( 'NONE', #14846, #881 ) ;
#22543 = CARTESIAN_POINT ( 'NONE',  ( 30.67467450244491900, -28.55398182363552806, 7.544061037322998153 ) ) ;
#22544 = ORIENTED_EDGE ( 'NONE', *, *, #4965, .F. ) ;
#22545 = DIRECTION ( 'NONE',  ( 1.000000000000000000, 0.000000000000000000, -1.860490536778032451E-50 ) ) ;
#22546 = FACE_BOUND ( 'NONE', #8846, .T. ) ;
#22547 = CARTESIAN_POINT ( 'NONE',  ( -178.1763882397830798, 47.50000000000000000, -120.5992382549688955 ) ) ;
#22548 = CARTESIAN_POINT ( 'NONE',  ( -215.0000000000000568, 0.000000000000000000, 10.00000000000000000 ) ) ;
#22549 = AXIS2_PLACEMENT_3D ( 'NONE', #47264, #11907, #47521 ) ;
#22550 = CIRCLE ( 'NONE', #26665, 2.000000000000001776 ) ;
#22551 = CARTESIAN_POINT ( 'NONE',  ( 28.55116071645549525, -41.05976639056858346, -2.408242355805840784 ) ) ;
#22552 = CARTESIAN_POINT ( 'NONE',  ( 1.042245359060418375, 0.7067879234688301260, 9.974012008644017158 ) ) ;
#22553 = PRODUCT_DEFINITION_FORMATION_WITH_SPECIFIED_SOURCE ( 'ANY', '', #1545, .NOT_KNOWN. ) ;
#22554 = EDGE_CURVE ( 'NONE', #38131, #48818, #18763, .T. ) ;
#22555 = ORIENTED_EDGE ( 'NONE', *, *, #25946, .T. ) ;
#22556 = ITEM_DEFINED_TRANSFORMATION ( 'NONE', 'NONE', #16022,  #45486 ) ;
#22557 = PLANE ( 'NONE',  #47799 ) ;
#22558 =( BOUNDED_CURVE ( )  B_SPLINE_CURVE ( 3, ( #9768, #10031, #10782, #26432 ),
 .UNSPECIFIED., .F., .F. ) 
 B_SPLINE_CURVE_WITH_KNOTS ( ( 4, 4 ),
 ( 1.570796326794896558, 3.141592653589793116 ),
 .UNSPECIFIED. ) 
 CURVE ( )  GEOMETRIC_REPRESENTATION_ITEM ( )  RATIONAL_B_SPLINE_CURVE ( ( 1.000000000000000000, 0.8047378541243649375, 0.8047378541243649375, 1.000000000000000000 ) ) 
 REPRESENTATION_ITEM ( '' )  );
#22559 = CARTESIAN_POINT ( 'NONE',  ( 31.46770792452135268, -38.94077080897339727, 3.199614146704519602 ) ) ;
#22560 = CARTESIAN_POINT ( 'NONE',  ( 111.5540265531850679, 0.000000000000000000, 2.568287556927950632 ) ) ;
#22561 = DIRECTION ( 'NONE',  ( -1.000000000000000000, -0.000000000000000000, -0.000000000000000000 ) ) ;
#22562 = ORIENTED_EDGE ( 'NONE', *, *, #24874, .F. ) ;
#22563 = CARTESIAN_POINT ( 'NONE',  ( -164.9459734468149463, 2.143131898507880377E-16, 119.0682875569279702 ) ) ;
#22564 = CYLINDRICAL_SURFACE ( 'NONE', #49873, 4.000000000000003553 ) ;
#22565 =( BOUNDED_CURVE ( )  B_SPLINE_CURVE ( 3, ( #5648, #5398, #17711, #13836 ),
 .UNSPECIFIED., .F., .F. ) 
 B_SPLINE_CURVE_WITH_KNOTS ( ( 4, 4 ),
 ( 4.712388980384689674, 6.283185307179253165 ),
 .UNSPECIFIED. ) 
 CURVE ( )  GEOMETRIC_REPRESENTATION_ITEM ( )  RATIONAL_B_SPLINE_CURVE ( ( 1.000000000000000000, 0.8047378541243649375, 0.8047378541243649375, 1.000000000000000000 ) ) 
 REPRESENTATION_ITEM ( '' )  );
#22566 = CARTESIAN_POINT ( 'NONE',  ( 214.9999999999999432, 164.9999999999999716, 231.9999999999999716 ) ) ;
#22567 = DIRECTION ( 'NONE',  ( 0.000000000000000000, -2.265761274745217480E-16, 1.000000000000000000 ) ) ;
#22568 = DIRECTION ( 'NONE',  ( 0.000000000000000000, 0.000000000000000000, -1.000000000000000000 ) ) ;
#22569 = EDGE_LOOP ( 'NONE', ( #4550, #9566, #32561, #32247 ) ) ;
#22570 = AXIS2_PLACEMENT_3D ( 'NONE', #50563, #34733, #26761 ) ;
#22571 = LINE ( 'NONE', #34907, #7590 ) ;
#22572 = VERTEX_POINT ( 'NONE', #50021 ) ;
#22573 = CARTESIAN_POINT ( 'NONE',  ( -6.174150299305392053, 33.14591993373988998, 8.807470649214879543 ) ) ;
#22574 = MANIFOLD_SOLID_BREP ( 'Scale1', #16289 ) ;
#22575 = VECTOR ( 'NONE', #14718, 1000.000000000000000 ) ;
#22576 = ORIENTED_EDGE ( 'NONE', *, *, #40015, .T. ) ;
#22577 = DIRECTION ( 'NONE',  ( 0.000000000000000000, 0.000000000000000000, -1.000000000000000000 ) ) ;
#22578 = DIRECTION ( 'NONE',  ( 0.000000000000000000, 2.969158215481698263E-48, -1.000000000000000000 ) ) ;
#22579 = AXIS2_PLACEMENT_3D ( 'NONE', #28256, #43887, #20790 ) ;
#22580 =( BOUNDED_CURVE ( )  B_SPLINE_CURVE ( 3, ( #2656, #35013, #26525, #42159 ),
 .UNSPECIFIED., .F., .F. ) 
 B_SPLINE_CURVE_WITH_KNOTS ( ( 4, 4 ),
 ( 4.712388980384689674, 6.283185307179586232 ),
 .UNSPECIFIED. ) 
 CURVE ( )  GEOMETRIC_REPRESENTATION_ITEM ( )  RATIONAL_B_SPLINE_CURVE ( ( 1.000000000000000000, 0.8047378541243649375, 0.8047378541243649375, 1.000000000000000000 ) ) 
 REPRESENTATION_ITEM ( '' )  );
#22581 = VERTEX_POINT ( 'NONE', #35728 ) ;
#22582 = LINE ( 'NONE', #42332, #30595 ) ;
#22583 = VERTEX_POINT ( 'NONE', #47699 ) ;
#22584 = VECTOR ( 'NONE', #11502, 1000.000000000000000 ) ;
#22585 = CARTESIAN_POINT ( 'NONE',  ( -19.99999999999783995, 16.00000000000000000, 95.00000000000000000 ) ) ;
#22586 = EDGE_LOOP ( 'NONE', ( #14814, #46692, #14962, #19364, #9615 ) ) ;
#22587 = CARTESIAN_POINT ( 'NONE',  ( 72.27890028733797578, -1.750000000000009548, -38.15658617722494483 ) ) ;
#22588 = DIRECTION ( 'NONE',  ( 1.000000000000000000, 0.000000000000000000, 1.612977847700450206E-50 ) ) ;
#22589 = AXIS2_PLACEMENT_3D ( 'NONE', #29815, #10323, #28810 ) ;
#22590 = EDGE_LOOP ( 'NONE', ( #31820, #19235, #36180, #43674 ) ) ;
#22591 = CARTESIAN_POINT ( 'NONE',  ( -19.99999999999908695, 17.00000000000000000, 0.000000000000000000 ) ) ;
#22592 = CARTESIAN_POINT ( 'NONE',  ( 5.297170062947166969, 5.958621178614006197, -4.472333961502705790E-16 ) ) ;
#22593 = EDGE_CURVE ( 'NONE', #44023, #25029, #36097, .T. ) ;
#22594 = DIRECTION ( 'NONE',  ( 0.000000000000000000, 0.000000000000000000, -1.000000000000000000 ) ) ;
#22595 = EDGE_LOOP ( 'NONE', ( #30542, #8605, #24066, #47911, #9532, #25366 ) ) ;
#22596 = ORIENTED_EDGE ( 'NONE', *, *, #36676, .T. ) ;
#22597 = B_SPLINE_CURVE_WITH_KNOTS ( 'NONE', 3,
 ( #11571, #30822, #18734, #23103 ),
 .UNSPECIFIED., .F., .F.,
 ( 4, 4 ),
 ( 2.732001163471678047E-18, 0.009782300387714808892 ),
 .UNSPECIFIED. ) ;
#22598 = CARTESIAN_POINT ( 'NONE',  ( -46.69597344681494633, 1.750000000000010658, -79.18171244307201562 ) ) ;
#22599 = VECTOR ( 'NONE', #49887, 1000.000000000000000 ) ;
#22600 = VECTOR ( 'NONE', #12185, 1000.000000000000000 ) ;
#22601 = LINE ( 'NONE', #42590, #12491 ) ;
#22602 = EDGE_LOOP ( 'NONE', ( #7800, #50143, #29483, #7801 ) ) ;
#22603 = CARTESIAN_POINT ( 'NONE',  ( -331.7552636306689351, 248.6897383013407818, 297.1446280767822259 ) ) ;
#22604 = CARTESIAN_POINT ( 'NONE',  ( -22.93339884797946127, 29.71580813607156912, -3.721387749823086732 ) ) ;
#22605 = ORIENTED_EDGE ( 'NONE', *, *, #39809, .T. ) ;
#22606 = CARTESIAN_POINT ( 'NONE',  ( -5.670847180967843570, 1.750000000000023537, -120.2068387089191219 ) ) ;
#22607 = LINE ( 'NONE', #42354, #44765 ) ;
#22608 = ORIENTED_EDGE ( 'NONE', *, *, #34641, .F. ) ;
#22609 = CARTESIAN_POINT ( 'NONE',  ( -208.1473046169136296, 160.1880105690400171, 472.8425600500171981 ) ) ;
#22610 = CARTESIAN_POINT ( 'NONE',  ( 36.08557433729230723, -35.58569447144768105, 7.455576670931136185 ) ) ;
#22611 = DIRECTION ( 'NONE',  ( -1.000000000000000000, 0.000000000000000000, 0.000000000000000000 ) ) ;
#22612 = FACE_BOUND ( 'NONE', #17410, .T. ) ;
#22613 = CIRCLE ( 'NONE', #46350, 0.5000000000000004441 ) ;
#22614 = ORIENTED_EDGE ( 'NONE', *, *, #25235, .F. ) ;
#22615 = CARTESIAN_POINT ( 'NONE',  ( 48.99656738986517723, -11.00747004110342431, 1.847720168420772691 ) ) ;
#22616 = CIRCLE ( 'NONE', #47992, 4.000000000000003553 ) ;
#22617 = CARTESIAN_POINT ( 'NONE',  ( -36.08557433729205144, 35.58569447144795816, 7.455576670931136185 ) ) ;
#22618 = CARTESIAN_POINT ( 'NONE',  ( -0.3904210042914396661, 2.126747006146315844, 9.882710035074776300 ) ) ;
#22619 = ORIENTED_EDGE ( 'NONE', *, *, #29899, .T. ) ;
#22620 = ADVANCED_FACE ( 'NONE', ( #16453 ), #4146, .F. ) ;
#22621 = VERTEX_POINT ( 'NONE', #16690 ) ;
#22622 =( NAMED_UNIT ( * ) PLANE_ANGLE_UNIT ( ) SI_UNIT ( $, .RADIAN. ) );
#22623 = CARTESIAN_POINT ( 'NONE',  ( -124.9459734468149321, -1.025126265847081219, 159.0682875569279418 ) ) ;
#22624 = AXIS2_PLACEMENT_3D ( 'NONE', #7087, #11194, #15033 ) ;
#22625 = CARTESIAN_POINT ( 'NONE',  ( -45.67084718096785423, -1.750000000000009548, 161.8434138227750907 ) ) ;
#22626 = DIRECTION ( 'NONE',  ( 0.000000000000000000, 0.000000000000000000, 1.000000000000000000 ) ) ;
#22627 = CARTESIAN_POINT ( 'NONE',  ( -225.0000000000000568, 164.9999999999999716, 111.9999999999999858 ) ) ;
#22628 = CARTESIAN_POINT ( 'NONE',  ( -5.670847180967843570, -1.750000000000023315, -118.1565861772249519 ) ) ;
#22629 = PRESENTATION_LAYER_ASSIGNMENT (  '', '', ( #20173 ) ) ;
#22630 = CARTESIAN_POINT ( 'NONE',  ( -64.99999999999846523, 17.00000000000000000, 35.00000000000000000 ) ) ;
#22631 = ORIENTED_EDGE ( 'NONE', *, *, #21139, .T. ) ;
#22632 = CARTESIAN_POINT ( 'NONE',  ( 183.0000000000000000, -256.4999999999999432, -349.9999999999999432 ) ) ;
#22633 = CARTESIAN_POINT ( 'NONE',  ( -46.76852358249002606, 17.86468378716741512, -9.367992836599954742 ) ) ;
#22634 = AXIS2_PLACEMENT_3D ( 'NONE', #3856, #43351, #39276 ) ;
#22635 =( LENGTH_UNIT ( ) NAMED_UNIT ( * ) SI_UNIT ( .MILLI., .METRE. ) );
#22636 = ORIENTED_EDGE ( 'NONE', *, *, #33113, .F. ) ;
#22637 = CARTESIAN_POINT ( 'NONE',  ( -24.39427009666018265, -44.07992421011638129, 8.807470649214879543 ) ) ;
#22638 = ORIENTED_EDGE ( 'NONE', *, *, #740, .T. ) ;
#22639 = CARTESIAN_POINT ( 'NONE',  ( 168.9999999999999716, -164.9999999999999432, -344.0000000000001137 ) ) ;
#22640 = DIRECTION ( 'NONE',  ( -0.000000000000000000, -1.000000000000000000, -0.000000000000000000 ) ) ;
#22641 = CARTESIAN_POINT ( 'NONE',  ( 30.00000000000092726, 17.00000000000000000, -24.99999999999999289 ) ) ;
#22642 = ORIENTED_EDGE ( 'NONE', *, *, #21513, .F. ) ;
#22643 = AXIS2_PLACEMENT_3D ( 'NONE', #47933, #47428, #39788 ) ;
#22644 = PLANE ( 'NONE',  #32000 ) ;
#22645 = ORIENTED_EDGE ( 'NONE', *, *, #34837, .F. ) ;
#22646 = CARTESIAN_POINT ( 'NONE',  ( 15.44803555374680393, 6.237487519713364570, -3.546734833711462365 ) ) ;
#22647 = AXIS2_PLACEMENT_3D ( 'NONE', #7988, #35451, #3868 ) ;
#22648 = LINE ( 'NONE', #44958, #39300 ) ;
#22649 = CARTESIAN_POINT ( 'NONE',  ( -128.4459734468149179, 0.000000000000000000, 2.568287556927950632 ) ) ;
#22650 = EDGE_CURVE ( 'NONE', #17310, #46387, #41316, .T. ) ;
#22651 = ORIENTED_EDGE ( 'NONE', *, *, #48795, .F. ) ;
#22652 = ORIENTED_EDGE ( 'NONE', *, *, #41883, .T. ) ;
#22653 = CARTESIAN_POINT ( 'NONE',  ( -5.000000000000000000, 175.0000000000000284, 346.2500000000002274 ) ) ;
#22654 = CARTESIAN_POINT ( 'NONE',  ( 33.30402655318503946, 1.750000000000009992, -159.1817124430720298 ) ) ;
#22655 = ORIENTED_EDGE ( 'NONE', *, *, #10685, .F. ) ;
#22656 = ORIENTED_EDGE ( 'NONE', *, *, #46155, .F. ) ;
#22657 = CARTESIAN_POINT ( 'NONE',  ( 35.00000000000186162, 17.00000000000000000, 90.00000000000000000 ) ) ;
#22658 = CARTESIAN_POINT ( 'NONE',  ( -84.94597344681494633, 2.143131898507880377E-16, -120.9317124430720156 ) ) ;
#22659 = CARTESIAN_POINT ( 'NONE',  ( 344.0000000000000568, 167.0000000000000000, 341.9999999999998863 ) ) ;
#22660 = ORIENTED_EDGE ( 'NONE', *, *, #31789, .F. ) ;
#22661 = CARTESIAN_POINT ( 'NONE',  ( 35.00000000000186162, 17.00000000000000000, 65.00000000000000000 ) ) ;
#22662 = VERTEX_POINT ( 'NONE', #8765 ) ;
#22663 = EDGE_CURVE ( 'NONE', #27818, #26389, #36540, .T. ) ;
#22664 = ADVANCED_FACE ( 'NONE', ( #43631 ), #35532, .T. ) ;
#22665 = DIRECTION ( 'NONE',  ( 0.000000000000000000, -2.265761274745217480E-16, 1.000000000000000000 ) ) ;
#22666 = AXIS2_PLACEMENT_3D ( 'NONE', #9975, #2772, #1781 ) ;
#22667 = LINE ( 'NONE', #38086, #46318 ) ;
#22668 = ADVANCED_FACE ( 'NONE', ( #20295 ), #27497, .T. ) ;
#22669 = CARTESIAN_POINT ( 'NONE',  ( 151.5540265531850537, 1.025126265847089657, -80.93171244307201562 ) ) ;
#22670 = EDGE_LOOP ( 'NONE', ( #44428, #43360, #645, #9667, #46788 ) ) ;
#22671 = ORIENTED_EDGE ( 'NONE', *, *, #40725, .F. ) ;
#22672 = ORIENTED_EDGE ( 'NONE', *, *, #22998, .T. ) ;
#22673 = CARTESIAN_POINT ( 'NONE',  ( 340.0000000000001137, 183.3431457505076594, 358.3431457505074604 ) ) ;
#22674 = CARTESIAN_POINT ( 'NONE',  ( 181.0000000000000000, -164.9999999999999432, 343.9999999999998863 ) ) ;
#22675 = VERTEX_POINT ( 'NONE', #28257 ) ;
#22676 = DIRECTION ( 'NONE',  ( 1.586032892321652236E-16, 1.000000000000000000, 6.853681917100419162E-49 ) ) ;
#22677 = EDGE_CURVE ( 'NONE', #9127, #38661, #24416, .T. ) ;
#22678 = EDGE_CURVE ( 'NONE', #17360, #38683, #19703, .T. ) ;
#22679 = EDGE_LOOP ( 'NONE', ( #27355, #3499, #44821, #7134 ) ) ;
#22680 = DIRECTION ( 'NONE',  ( -1.000000000000000000, -0.000000000000000000, -0.000000000000000000 ) ) ;
#22681 = EDGE_LOOP ( 'NONE', ( #30374, #43216, #7185, #8366, #37584 ) ) ;
#22682 = CARTESIAN_POINT ( 'NONE',  ( -207.7210997126620384, 1.750000000000009326, 1.843413822775066269 ) ) ;
#22683 = ADVANCED_FACE ( 'NONE', ( #38217 ), #3027, .T. ) ;
#22684 = CARTESIAN_POINT ( 'NONE',  ( -30.87089393895367095, 12.69923079256638587, -9.367992836599954742 ) ) ;
#22685 = PLANE ( 'NONE',  #26113 ) ;
#22686 = ADVANCED_FACE ( 'NONE', ( #19180 ), #31266, .F. ) ;
#22687 = LINE ( 'NONE', #2188, #41330 ) ;
#22688 = ORIENTED_EDGE ( 'NONE', *, *, #25406, .T. ) ;
#22689 = CARTESIAN_POINT ( 'NONE',  ( -4.945973446814903696, 2.143131898507912917E-16, 79.06828755692795596 ) ) ;
#22690 = EDGE_CURVE ( 'NONE', #23786, #49960, #42676, .T. ) ;
#22691 = CARTESIAN_POINT ( 'NONE',  ( 0.4266413953668419246, 1.250184266969606162, 9.943883492372851407 ) ) ;
#22692 = CARTESIAN_POINT ( 'NONE',  ( 1.040834085586084257E-14, -6.912230148066169200, 5.000000000000000000 ) ) ;
#22693 = DIRECTION ( 'NONE',  ( 0.000000000000000000, 0.000000000000000000, -1.000000000000000000 ) ) ;
#22695 = DIRECTION ( 'NONE',  ( 0.000000000000000000, -0.9230769230769231282, 0.3846153846153845812 ) ) ;
#22694 = B_SPLINE_CURVE_WITH_KNOTS ( 'NONE', 3,
 ( #48528, #13418, #2137, #40876 ),
 .UNSPECIFIED., .F., .F.,
 ( 4, 4 ),
 ( 0.01010185847678694501, 0.01012833122191989475 ),
 .UNSPECIFIED. ) ;
#22696 = CARTESIAN_POINT ( 'NONE',  ( 85.00000000000184741, 16.00000000000000000, 90.00000000000000000 ) ) ;
#22697 = DIRECTION ( 'NONE',  ( 0.4740998230350172427, -0.3386427307392981256, -0.8127425537743157014 ) ) ;
#22698 = EDGE_CURVE ( 'NONE', #20659, #34186, #43036, .T. ) ;
#22699 = LINE ( 'NONE', #42196, #32891 ) ;
#22700 = VECTOR ( 'NONE', #35247, 1000.000000000000000 ) ;
#22701 = ORIENTED_EDGE ( 'NONE', *, *, #46919, .F. ) ;
#22702 = ADVANCED_FACE ( 'NONE', ( #7405 ), #46095, .F. ) ;
#22703 = EDGE_CURVE ( 'NONE', #5041, #47564, #18669, .T. ) ;
#22704 = FACE_BOUND ( 'NONE', #792, .T. ) ;
#22705 = FACE_OUTER_BOUND ( 'NONE', #35387, .T. ) ;
#22706 = CARTESIAN_POINT ( 'NONE',  ( 356.0000000000000568, 175.0000000000000284, -92.00000000000019895 ) ) ;
#22707 = ADVANCED_FACE ( 'NONE', ( #3277 ), #26644, .T. ) ;
#22708 = VERTEX_POINT ( 'NONE', #15602 ) ;
#22709 = EDGE_LOOP ( 'NONE', ( #41320, #19393, #23088, #17162 ) ) ;
#22710 = DIRECTION ( 'NONE',  ( 0.000000000000000000, 0.000000000000000000, 1.000000000000000000 ) ) ;
#22711 = B_SPLINE_CURVE_WITH_KNOTS ( 'NONE', 3,
 ( #11464, #50417, #11715, #26607 ),
 .UNSPECIFIED., .F., .F.,
 ( 4, 4 ),
 ( 0.0006669682284780797596, 0.0007799402130920312336 ),
 .UNSPECIFIED. ) ;
#22712 = EDGE_CURVE ( 'NONE', #25305, #41166, #1015, .T. ) ;
#22713 = CARTESIAN_POINT ( 'NONE',  ( -164.9459734468149463, 2.143131898507880377E-16, 42.56828755692798438 ) ) ;
#22714 = VECTOR ( 'NONE', #21592, 1000.000000000000000 ) ;
#22715 = ORIENTED_EDGE ( 'NONE', *, *, #4611, .T. ) ;
#22716 = ORIENTED_EDGE ( 'NONE', *, *, #5606, .F. ) ;
#22717 = CARTESIAN_POINT ( 'NONE',  ( -10.25676241992221449, 8.638513918217336496, 18.89424093979656405 ) ) ;
#22718 = CARTESIAN_POINT ( 'NONE',  ( 0.3862712429686815385, 1.188820645368943385, 9.972675548442461846 ) ) ;
#22719 = DIRECTION ( 'NONE',  ( -0.000000000000000000, -0.000000000000000000, -1.000000000000000000 ) ) ;
#22720 = ORIENTED_EDGE ( 'NONE', *, *, #20175, .T. ) ;
#22721 = VERTEX_POINT ( 'NONE', #46856 ) ;
#22722 = B_SPLINE_CURVE_WITH_KNOTS ( 'NONE', 3,
 ( #38130, #10653, #15015, #30416 ),
 .UNSPECIFIED., .F., .F.,
 ( 4, 4 ),
 ( 3.969024117295675979E-17, 0.0004301978946275559026 ),
 .UNSPECIFIED. ) ;
#22723 = VERTEX_POINT ( 'NONE', #26890 ) ;
#22724 =( BOUNDED_CURVE ( )  B_SPLINE_CURVE ( 3, ( #4714, #4456, #27568, #17012 ),
 .UNSPECIFIED., .F., .F. ) 
 B_SPLINE_CURVE_WITH_KNOTS ( ( 4, 4 ),
 ( 3.141592653589793116, 4.712388980384689674 ),
 .UNSPECIFIED. ) 
 CURVE ( )  GEOMETRIC_REPRESENTATION_ITEM ( )  RATIONAL_B_SPLINE_CURVE ( ( 1.000000000000000000, 0.8047378541243649375, 0.8047378541243649375, 1.000000000000000000 ) ) 
 REPRESENTATION_ITEM ( '' )  );
#22725 = CARTESIAN_POINT ( 'NONE',  ( 74.32915281903215998, -1.750000000000010436, 119.7931612910808781 ) ) ;
#22726 = CARTESIAN_POINT ( 'NONE',  ( -49.46074318306826001, 9.578883844007169301, 8.807470649214879543 ) ) ;
#22727 = DIRECTION ( 'NONE',  ( -0.000000000000000000, -0.000000000000000000, -1.000000000000000000 ) ) ;
#22728 = ORIENTED_EDGE ( 'NONE', *, *, #30543, .T. ) ;
#22729 = CARTESIAN_POINT ( 'NONE',  ( 181.0000000000000000, -168.9999999999999432, -350.0000000000001705 ) ) ;
#22730 = CARTESIAN_POINT ( 'NONE',  ( -206.6959734468149463, 1.750000000000009992, 0.8182875569279768335 ) ) ;
#22731 = ORIENTED_EDGE ( 'NONE', *, *, #12343, .F. ) ;
#22732 = ADVANCED_FACE ( 'NONE', ( #35382 ), #50180, .F. ) ;
#22733 = ORIENTED_EDGE ( 'NONE', *, *, #41518, .T. ) ;
#22734 = CARTESIAN_POINT ( 'NONE',  ( 112.2789002873379758, 1.749999999999996669, 159.7931612910809065 ) ) ;
#22735 = CYLINDRICAL_SURFACE ( 'NONE', #45550, 1.750000000000036193 ) ;
#22736 = CARTESIAN_POINT ( 'NONE',  ( -48.44597344681495343, 0.000000000000000000, -40.93171244307205825 ) ) ;
#22737 = ORIENTED_EDGE ( 'NONE', *, *, #8301, .T. ) ;
#22738 = ADVANCED_FACE ( 'NONE', ( #50448 ), #23558, .F. ) ;
#22739 = ORIENTED_EDGE ( 'NONE', *, *, #35355, .F. ) ;
#22740 = DIRECTION ( 'NONE',  ( -3.172065784643302499E-16, -1.000000000000000000, 2.537652627714641605E-15 ) ) ;
#22741 = CARTESIAN_POINT ( 'NONE',  ( -194.9999999999999432, -172.9999999999999716, 252.0000000000000568 ) ) ;
#22742 = EDGE_CURVE ( 'NONE', #45973, #27971, #15852, .T. ) ;
#22743 = FACE_OUTER_BOUND ( 'NONE', #11028, .T. ) ;
#22744 = CARTESIAN_POINT ( 'NONE',  ( -207.7210997126620384, 1.750000000000010436, 79.79316129108087807 ) ) ;
#22745 = EDGE_CURVE ( 'NONE', #37254, #302, #42530, .T. ) ;
#22746 = CARTESIAN_POINT ( 'NONE',  ( 356.0000000000000000, 165.0000000000000000, -106.0000000000001990 ) ) ;
#22747 = ORIENTED_EDGE ( 'NONE', *, *, #9317, .T. ) ;
#22748 =( LENGTH_UNIT ( ) NAMED_UNIT ( * ) SI_UNIT ( .MILLI., .METRE. ) );
#22749 = EDGE_CURVE ( 'NONE', #50360, #30887, #9838, .T. ) ;
#22750 = CARTESIAN_POINT ( 'NONE',  ( 210.0000000000000568, 2.143131898507880377E-16, -160.9317124430720298 ) ) ;
#22751 = EDGE_CURVE ( 'NONE', #37293, #26564, #34352, .T. ) ;
#22752 = LINE ( 'NONE', #14799, #23182 ) ;
#22753 = CARTESIAN_POINT ( 'NONE',  ( -1.019713130072858798, -3.848720492505054658, 6.098637220230962441E-17 ) ) ;
#22754 = CYLINDRICAL_SURFACE ( 'NONE', #31276, 1.750000000000015543 ) ;
#22755 = VECTOR ( 'NONE', #21475, 1000.000000000000000 ) ;
#22756 = CARTESIAN_POINT ( 'NONE',  ( 344.0000000000000000, -167.0000000000001137, 342.0000000000000000 ) ) ;
#22757 = ORIENTED_EDGE ( 'NONE', *, *, #35761, .T. ) ;
#22758 = CARTESIAN_POINT ( 'NONE',  ( 23.29043492822826167, -24.10797434788167948, 1.847720168420772691 ) ) ;
#22759 = CARTESIAN_POINT ( 'NONE',  ( 193.3040265531851105, 0.000000000000000000, 165.0000000000000000 ) ) ;
#22760 = CARTESIAN_POINT ( 'NONE',  ( 7.500000000000000000, 224.9999999999999716, -240.0000000000000000 ) ) ;
#22761 = ORIENTED_EDGE ( 'NONE', *, *, #7992, .T. ) ;
#22762 = CYLINDRICAL_SURFACE ( 'NONE', #24044, 1.750000000000001554 ) ;
#22763 = EDGE_CURVE ( 'NONE', #20370, #47244, #26388, .T. ) ;
#22764 = CARTESIAN_POINT ( 'NONE',  ( 339.9999999999999432, 165.0000000000000000, -344.0000000000001705 ) ) ;
#22765 = VERTEX_POINT ( 'NONE', #42034 ) ;
#22766 = CARTESIAN_POINT ( 'NONE',  ( -125.6708471809678542, -1.749999999999996669, -78.15658617722492352 ) ) ;
#22767 = CARTESIAN_POINT ( 'NONE',  ( 2.178343065408716139, 16.64136160116211727, -9.233365092205394475 ) ) ;
#22768 = CARTESIAN_POINT ( 'NONE',  ( 360.0000000000000000, 181.0000000000000284, -356.0000000000001705 ) ) ;
#22769 = LINE ( 'NONE', #19162, #32369 ) ;
#22770 = AXIS2_PLACEMENT_3D ( 'NONE', #41936, #21671, #6783 ) ;
#22771 = VERTEX_POINT ( 'NONE', #37701 ) ;
#22772 = CARTESIAN_POINT ( 'NONE',  ( 210.0000000000000568, 0.000000000000000000, 162.5682875569279702 ) ) ;
#22773 = B_SPLINE_SURFACE_WITH_KNOTS ( 'NONE', 3, 3, ( 
 ( #188, #23258, #39444, #27377 ),
 ( #38679, #39193, #11984, #4025 ),
 ( #19421, #27638, #3771, #15826 ),
 ( #43270, #7890, #19670, #15574 ) ),
 .UNSPECIFIED., .F., .F., .F.,
 ( 4, 4 ),
 ( 4, 4 ),
 ( 0.000000000000000000, 1.000000000000000000 ),
 ( 0.000000000000000000, 1.000000000000000000 ),
 .UNSPECIFIED. ) ;
#22774 = ORIENTED_EDGE ( 'NONE', *, *, #30936, .T. ) ;
#22775 = ORIENTED_EDGE ( 'NONE', *, *, #26594, .T. ) ;
#22776 = FACE_OUTER_BOUND ( 'NONE', #44665, .T. ) ;
#22777 = ORIENTED_EDGE ( 'NONE', *, *, #7332, .F. ) ;
#22778 = CARTESIAN_POINT ( 'NONE',  ( 357.9999999999999432, 174.9999999999996589, -356.0000000000003411 ) ) ;
#22779 = CARTESIAN_POINT ( 'NONE',  ( -15.62858259096117841, 5.755205073598721910, -9.683996418299976483 ) ) ;
#22780 = CARTESIAN_POINT ( 'NONE',  ( 30.00000000000123279, 17.00000000000000000, 30.00000000000000000 ) ) ;
#22781 = EDGE_CURVE ( 'NONE', #23545, #30427, #48773, .T. ) ;
#22782 = DIRECTION ( 'NONE',  ( -2.775557561562891351E-16, -0.7071067811865477948, -0.7071067811865473507 ) ) ;
#22783 = ORIENTED_EDGE ( 'NONE', *, *, #21784, .F. ) ;
#22784 = CARTESIAN_POINT ( 'NONE',  ( 344.0000000000000568, 169.0000000000000000, 349.9999999999998295 ) ) ;
#22785 = CARTESIAN_POINT ( 'NONE',  ( 33.30402655318503946, 1.750000000000009992, 160.8182875569279702 ) ) ;
#22786 = FACE_OUTER_BOUND ( 'NONE', #47197, .T. ) ;
#22787 = EDGE_LOOP ( 'NONE', ( #14965, #37467, #1761, #5407 ) ) ;
#22788 = VECTOR ( 'NONE', #21614, 1000.000000000000000 ) ;
#22789 = B_SPLINE_CURVE_WITH_KNOTS ( 'NONE', 3,
 ( #43145, #39305, #43379, #19788 ),
 .UNSPECIFIED., .F., .F.,
 ( 4, 4 ),
 ( 0.7491799374948677759, 1.000000000000000000 ),
 .UNSPECIFIED. ) ;
#22790 = PLANE ( 'NONE',  #31724 ) ;
#22791 = LINE ( 'NONE', #26895, #4015 ) ;
#22792 = ORIENTED_EDGE ( 'NONE', *, *, #31926, .T. ) ;
#22793 = ORIENTED_EDGE ( 'NONE', *, *, #33065, .T. ) ;
#22794 = ORIENTED_EDGE ( 'NONE', *, *, #12373, .F. ) ;
#22795 = CARTESIAN_POINT ( 'NONE',  ( 195.9157620838774676, 159.2880105690400399, 472.6625600500173050 ) ) ;
#22796 = CARTESIAN_POINT ( 'NONE',  ( -1.011271242968693862, 0.7347315653655780432, 10.00000000000000000 ) ) ;
#22797 = ORIENTED_EDGE ( 'NONE', *, *, #29580, .F. ) ;
#22798 = CARTESIAN_POINT ( 'NONE',  ( -1.066995270233474624, 33.23888904628638841, -3.760136334089591248 ) ) ;
#22799 = DIRECTION ( 'NONE',  ( 0.000000000000000000, 1.000000000000000000, 3.186989995019654210E-49 ) ) ;
#22800 = FACE_OUTER_BOUND ( 'NONE', #12454, .T. ) ;
#22801 = ADVANCED_FACE ( 'NONE', ( #41778 ), #18425, .F. ) ;
#22802 = CARTESIAN_POINT ( 'NONE',  ( 113.3040265531850537, 0.000000000000000000, 165.0000000000000000 ) ) ;
#22803 = CARTESIAN_POINT ( 'NONE',  ( -6.429410166934457216, -2.386389549874184279, 9.753789706659947711 ) ) ;
#22804 = EDGE_CURVE ( 'NONE', #43558, #2880, #6634, .T. ) ;
#22805 = CARTESIAN_POINT ( 'NONE',  ( 168.9999999999999716, -95.49999999999997158, -115.0000000000001563 ) ) ;
#22806 = DIRECTION ( 'NONE',  ( 1.000000000000000000, 0.000000000000000000, -0.000000000000000000 ) ) ;
#22807 = CARTESIAN_POINT ( 'NONE',  ( -1.011271242968677875, -0.7347315653656004697, 10.00000000000000000 ) ) ;
#22808 = ADVANCED_FACE ( 'NONE', ( #22786 ), #33595, .F. ) ;
#22809 = DIRECTION ( 'NONE',  ( 0.000000000000000000, 0.000000000000000000, 1.000000000000000000 ) ) ;
#22810 = ORIENTED_EDGE ( 'NONE', *, *, #31994, .F. ) ;
#22811 = ADVANCED_FACE ( 'NONE', ( #14327 ), #2277, .F. ) ;
#22812 = EDGE_CURVE ( 'NONE', #913, #50273, #18675, .T. ) ;
#22813 = FACE_OUTER_BOUND ( 'NONE', #47237, .T. ) ;
#22814 = LINE ( 'NONE', #7436, #8685 ) ;
#22815 = CARTESIAN_POINT ( 'NONE',  ( 9.174209336589868258, 3.979181203266223488, 9.646707543097347681 ) ) ;
#22816 = CARTESIAN_POINT ( 'NONE',  ( -3.231548175622898089, 9.463461120997347820, 9.282506307616472441 ) ) ;
#22817 = ORIENTED_EDGE ( 'NONE', *, *, #23279, .T. ) ;
#22818 = CARTESIAN_POINT ( 'NONE',  ( 0.000000000000000000, 0.000000000000000000, 15.00000000000000000 ) ) ;
#22819 = CARTESIAN_POINT ( 'NONE',  ( 113.3040265531850537, 0.000000000000000000, 165.0000000000000000 ) ) ;
#22820 = EDGE_CURVE ( 'NONE', #37811, #5747, #42290, .T. ) ;
#22821 = CARTESIAN_POINT ( 'NONE',  ( -0.3862712429686895876, 1.188820645368940720, 10.00000000000000000 ) ) ;
#22822 = CARTESIAN_POINT ( 'NONE',  ( -127.7210997126620242, 1.749999999999996669, 121.8434138227750481 ) ) ;
#22823 = CARTESIAN_POINT ( 'NONE',  ( 339.9999999999998863, -168.9999999999999716, -360.0000000000003411 ) ) ;
#22824 = B_SPLINE_CURVE_WITH_KNOTS ( 'NONE', 3,
 ( #14169, #29843, #40881, #29586 ),
 .UNSPECIFIED., .F., .F.,
 ( 4, 4 ),
 ( 1.735570302229820823E-18, 2.647279941212161278E-05 ),
 .UNSPECIFIED. ) ;
#22825 = VERTEX_POINT ( 'NONE', #22533 ) ;
#22827 = VERTEX_POINT ( 'NONE', #37461 ) ;
#22826 = VECTOR ( 'NONE', #13169, 999.9999999999998863 ) ;
#22828 = CARTESIAN_POINT ( 'NONE',  ( 0.1469336902871260508, 1.496274467947966258, 9.953784399990622589 ) ) ;
#22829 = EDGE_LOOP ( 'NONE', ( #20887, #30706, #1637, #841, #25781, #18270 ) ) ;
#22830 = CARTESIAN_POINT ( 'NONE',  ( 0.4266413953668419246, 1.250184266969606162, 9.943883492372851407 ) ) ;
#22831 = FACE_OUTER_BOUND ( 'NONE', #32878, .T. ) ;
#22832 = ORIENTED_EDGE ( 'NONE', *, *, #34471, .T. ) ;
#22833 = SURFACE_STYLE_USAGE ( .BOTH. , #6675 ) ;
#22834 = ORIENTED_EDGE ( 'NONE', *, *, #6572, .F. ) ;
#22835 = ORIENTED_EDGE ( 'NONE', *, *, #34901, .F. ) ;
#22836 = LINE ( 'NONE', #18219, #19636 ) ;
#22837 = CARTESIAN_POINT ( 'NONE',  ( -164.9459734468149463, 2.143131898507880377E-16, 119.0682875569279702 ) ) ;
#22838 = ORIENTED_EDGE ( 'NONE', *, *, #22242, .T. ) ;
#22839 = CARTESIAN_POINT ( 'NONE',  ( 0.9870575514054733546, 1.980598328282569653, 9.881002359080278907 ) ) ;
#22840 = LINE ( 'NONE', #6684, #4603 ) ;
#22841 = DIRECTION ( 'NONE',  ( -1.000000000000000000, -0.000000000000000000, -0.000000000000000000 ) ) ;
#22842 = EDGE_LOOP ( 'NONE', ( #19534, #35082, #43134, #42720, #8089, #36965, #29934, #22427, #42295, #45580 ) ) ;
#22843 = EDGE_LOOP ( 'NONE', ( #40284, #48260, #10305, #8285, #18506, #23237, #24142, #19951, #49884, #28921, #44172, #50625, #27349, #45535, #29777, #40674, #15396, #35871, #34571, #17298, #4939, #39554, #13209, #11113, #30948, #44409, #24612, #47008, #9288, #3345 ) ) ;
#22844 = CARTESIAN_POINT ( 'NONE',  ( -2.948105490345101387, -9.555557232197246620, 9.282506307616472441 ) ) ;
#22845 = ADVANCED_FACE ( 'NONE', ( #13811 ), #38463, .F. ) ;
#22846 = CARTESIAN_POINT ( 'NONE',  ( 152.2789002873379900, 1.750000000000009326, 1.843413822775066269 ) ) ;
#22847 = ORIENTED_EDGE ( 'NONE', *, *, #28503, .T. ) ;
#22848 = DIRECTION ( 'NONE',  ( -0.000000000000000000, -0.000000000000000000, -1.000000000000000000 ) ) ;
#22849 = CARTESIAN_POINT ( 'NONE',  ( -20.21530556545279111, 31.58467066308232063, -9.422646554964174470 ) ) ;
#22850 = ORIENTED_EDGE ( 'NONE', *, *, #2203, .T. ) ;
#22851 = CARTESIAN_POINT ( 'NONE',  ( -44.94597344681493922, 2.143131898507880377E-16, -157.4317124430720014 ) ) ;
#22852 = FACE_OUTER_BOUND ( 'NONE', #27015, .T. ) ;
#22853 = VERTEX_POINT ( 'NONE', #38218 ) ;
#22854 = CARTESIAN_POINT ( 'NONE',  ( 193.3040265531851105, 1.750000000000009992, -159.1817124430720298 ) ) ;
#22855 = VECTOR ( 'NONE', #49882, 1000.000000000000000 ) ;
#22856 = CARTESIAN_POINT ( 'NONE',  ( -543.3973046169135159, 54.43801056904003133, -177.1374399499827916 ) ) ;
#22857 =( BOUNDED_CURVE ( )  B_SPLINE_CURVE ( 3, ( #26080, #2230, #2972, #33299 ),
 .UNSPECIFIED., .F., .F. ) 
 B_SPLINE_CURVE_WITH_KNOTS ( ( 4, 4 ),
 ( 4.712388980384689674, 6.283185307179586232 ),
 .UNSPECIFIED. ) 
 CURVE ( )  GEOMETRIC_REPRESENTATION_ITEM ( )  RATIONAL_B_SPLINE_CURVE ( ( 1.000000000000000000, 0.8047378541243649375, 0.8047378541243649375, 1.000000000000000000 ) ) 
 REPRESENTATION_ITEM ( '' )  );
#22858 = EDGE_CURVE ( 'NONE', #28153, #40717, #14073, .T. ) ;
#22859 = AXIS2_PLACEMENT_3D ( 'NONE', #15441, #3637, #46953 ) ;
#22860 = EDGE_CURVE ( 'NONE', #3579, #16946, #9979, .T. ) ;
#22861 = ORIENTED_EDGE ( 'NONE', *, *, #42456, .T. ) ;
#22862 = CARTESIAN_POINT ( 'NONE',  ( -1.377509002708424468, 0.6027468487255034368, 9.927319414211229542 ) ) ;
#22863 = CIRCLE ( 'NONE', #25329, 1.750000000000008438 ) ;
#22864 = VECTOR ( 'NONE', #48681, 1000.000000000000000 ) ;
#22865 = PRESENTATION_STYLE_ASSIGNMENT (( #41865 ) ) ;
#22866 =( BOUNDED_CURVE ( )  B_SPLINE_CURVE ( 3, ( #44833, #9203, #24863, #45332 ),
 .UNSPECIFIED., .F., .F. ) 
 B_SPLINE_CURVE_WITH_KNOTS ( ( 4, 4 ),
 ( 1.570796326794896558, 3.141592653589793116 ),
 .UNSPECIFIED. ) 
 CURVE ( )  GEOMETRIC_REPRESENTATION_ITEM ( )  RATIONAL_B_SPLINE_CURVE ( ( 1.000000000000000000, 0.8047378541243649375, 0.8047378541243649375, 1.000000000000000000 ) ) 
 REPRESENTATION_ITEM ( '' )  );
#22867 = CARTESIAN_POINT ( 'NONE',  ( 10.70590866674922204, -12.76446523155706814, -3.546734833711462365 ) ) ;
#22868 = ORIENTED_EDGE ( 'NONE', *, *, #28499, .T. ) ;
#22869 = ORIENTED_EDGE ( 'NONE', *, *, #27580, .F. ) ;
#22870 = EDGE_CURVE ( 'NONE', #20500, #2288, #6380, .T. ) ;
#22871 = DIRECTION ( 'NONE',  ( 0.9767437569925631058, -4.158490309726805533E-16, 0.2144099651976388021 ) ) ;
#22872 = ADVANCED_FACE ( 'NONE', ( #25639 ), #25896, .F. ) ;
#22873 = CARTESIAN_POINT ( 'NONE',  ( 6.909265173666245374, -36.86491375218297861, 8.100132398494514163 ) ) ;
#22874 = CARTESIAN_POINT ( 'NONE',  ( 2.595273106918288164, 2.906811120256387326, 9.741991644047248045 ) ) ;
#22875 = CARTESIAN_POINT ( 'NONE',  ( -1.172603113866931501, -0.3455467477709202595, 9.987567862361071747 ) ) ;
#22876 = CARTESIAN_POINT ( 'NONE',  ( -124.9459734468149321, 1.025126265847081664, -157.4317124430720582 ) ) ;
#22877 = DIRECTION ( 'NONE',  ( -1.000000000000000000, -0.000000000000000000, -0.000000000000000000 ) ) ;
#22878 = DIRECTION ( 'NONE',  ( 0.000000000000000000, -0.000000000000000000, -1.000000000000000000 ) ) ;
#22879 = ORIENTED_EDGE ( 'NONE', *, *, #44782, .T. ) ;
#22880 = EDGE_CURVE ( 'NONE', #35976, #1474, #22027, .T. ) ;
#22881 = DIRECTION ( 'NONE',  ( 1.000000000000000000, 0.000000000000000000, 0.000000000000000000 ) ) ;
#22882 =( BOUNDED_CURVE ( )  B_SPLINE_CURVE ( 3, ( #18371, #41733, #28490, #10433 ),
 .UNSPECIFIED., .F., .F. ) 
 B_SPLINE_CURVE_WITH_KNOTS ( ( 4, 4 ),
 ( 4.712388980384689674, 6.283185307179586232 ),
 .UNSPECIFIED. ) 
 CURVE ( )  GEOMETRIC_REPRESENTATION_ITEM ( )  RATIONAL_B_SPLINE_CURVE ( ( 1.000000000000000000, 0.8047378541243649375, 0.8047378541243649375, 1.000000000000000000 ) ) 
 REPRESENTATION_ITEM ( '' )  );
#22883 = PRODUCT_DEFINITION_SHAPE ( 'NONE', 'NONE',  #50725 ) ;
#22884 = CARTESIAN_POINT ( 'NONE',  ( 130.0000000000012221, 17.00000000000000000, 30.00000000000000000 ) ) ;
#22885 = DIRECTION ( 'NONE',  ( 0.8637789008984335659, -0.000000000000000000, 0.5038710255240859137 ) ) ;
#22886 = EDGE_LOOP ( 'NONE', ( #4545, #50440, #8950, #8306 ) ) ;
#22887 = CARTESIAN_POINT ( 'NONE',  ( 72.27890028733797578, -1.750000000000009548, 159.7931612910809065 ) ) ;
#22888 = CARTESIAN_POINT ( 'NONE',  ( 224.9999999999999432, -175.0000000000000000, 500.0000000000000000 ) ) ;
#22889 = ORIENTED_EDGE ( 'NONE', *, *, #37456, .F. ) ;
#22890 = CYLINDRICAL_SURFACE ( 'NONE', #14737, 1.750000000000001554 ) ;
#22891 = DIRECTION ( 'NONE',  ( -1.942330104924128867E-32, 0.000000000000000000, -1.000000000000000000 ) ) ;
#22892 = CARTESIAN_POINT ( 'NONE',  ( 210.0000000000000568, 2.143131898507881116E-16, 39.06828755692797728 ) ) ;
#22893 = EDGE_LOOP ( 'NONE', ( #1542, #49231, #19312, #4215, #3461, #27553 ) ) ;
#22894 = VECTOR ( 'NONE', #9640, 1000.000000000000000 ) ;
#22895 = AXIS2_PLACEMENT_3D ( 'NONE', #36556, #4969, #24234 ) ;
#22896 = FACE_OUTER_BOUND ( 'NONE', #3914, .T. ) ;
#22897 = CARTESIAN_POINT ( 'NONE',  ( 33.30402655318503946, 1.750000000000010214, -39.18171244307202983 ) ) ;
#22898 = VERTEX_POINT ( 'NONE', #45844 ) ;
#22899 = CARTESIAN_POINT ( 'NONE',  ( -1.780494907546731120, -1.041382914740391019, 9.891980816076523908 ) ) ;
#22900 = CARTESIAN_POINT ( 'NONE',  ( -46.69597344681494633, 1.750000000000009992, -159.1817124430720298 ) ) ;
#22901 = CIRCLE ( 'NONE', #34381, 0.4999999999999992228 ) ;
#22902 = CARTESIAN_POINT ( 'NONE',  ( -214.9999999999999432, 173.0000000000000000, 372.0000000000000000 ) ) ;
#22903 = VECTOR ( 'NONE', #254, 1000.000000000000000 ) ;
#22904 = ORIENTED_EDGE ( 'NONE', *, *, #19976, .F. ) ;
#22905 = ORIENTED_EDGE ( 'NONE', *, *, #4223, .F. ) ;
#22906 = DIRECTION ( 'NONE',  ( 0.000000000000000000, 0.000000000000000000, 1.000000000000000000 ) ) ;
#22907 = LINE ( 'NONE', #38586, #20589 ) ;
#22908 = EDGE_CURVE ( 'NONE', #40358, #3643, #36399, .T. ) ;
#22909 = VECTOR ( 'NONE', #37572, 1000.000000000000000 ) ;
#22910 = ORIENTED_EDGE ( 'NONE', *, *, #28399, .T. ) ;
#22911 = VERTEX_POINT ( 'NONE', #38964 ) ;
#22912 = CARTESIAN_POINT ( 'NONE',  ( 73.30402655318508209, 1.750000000000009992, 0.8182875569279768335 ) ) ;
#22913 = CARTESIAN_POINT ( 'NONE',  ( 183.0000000000000000, -174.9999999999999716, -356.0000000000001705 ) ) ;
#22914 = MANIFOLD_SOLID_BREP ( 'Square tube 20 X 20 X 2(1)[6]', #2363 ) ;
#22915 = DIRECTION ( 'NONE',  ( 0.000000000000000000, 0.000000000000000000, 1.000000000000000000 ) ) ;
#22916 = EDGE_LOOP ( 'NONE', ( #32279, #19426, #40171, #25565 ) ) ;
#22917 = CARTESIAN_POINT ( 'NONE',  ( -1.111875982683548703, -1.111927553622429343, 9.927288994922816912 ) ) ;
#22918 = VERTEX_POINT ( 'NONE', #3798 ) ;
#22919 = FACE_OUTER_BOUND ( 'NONE', #44894, .T. ) ;
#22920 = CARTESIAN_POINT ( 'NONE',  ( -128.4459734468149179, 0.000000000000000000, 82.56828755692795596 ) ) ;
#22921 = CYLINDRICAL_SURFACE ( 'NONE', #27986, 0.4999999999999997224 ) ;
#22922 = ORIENTED_EDGE ( 'NONE', *, *, #31822, .F. ) ;
#22923 = ORIENTED_EDGE ( 'NONE', *, *, #20837, .T. ) ;
#22924 = VERTEX_POINT ( 'NONE', #43037 ) ;
#22925 = DIRECTION ( 'NONE',  ( -0.000000000000000000, -0.000000000000000000, -1.000000000000000000 ) ) ;
#22926 = CARTESIAN_POINT ( 'NONE',  ( -0.6126904405382037622, -1.085824959725731231, 9.981352469109934233 ) ) ;
#22927 = DIRECTION ( 'NONE',  ( -1.000000000000000000, 0.000000000000000000, 0.000000000000000000 ) ) ;
#22928 = ORIENTED_EDGE ( 'NONE', *, *, #4974, .T. ) ;
#22929 = CARTESIAN_POINT ( 'NONE',  ( -1.370084944437349295, -0.09457992852950281026, 9.946805383069644790 ) ) ;
#22930 = ORIENTED_EDGE ( 'NONE', *, *, #33997, .T. ) ;
#22931 = DIRECTION ( 'NONE',  ( -1.000000000000000000, 0.000000000000000000, -0.000000000000000000 ) ) ;
#22933 = ORIENTED_EDGE ( 'NONE', *, *, #18598, .F. ) ;
#22932 = CIRCLE ( 'NONE', #24555, 4.000000000000003553 ) ;
#22934 = DIRECTION ( 'NONE',  ( 0.000000000000000000, 1.000000000000000000, 0.000000000000000000 ) ) ;
#22935 = CARTESIAN_POINT ( 'NONE',  ( -46.69597344681494633, -1.750000000000010658, 80.81828755692798438 ) ) ;
#22936 = DIRECTION ( 'NONE',  ( 0.000000000000000000, 0.000000000000000000, 1.000000000000000000 ) ) ;
#22937 = CARTESIAN_POINT ( 'NONE',  ( 191.5540265531851105, 0.000000000000000000, -117.4317124430720725 ) ) ;
#22938 = CARTESIAN_POINT ( 'NONE',  ( 1.249999999999999778, 0.000000000000000000, 3.333333333333333481 ) ) ;
#22939 = ORIENTED_EDGE ( 'NONE', *, *, #23116, .F. ) ;
#22940 = EDGE_CURVE ( 'NONE', #42417, #40803, #32500, .T. ) ;
#22941 = CARTESIAN_POINT ( 'NONE',  ( 9.358026734184097251, 0.000000000000000000, 0.000000000000000000 ) ) ;
#22942 = CARTESIAN_POINT ( 'NONE',  ( -87.72109971266203843, -1.750000000000010214, -80.20683870891910772 ) ) ;
#22943 = CARTESIAN_POINT ( 'NONE',  ( 0.000000000000000000, 17.00000000000000000, 0.000000000000000000 ) ) ;
#22944 = DIRECTION ( 'NONE',  ( -0.000000000000000000, -0.000000000000000000, -1.000000000000000000 ) ) ;
#22945 = VECTOR ( 'NONE', #3081, 1000.000000000000000 ) ;
#22946 = DIRECTION ( 'NONE',  ( 0.000000000000000000, 1.000000000000000000, -2.969158215481698263E-48 ) ) ;
#22947 = CARTESIAN_POINT ( 'NONE',  ( -29.39982726364978660, -16.78152490921149109, 8.356839323120299312 ) ) ;
#22948 = EDGE_LOOP ( 'NONE', ( #23664, #37455, #43542, #44373, #43295, #3843 ) ) ;
#22949 = DIRECTION ( 'NONE',  ( 0.000000000000000000, 1.000000000000000000, 0.000000000000000000 ) ) ;
#22950 = DIRECTION ( 'NONE',  ( -0.000000000000000000, -0.000000000000000000, 1.000000000000000000 ) ) ;
#22951 = ORIENTED_EDGE ( 'NONE', *, *, #13132, .T. ) ;
#22952 = CARTESIAN_POINT ( 'NONE',  ( 1.011271242968677653, 0.7347315653656002477, -3.333333333333333481 ) ) ;
#22953 = DIRECTION ( 'NONE',  ( 0.000000000000000000, 0.000000000000000000, 1.000000000000000000 ) ) ;
#22954 = CARTESIAN_POINT ( 'NONE',  ( 0.9015506157962454026, -0.9804419706258503675, 9.951893257060014264 ) ) ;
#22955 = EDGE_LOOP ( 'NONE', ( #31253, #30220, #37065, #19982, #30893, #40113 ) ) ;
#22956 = ORIENTED_EDGE ( 'NONE', *, *, #19615, .T. ) ;
#22957 = CARTESIAN_POINT ( 'NONE',  ( -6.174150299305392053, 33.14591993373988998, 8.807470649214879543 ) ) ;
#22958 = CARTESIAN_POINT ( 'NONE',  ( -1.066995270233474624, 33.23888904628638841, -3.760136334089591248 ) ) ;
#22959 = TOROIDAL_SURFACE ( 'NONE', #16418, 14.00000000000000355, 20.99999999999999289 ) ;
#22960 = AXIS2_PLACEMENT_3D ( 'NONE', #37563, #6735, #22383 ) ;
#22961 = ORIENTED_EDGE ( 'NONE', *, *, #35914, .T. ) ;
#22962 = ORIENTED_EDGE ( 'NONE', *, *, #28054, .F. ) ;
#22963 = CARTESIAN_POINT ( 'NONE',  ( 0.3862712429686978033, -1.188820645368937834, 10.00000000000000000 ) ) ;
#22964 = CARTESIAN_POINT ( 'NONE',  ( -0.3370904143228927730, -0.2449105217885335917, 10.00000000000000000 ) ) ;
#22965 = CYLINDRICAL_SURFACE ( 'NONE', #3752, 1.750000000000015543 ) ;
#22966 = ORIENTED_EDGE ( 'NONE', *, *, #3261, .F. ) ;
#22967 = ORIENTED_EDGE ( 'NONE', *, *, #44628, .F. ) ;
#22968 = VECTOR ( 'NONE', #15365, 1000.000000000000000 ) ;
#22969 = VERTEX_POINT ( 'NONE', #50449 ) ;
#22970 = VECTOR ( 'NONE', #47882, 1000.000000000000000 ) ;
#22971=STYLED_ITEM('',(#50754),#5950);
#22972 = DIRECTION ( 'NONE',  ( -0.000000000000000000, -1.000000000000000000, 2.537652627714643577E-15 ) ) ;
#22973 = DIRECTION ( 'NONE',  ( 0.000000000000000000, 5.664403186863042467E-17, 1.000000000000000000 ) ) ;
#22974 = VERTEX_POINT ( 'NONE', #39217 ) ;
#22975 = CARTESIAN_POINT ( 'NONE',  ( 0.000000000000000000, 0.000000000000000000, 0.000000000000000000 ) ) ;
#22976 = DIRECTION ( 'NONE',  ( 0.000000000000000000, -1.000000000000000000, 0.000000000000000000 ) ) ;
#22977 = DIRECTION ( 'NONE',  ( 0.000000000000000000, -0.4436251537532894806, 0.8962124318248270161 ) ) ;
#22978 = EDGE_LOOP ( 'NONE', ( #31330, #44029, #2216, #12899 ) ) ;
#22979 = EDGE_LOOP ( 'NONE', ( #38214, #7556 ) ) ;
#22980 = CARTESIAN_POINT ( 'NONE',  ( 0.9494396179258391966, -9.954826186926261755, 9.646707543097345905 ) ) ;
#22981 = CARTESIAN_POINT ( 'NONE',  ( 344.0000000000000000, 165.0000000000001990, -340.0000000000002842 ) ) ;
#22982 = DIRECTION ( 'NONE',  ( 0.000000000000000000, 0.000000000000000000, 1.000000000000000000 ) ) ;
#22983 = VERTEX_POINT ( 'NONE', #30754 ) ;
#22984 = ORIENTED_EDGE ( 'NONE', *, *, #31343, .F. ) ;
#22985 = CARTESIAN_POINT ( 'NONE',  ( 350.0000000000000000, 181.0000000000000284, -358.0000000000002274 ) ) ;
#22986 = CARTESIAN_POINT ( 'NONE',  ( -114.9999999999997158, 16.00000000000000000, -60.00000000000000000 ) ) ;
#22987 = CARTESIAN_POINT ( 'NONE',  ( -49.99999999999999289, 0.000000000000000000, 800.0000000000000000 ) ) ;
#22988 = EDGE_CURVE ( 'NONE', #27847, #48161, #31267, .T. ) ;
#22989 = CARTESIAN_POINT ( 'NONE',  ( 1.011271242968677653, 0.7347315653656002477, 3.333333333333333481 ) ) ;
#22990 = ORIENTED_EDGE ( 'NONE', *, *, #19742, .T. ) ;
#22991 = DIRECTION ( 'NONE',  ( 0.000000000000000000, 0.000000000000000000, -1.000000000000000000 ) ) ;
#22992 = EDGE_CURVE ( 'NONE', #23347, #27632, #8421, .T. ) ;
#22993 = DIRECTION ( 'NONE',  ( 0.000000000000000000, 0.000000000000000000, -1.000000000000000000 ) ) ;
#22994 = CARTESIAN_POINT ( 'NONE',  ( -5.000000000000000000, -184.7999999999999545, 359.7999999999997840 ) ) ;
#22995 = EDGE_CURVE ( 'NONE', #40295, #5199, #12698, .T. ) ;
#22996 = VECTOR ( 'NONE', #25560, 1000.000000000000000 ) ;
#22997 = CARTESIAN_POINT ( 'NONE',  ( -6.000000000000000888, 0.000000000000000000, 5.000000000000000000 ) ) ;
#22998 = EDGE_CURVE ( 'NONE', #18651, #9239, #23559, .T. ) ;
#22999 = VECTOR ( 'NONE', #17158, 1000.000000000000000 ) ;
#23000 = LINE ( 'NONE', #10697, #19956 ) ;
#23001 = VERTEX_POINT ( 'NONE', #38707 ) ;
#23002 = CARTESIAN_POINT ( 'NONE',  ( 6.174150299305392053, -50.00000000000000711, 8.807470649214879543 ) ) ;
#23003 = FACE_OUTER_BOUND ( 'NONE', #9410, .T. ) ;
#23004 = AXIS2_PLACEMENT_3D ( 'NONE', #19153, #9642, #44510 ) ;
#23005 = CARTESIAN_POINT ( 'NONE',  ( 1.593403307200061292, 0.6097984806595578844, 9.912102921405024247 ) ) ;
#23006 = ORIENTED_EDGE ( 'NONE', *, *, #44331, .F. ) ;
#23007 = CYLINDRICAL_SURFACE ( 'NONE', #29745, 1.750000000000015543 ) ;
#23008 = DIRECTION ( 'NONE',  ( -7.793956916774525800E-48, 0.000000000000000000, -1.000000000000000000 ) ) ;
#23009 = ORIENTED_EDGE ( 'NONE', *, *, #15729, .T. ) ;
#23010 = CARTESIAN_POINT ( 'NONE',  ( -208.4459734468149179, 2.143131898507880377E-16, -160.9317124430720298 ) ) ;
#23011 = CARTESIAN_POINT ( 'NONE',  ( 3.975459390375365665, 0.2195152216756870167, 1.992221491942114397E-15 ) ) ;
#23012 = CARTESIAN_POINT ( 'NONE',  ( 0.3910393408562611861, 3.877122853646846945, 9.741991644046958498 ) ) ;
#23013 = DIRECTION ( 'NONE',  ( -1.000000000000000000, -0.000000000000000000, -0.000000000000000000 ) ) ;
#23014 =( BOUNDED_CURVE ( )  B_SPLINE_CURVE ( 3, ( #50509, #3602, #42348, #42848 ),
 .UNSPECIFIED., .F., .F. ) 
 B_SPLINE_CURVE_WITH_KNOTS ( ( 4, 4 ),
 ( 1.570796326794896558, 3.141592653589793116 ),
 .UNSPECIFIED. ) 
 CURVE ( )  GEOMETRIC_REPRESENTATION_ITEM ( )  RATIONAL_B_SPLINE_CURVE ( ( 1.000000000000000000, 0.8047378541243649375, 0.8047378541243649375, 1.000000000000000000 ) ) 
 REPRESENTATION_ITEM ( '' )  );
#23015 = ORIENTED_EDGE ( 'NONE', *, *, #3628, .T. ) ;
#23016 = CARTESIAN_POINT ( 'NONE',  ( -33.14391172085785797, -37.72293746533095060, -8.016098858316199838 ) ) ;
#23017 = EDGE_CURVE ( 'NONE', #28855, #19633, #35633, .T. ) ;
#23019 = ORIENTED_EDGE ( 'NONE', *, *, #24683, .T. ) ;
#23018 = EDGE_CURVE ( 'NONE', #38997, #49549, #16110, .T. ) ;
#23020 = ORIENTED_EDGE ( 'NONE', *, *, #3855, .T. ) ;
#23021 = CARTESIAN_POINT ( 'NONE',  ( 1.111875982684040753, 1.111927553622385378, 9.927288994922816912 ) ) ;
#23022 = EDGE_CURVE ( 'NONE', #46658, #38055, #8690, .T. ) ;
#23023 = EDGE_CURVE ( 'NONE', #24437, #37912, #31014, .T. ) ;
#23024 = ORIENTED_EDGE ( 'NONE', *, *, #6367, .T. ) ;
#23025 = CARTESIAN_POINT ( 'NONE',  ( 35.00000000000122213, 17.00000000000000000, 30.00000000000000000 ) ) ;
#23026 = CYLINDRICAL_SURFACE ( 'NONE', #17543, 2.000000000000001776 ) ;
#23027 = DIRECTION ( 'NONE',  ( 0.000000000000000000, 0.000000000000000000, 1.000000000000000000 ) ) ;
#23028 = EDGE_CURVE ( 'NONE', #6887, #14195, #47106, .T. ) ;
#23029 = EDGE_CURVE ( 'NONE', #50425, #36390, #16976, .T. ) ;
#23030 = CARTESIAN_POINT ( 'NONE',  ( 0.8285222815141930486, 1.889008401827334094, 9.886433018048068178 ) ) ;
#23031 = VERTEX_POINT ( 'NONE', #23814 ) ;
#23032 = VECTOR ( 'NONE', #37826, 1000.000000000000000 ) ;
#23033 = CARTESIAN_POINT ( 'NONE',  ( 33.30402655318503946, 0.000000000000000000, 165.0000000000000000 ) ) ;
#23034 = CARTESIAN_POINT ( 'NONE',  ( -114.9999999999997158, 17.00000000000000000, -84.99999999999998579 ) ) ;
#23035 = CARTESIAN_POINT ( 'NONE',  ( 9.919534718721870092, -1.461167986676253916, 9.524510970297029644 ) ) ;
#23036 = ORIENTED_EDGE ( 'NONE', *, *, #21634, .F. ) ;
#23037 = CARTESIAN_POINT ( 'NONE',  ( -126.6959734468149321, -1.749999999999997335, -79.18171244307201562 ) ) ;
#23038 = CARTESIAN_POINT ( 'NONE',  ( 210.0000000000000568, 0.000000000000000000, 42.56828755692799149 ) ) ;
#23039 = VERTEX_POINT ( 'NONE', #32536 ) ;
#23040 = ORIENTED_EDGE ( 'NONE', *, *, #45901, .F. ) ;
#23041 = ORIENTED_EDGE ( 'NONE', *, *, #29071, .T. ) ;
#23042 = CARTESIAN_POINT ( 'NONE',  ( -20.00000000000001776, 16.00000000000000000, -114.9999999999999858 ) ) ;
#23043 = AXIS2_PLACEMENT_3D ( 'NONE', #26778, #7536, #3671 ) ;
#23044 = CARTESIAN_POINT ( 'NONE',  ( 181.0000000000000000, -268.4999999999999432, -339.9999999999998863 ) ) ;
#23045 = VECTOR ( 'NONE', #8026, 1000.000000000000000 ) ;
#23046 = EDGE_LOOP ( 'NONE', ( #42458, #11448, #17768 ) ) ;
#23047 = ADVANCED_FACE ( 'NONE', ( #25075 ), #16612, .T. ) ;
#23048 = DIRECTION ( 'NONE',  ( 0.000000000000000000, -1.000000000000000000, 0.000000000000000000 ) ) ;
#23049 = CARTESIAN_POINT ( 'NONE',  ( 73.30402655318508209, 1.750000000000009992, 160.8182875569279702 ) ) ;
#23050 = EDGE_CURVE ( 'NONE', #44491, #10704, #43897, .T. ) ;
#23051 = B_SPLINE_CURVE_WITH_KNOTS ( 'NONE', 3,
 ( #5240, #48294, #40655, #5491 ),
 .UNSPECIFIED., .F., .F.,
 ( 4, 4 ),
 ( 5.536300823665787423E-16, 0.009782300387714815831 ),
 .UNSPECIFIED. ) ;
#23052 = CARTESIAN_POINT ( 'NONE',  ( 0.1469336902871260508, 1.496274467947966258, 9.953784399990622589 ) ) ;
#23053 = CARTESIAN_POINT ( 'NONE',  ( 152.2789002873379900, -1.750000000000010214, -78.15658617722490931 ) ) ;
#23054 = EDGE_CURVE ( 'NONE', #49813, #15078, #17115, .T. ) ;
#23055 = CARTESIAN_POINT ( 'NONE',  ( 210.0000000000000568, 0.000000000000000000, 122.5682875569279844 ) ) ;
#23056 = CARTESIAN_POINT ( 'NONE',  ( 32.27890028733795447, -1.750000000000010214, 119.7931612910808781 ) ) ;
#23057 = CARTESIAN_POINT ( 'NONE',  ( 31.55402655318506788, 2.143131898507880377E-16, -160.9317124430720298 ) ) ;
#23058 = DIRECTION ( 'NONE',  ( -1.000000000000000000, 0.000000000000000000, -1.586032872232979935E-16 ) ) ;
#23059 = ORIENTED_EDGE ( 'NONE', *, *, #45434, .T. ) ;
#23060 = CARTESIAN_POINT ( 'NONE',  ( 166.9999999999999716, -256.4999999999999432, -349.9999999999999432 ) ) ;
#23061 = CARTESIAN_POINT ( 'NONE',  ( 210.0000000000000568, 2.143131898507881856E-16, -80.93171244307202983 ) ) ;
#23062 = CYLINDRICAL_SURFACE ( 'NONE', #46134, 4.000000000000003553 ) ;
#23063 = CARTESIAN_POINT ( 'NONE',  ( -204.9459734468149463, 2.143131898507880377E-16, 2.568287556927978166 ) ) ;
#23064 = VERTEX_POINT ( 'NONE', #709 ) ;
#23065 = CARTESIAN_POINT ( 'NONE',  ( -14.48769039275601145, -30.44468701195584970, 8.807470649214879543 ) ) ;
#23066 = ADVANCED_FACE ( 'NONE', ( #21209 ), #40727, .T. ) ;
#23067 = DIRECTION ( 'NONE',  ( 3.172065745548403743E-16, 1.000000000000000000, 0.000000000000000000 ) ) ;
#23068 = AXIS2_PLACEMENT_3D ( 'NONE', #44625, #45382, #44876 ) ;
#23069 = VECTOR ( 'NONE', #4516, 1000.000000000000000 ) ;
#23070 = CARTESIAN_POINT ( 'NONE',  ( 33.30402655318503946, 1.750000000000010658, 80.81828755692798438 ) ) ;
#23071 = CARTESIAN_POINT ( 'NONE',  ( 210.0000000000000568, 0.000000000000000000, -79.18171244307201562 ) ) ;
#23072 = CARTESIAN_POINT ( 'NONE',  ( 71.55402655318505367, 1.025126265847088991, 2.568287556927986159 ) ) ;
#23073 = ORIENTED_EDGE ( 'NONE', *, *, #8929, .F. ) ;
#23074 = SURFACE_SIDE_STYLE ('',( #7696 ) ) ;
#23075 = ORIENTED_EDGE ( 'NONE', *, *, #8107, .T. ) ;
#23076 = VECTOR ( 'NONE', #4400, 1000.000000000000000 ) ;
#23077 = CARTESIAN_POINT ( 'NONE',  ( 49.89397392339123627, -8.245536726716670373, 7.906207997025717304 ) ) ;
#23078 = EDGE_CURVE ( 'NONE', #42417, #40485, #9161, .T. ) ;
#23079 = ORIENTED_EDGE ( 'NONE', *, *, #6489, .F. ) ;
#23080 = CARTESIAN_POINT ( 'NONE',  ( 169.0000000000000568, -166.9999999999999432, -115.0000000000001847 ) ) ;
#23081 = PLANE ( 'NONE',  #16738 ) ;
#23082 = VECTOR ( 'NONE', #7384, 1000.000000000000000 ) ;
#23083 = ORIENTED_EDGE ( 'NONE', *, *, #23108, .F. ) ;
#23084 = CARTESIAN_POINT ( 'NONE',  ( 210.0000000000000568, 0.000000000000000000, 120.8182875569279702 ) ) ;
#23085 = ORIENTED_EDGE ( 'NONE', *, *, #40032, .F. ) ;
#23086 = ADVANCED_FACE ( 'NONE', ( #1480 ), #36903, .T. ) ;
#23087 = ADVANCED_FACE ( 'NONE', ( #4560 ), #7216, .T. ) ;
#23088 = ORIENTED_EDGE ( 'NONE', *, *, #24297, .T. ) ;
#23089 = DIRECTION ( 'NONE',  ( 0.000000000000000000, 0.000000000000000000, 1.000000000000000000 ) ) ;
#23090 = LINE ( 'NONE', #18481, #30623 ) ;
#23091 = ORIENTED_EDGE ( 'NONE', *, *, #48296, .F. ) ;
#23092 = CARTESIAN_POINT ( 'NONE',  ( -215.0000000000000568, 164.9999999999999716, 500.0000000000000000 ) ) ;
#23093 = DIRECTION ( 'NONE',  ( -0.9928768384869219865, 0.000000000000000000, -0.1191452206184307611 ) ) ;
#23094 = CARTESIAN_POINT ( 'NONE',  ( 164.9999999999999716, -256.4999999999999432, -349.9999999999999432 ) ) ;
#23095 = ORIENTED_EDGE ( 'NONE', *, *, #8408, .F. ) ;
#23096 = EDGE_CURVE ( 'NONE', #16958, #26846, #47558, .T. ) ;
#23097 = ORIENTED_EDGE ( 'NONE', *, *, #15224, .F. ) ;
#23098 = CARTESIAN_POINT ( 'NONE',  ( 339.9999999999999432, 183.0000000000000284, -356.0000000000002274 ) ) ;
#23099 = EDGE_CURVE ( 'NONE', #22082, #26763, #8674, .T. ) ;
#23100 = LINE ( 'NONE', #26953, #15758 ) ;
#23101 = ORIENTED_EDGE ( 'NONE', *, *, #6445, .F. ) ;
#23102 = PLANE ( 'NONE',  #552 ) ;
#23103 = CARTESIAN_POINT ( 'NONE',  ( -9.174209336589896679, -3.979181203266159095, 9.646707543097347681 ) ) ;
#23104 =( BOUNDED_CURVE ( )  B_SPLINE_CURVE ( 3, ( #49688, #3276, #14580, #30237 ),
 .UNSPECIFIED., .F., .F. ) 
 B_SPLINE_CURVE_WITH_KNOTS ( ( 4, 4 ),
 ( 1.570796326794896558, 3.141592653589793116 ),
 .UNSPECIFIED. ) 
 CURVE ( )  GEOMETRIC_REPRESENTATION_ITEM ( )  RATIONAL_B_SPLINE_CURVE ( ( 1.000000000000000000, 0.8047378541243649375, 0.8047378541243649375, 1.000000000000000000 ) ) 
 REPRESENTATION_ITEM ( '' )  );
#23105 = ORIENTED_EDGE ( 'NONE', *, *, #20165, .T. ) ;
#23106 = DIRECTION ( 'NONE',  ( 1.000000000000000000, 0.000000000000000000, 0.000000000000000000 ) ) ;
#23107 = CIRCLE ( 'NONE', #1002, 2.000000000000001776 ) ;
#23108 = EDGE_CURVE ( 'NONE', #31779, #614, #44289, .T. ) ;
#23109 = LINE ( 'NONE', #7479, #11169 ) ;
#23110 = VERTEX_POINT ( 'NONE', #973 ) ;
#23111 = AXIS2_PLACEMENT_3D ( 'NONE', #37615, #18326, #9638 ) ;
#23112 = CARTESIAN_POINT ( 'NONE',  ( -124.9459734468149463, 2.143131898507847836E-16, -117.4317124430720725 ) ) ;
#23113 = FACE_OUTER_BOUND ( 'NONE', #1850, .T. ) ;
#23114 = LINE ( 'NONE', #38787, #46712 ) ;
#23115 = CARTESIAN_POINT ( 'NONE',  ( 6.204997580903516941, -7.388441598285492518, 225.0000000000000000 ) ) ;
#23116 = EDGE_CURVE ( 'NONE', #2839, #10058, #32278, .T. ) ;
#23117 = VECTOR ( 'NONE', #7470, 1000.000000000000000 ) ;
#23118 = ORIENTED_EDGE ( 'NONE', *, *, #10249, .F. ) ;
#23119 = CARTESIAN_POINT ( 'NONE',  ( 0.000000000000000000, 0.000000000000000000, 800.0000000000000000 ) ) ;
#23120 = CARTESIAN_POINT ( 'NONE',  ( -34.95136153415531766, 36.40974830873496870, 8.356839323120299312 ) ) ;
#23121 = FACE_OUTER_BOUND ( 'NONE', #9037, .T. ) ;
#23122 = ORIENTED_EDGE ( 'NONE', *, *, #19532, .F. ) ;
#23123 = ORIENTED_EDGE ( 'NONE', *, *, #18583, .F. ) ;
#23124 =( NAMED_UNIT ( * ) SI_UNIT ( $, .STERADIAN. ) SOLID_ANGLE_UNIT ( ) );
#23125 = CARTESIAN_POINT ( 'NONE',  ( -207.7210997126620384, 1.750000000000010436, -80.20683870891910772 ) ) ;
#23126 = CARTESIAN_POINT ( 'NONE',  ( -14.99999999999845812, 17.00000000000000000, 35.00000000000000000 ) ) ;
#23127 =( LENGTH_UNIT ( ) NAMED_UNIT ( * ) SI_UNIT ( .MILLI., .METRE. ) );
#23128 = LINE ( 'NONE', #42778, #19230 ) ;
#23129 = PLANE ( 'NONE',  #33826 ) ;
#23130 = ORIENTED_EDGE ( 'NONE', *, *, #3312, .F. ) ;
#23131 = CARTESIAN_POINT ( 'NONE',  ( 168.9999999999999716, -5.999999999999950262, -350.0000000000001705 ) ) ;
#23132 = DIRECTION ( 'NONE',  ( -0.000000000000000000, -0.000000000000000000, -1.000000000000000000 ) ) ;
#23133 = CARTESIAN_POINT ( 'NONE',  ( 2.188678504086826848, -0.3267089737525829540, 9.881002359080282460 ) ) ;
#23134 = ORIENTED_EDGE ( 'NONE', *, *, #16785, .F. ) ;
#23135 = CARTESIAN_POINT ( 'NONE',  ( 113.3040265531850537, 1.749999999999996891, -159.1817124430720298 ) ) ;
#23136 = AXIS2_PLACEMENT_3D ( 'NONE', #16623, #32293, #12774 ) ;
#23137 = DIRECTION ( 'NONE',  ( -0.000000000000000000, -1.000000000000000000, -0.000000000000000000 ) ) ;
#23138 = EDGE_LOOP ( 'NONE', ( #11674, #21189, #41830, #3742 ) ) ;
#23139 = CARTESIAN_POINT ( 'NONE',  ( 210.0000000000000568, 0.000000000000000000, -39.18171244307202983 ) ) ;
#23140 = CIRCLE ( 'NONE', #9231, 2.000000000000001776 ) ;
#23141 = CARTESIAN_POINT ( 'NONE',  ( 0.000000000000000000, 0.000000000000000000, 800.0000000000000000 ) ) ;
#23142 = CARTESIAN_POINT ( 'NONE',  ( 113.3040265531850537, 1.749999999999996891, 0.8182875569279768335 ) ) ;
#23143 = ORIENTED_EDGE ( 'NONE', *, *, #16494, .T. ) ;
#23144 = B_SPLINE_CURVE_WITH_KNOTS ( 'NONE', 3,
 ( #25660, #48194, #41052, #49205 ),
 .UNSPECIFIED., .F., .F.,
 ( 4, 4 ),
 ( 0.001403500796105026753, 0.001586656765098990764 ),
 .UNSPECIFIED. ) ;
#23145 = VECTOR ( 'NONE', #21828, 1000.000000000000000 ) ;
#23146 = EDGE_CURVE ( 'NONE', #48817, #11294, #44045, .T. ) ;
#23147 = CARTESIAN_POINT ( 'NONE',  ( -20.00000000000003197, 17.00000000000000000, -114.9999999999999858 ) ) ;
#23148 = ADVANCED_FACE ( 'NONE', ( #5051 ), #14007, .T. ) ;
#23149 = AXIS2_PLACEMENT_3D ( 'NONE', #16263, #44197, #47271 ) ;
#23150 = DIRECTION ( 'NONE',  ( -1.000000000000000000, 0.000000000000000000, -0.000000000000000000 ) ) ;
#23151 = ORIENTED_EDGE ( 'NONE', *, *, #41866, .T. ) ;
#23152 = CARTESIAN_POINT ( 'NONE',  ( -8.445973446814962315, 1.025126265847096985, -0.9317124430720461481 ) ) ;
#23153 = CARTESIAN_POINT ( 'NONE',  ( 33.43156050989131955, -4.370686678976570150, 8.807470649214879543 ) ) ;
#23154 = DIRECTION ( 'NONE',  ( 0.000000000000000000, 0.000000000000000000, 1.000000000000000000 ) ) ;
#23155 = ORIENTED_EDGE ( 'NONE', *, *, #29637, .F. ) ;
#23156 = ADVANCED_FACE ( 'NONE', ( #6067 ), #17615, .T. ) ;
#23157 = ORIENTED_EDGE ( 'NONE', *, *, #10322, .T. ) ;
#23158 = PLANE ( 'NONE',  #21027 ) ;
#23159 = CARTESIAN_POINT ( 'NONE',  ( -4.207128120815918256E-14, 3.058192377181588826E-14, 10.00000000000000000 ) ) ;
#23160 = EDGE_CURVE ( 'NONE', #45145, #19313, #35988, .T. ) ;
#23161 = EDGE_CURVE ( 'NONE', #5437, #3794, #49377, .T. ) ;
#23162 =( BOUNDED_CURVE ( )  B_SPLINE_CURVE ( 3, ( #41951, #25800, #49839, #26558 ),
 .UNSPECIFIED., .F., .F. ) 
 B_SPLINE_CURVE_WITH_KNOTS ( ( 4, 4 ),
 ( 3.141592653589793116, 4.712388980384689674 ),
 .UNSPECIFIED. ) 
 CURVE ( )  GEOMETRIC_REPRESENTATION_ITEM ( )  RATIONAL_B_SPLINE_CURVE ( ( 1.000000000000000000, 0.8047378541243649375, 0.8047378541243649375, 1.000000000000000000 ) ) 
 REPRESENTATION_ITEM ( '' )  );
#23163 = ORIENTED_EDGE ( 'NONE', *, *, #21429, .F. ) ;
#23164 = EDGE_LOOP ( 'NONE', ( #33584, #33238, #48198, #35002 ) ) ;
#23165 = CARTESIAN_POINT ( 'NONE',  ( 210.0000000000000568, 2.143131898507881856E-16, 79.06828755692797017 ) ) ;
#23166 = DIRECTION ( 'NONE',  ( -0.000000000000000000, -1.000000000000000000, 2.537652627714643577E-15 ) ) ;
#23167 = DIRECTION ( 'NONE',  ( -0.000000000000000000, -0.000000000000000000, -1.000000000000000000 ) ) ;
#23168 = ORIENTED_EDGE ( 'NONE', *, *, #6764, .T. ) ;
#23169 = CARTESIAN_POINT ( 'NONE',  ( -10.30302290646040575, -13.08520913973572419, -9.683996418299976483 ) ) ;
#23170 = EDGE_CURVE ( 'NONE', #47056, #13420, #16079, .T. ) ;
#23171 = ORIENTED_EDGE ( 'NONE', *, *, #25288, .T. ) ;
#23172 =( BOUNDED_CURVE ( )  B_SPLINE_CURVE ( 3, ( #26741, #33936, #15189, #38557 ),
 .UNSPECIFIED., .F., .F. ) 
 B_SPLINE_CURVE_WITH_KNOTS ( ( 4, 4 ),
 ( 0.000000000000000000, 1.570796326794896558 ),
 .UNSPECIFIED. ) 
 CURVE ( )  GEOMETRIC_REPRESENTATION_ITEM ( )  RATIONAL_B_SPLINE_CURVE ( ( 1.000000000000000000, 0.8047378541243649375, 0.8047378541243649375, 1.000000000000000000 ) ) 
 REPRESENTATION_ITEM ( '' )  );
#23173 = VECTOR ( 'NONE', #20583, 999.9999999999998863 ) ;
#23174 = ADVANCED_FACE ( 'NONE', ( #48871 ), #34682, .T. ) ;
#23175 = PLANE ( 'NONE',  #18133 ) ;
#23176 = CARTESIAN_POINT ( 'NONE',  ( 181.0000000000000000, -95.49999999999998579, -350.0000000000001705 ) ) ;
#23177 = CYLINDRICAL_SURFACE ( 'NONE', #14049, 4.000000000000003553 ) ;
#23178 = VERTEX_POINT ( 'NONE', #33788 ) ;
#23179 = EDGE_LOOP ( 'NONE', ( #527, #46535, #47306, #1081, #4131, #26572 ) ) ;
#23180 = VERTEX_POINT ( 'NONE', #18611 ) ;
#23181 = DIRECTION ( 'NONE',  ( 0.000000000000000000, 0.000000000000000000, -1.000000000000000000 ) ) ;
#23182 = VECTOR ( 'NONE', #14287, 1000.000000000000000 ) ;
#23183 = CARTESIAN_POINT ( 'NONE',  ( -14.29087950072019098, -9.652079258044555132, 8.727788335465566760 ) ) ;
#23184 = EDGE_LOOP ( 'NONE', ( #17502, #32904, #42528, #38393 ) ) ;
#23185 = CARTESIAN_POINT ( 'NONE',  ( -86.69597344681494633, -1.750000000000010214, 40.81828755692798438 ) ) ;
#23186 = ORIENTED_EDGE ( 'NONE', *, *, #6265, .T. ) ;
#23187 = CARTESIAN_POINT ( 'NONE',  ( -14.99999999999937472, 17.00000000000000000, -30.00000000000000000 ) ) ;
#23188 = EDGE_LOOP ( 'NONE', ( #3125, #26392, #40057, #710, #25819, #23594, #11412, #37632 ) ) ;
#23189 = CARTESIAN_POINT ( 'NONE',  ( 169.0000000000000000, 2.775557561562891351E-14, -95.00000000000014211 ) ) ;
#23190 = DIRECTION ( 'NONE',  ( -1.000000000000000000, -0.000000000000000000, -0.000000000000000000 ) ) ;
#23191 = VECTOR ( 'NONE', #45512, 1000.000000000000000 ) ;
#23192 = FACE_OUTER_BOUND ( 'NONE', #39928, .T. ) ;
#23193 = ORIENTED_EDGE ( 'NONE', *, *, #1519, .F. ) ;
#23194 = ORIENTED_EDGE ( 'NONE', *, *, #5261, .T. ) ;
#23195 = CARTESIAN_POINT ( 'NONE',  ( 135.0000000000012790, 17.00000000000000000, 5.000000000000004441 ) ) ;
#23196 = EDGE_CURVE ( 'NONE', #44491, #609, #9915, .T. ) ;
#23197 = DIRECTION ( 'NONE',  ( 0.000000000000000000, 0.000000000000000000, -1.000000000000000000 ) ) ;
#23198 = B_SPLINE_SURFACE_WITH_KNOTS ( 'NONE', 3, 3, ( 
 ( #38064, #30358, #38580, #26500 ),
 ( #2875, #33953, #14695, #10845 ),
 ( #42137, #7002, #22646, #50046 ),
 ( #38325, #3134, #34731, #18784 ) ),
 .UNSPECIFIED., .F., .F., .F.,
 ( 4, 4 ),
 ( 4, 4 ),
 ( 0.000000000000000000, 1.000000000000000000 ),
 ( 0.000000000000000000, 1.000000000000000000 ),
 .UNSPECIFIED. ) ;
#23199 = LINE ( 'NONE', #22692, #18708 ) ;
#23200 = CARTESIAN_POINT ( 'NONE',  ( 32.27890028733795447, -1.750000000000009548, -40.20683870891912193 ) ) ;
#23201 = EDGE_CURVE ( 'NONE', #42197, #43746, #40657, .T. ) ;
#23202 = CARTESIAN_POINT ( 'NONE',  ( 342.0000000000000568, 169.0000000000000000, 349.9999999999998863 ) ) ;
#23203 = DIRECTION ( 'NONE',  ( 0.000000000000000000, 0.000000000000000000, -1.000000000000000000 ) ) ;
#23204 = ORIENTED_EDGE ( 'NONE', *, *, #21086, .T. ) ;
#23205 = CARTESIAN_POINT ( 'NONE',  ( -10.50000000000003730, 13.59802227364767546, -19.51251772323704969 ) ) ;
#23206 = DIRECTION ( 'NONE',  ( 0.000000000000000000, 0.000000000000000000, -1.000000000000000000 ) ) ;
#23207 = ORIENTED_EDGE ( 'NONE', *, *, #13619, .F. ) ;
#23208 = LINE ( 'NONE', #3967, #36871 ) ;
#23209 = PLANE ( 'NONE',  #19272 ) ;
#23210 = VECTOR ( 'NONE', #31232, 1000.000000000000000 ) ;
#23211 = ORIENTED_EDGE ( 'NONE', *, *, #6631, .T. ) ;
#23212 = ORIENTED_EDGE ( 'NONE', *, *, #40939, .T. ) ;
#23213 = DIRECTION ( 'NONE',  ( -1.000000000000000000, 0.000000000000000000, 0.000000000000000000 ) ) ;
#23214 = VECTOR ( 'NONE', #20812, 1000.000000000000000 ) ;
#23215 = CARTESIAN_POINT ( 'NONE',  ( 3.996390545799824334, -16.57371371864897469, 8.953103998512858652 ) ) ;
#23216 = ORIENTED_EDGE ( 'NONE', *, *, #2631, .F. ) ;
#23217 = AXIS2_PLACEMENT_3D ( 'NONE', #41632, #10344, #45192 ) ;
#23218 = ORIENTED_EDGE ( 'NONE', *, *, #11835, .T. ) ;
#23219 = CARTESIAN_POINT ( 'NONE',  ( -25.79500241909648395, 7.611558401714507482, 230.0000000000000000 ) ) ;
#23220 = CARTESIAN_POINT ( 'NONE',  ( 4.999999999999999112, -175.0000000000000284, -353.7500000000001705 ) ) ;
#23221 = CARTESIAN_POINT ( 'NONE',  ( -3.229232847726260403, 16.57333684275945629, 9.178419661560148768 ) ) ;
#23222 = ORIENTED_EDGE ( 'NONE', *, *, #49914, .T. ) ;
#23223 = ORIENTED_EDGE ( 'NONE', *, *, #22360, .F. ) ;
#23224 = ADVANCED_FACE ( 'NONE', ( #45290 ), #14520, .F. ) ;
#23225 = VERTEX_POINT ( 'NONE', #30432 ) ;
#23226 = LINE ( 'NONE', #30955, #44676 ) ;
#23227 = CARTESIAN_POINT ( 'NONE',  ( 1.419290803332528661, 0.2086015876289408766, 9.950105812514292936 ) ) ;
#23228 = EDGE_LOOP ( 'NONE', ( #35642, #2958, #19510, #27205, #43533, #16807 ) ) ;
#23229 = VECTOR ( 'NONE', #41160, 1000.000000000000000 ) ;
#23230 = CARTESIAN_POINT ( 'NONE',  ( 1.072341519475944915, -1.326978504731018083, 9.912102921405038458 ) ) ;
#23231 = CARTESIAN_POINT ( 'NONE',  ( 23.79193388295309219, 28.98609808355011452, -9.422646554964176246 ) ) ;
#23232 = ORIENTED_EDGE ( 'NONE', *, *, #20481, .T. ) ;
#23233 = ORIENTED_EDGE ( 'NONE', *, *, #20229, .T. ) ;
#23234 = CARTESIAN_POINT ( 'NONE',  ( -6.695973446814940111, 0.000000000000000000, 165.0000000000000000 ) ) ;
#23235 = SURFACE_STYLE_USAGE ( .BOTH. , #7602 ) ;
#23236 = CARTESIAN_POINT ( 'NONE',  ( 191.5540265531851105, 0.000000000000000000, -117.4317124430720725 ) ) ;
#23237 = ORIENTED_EDGE ( 'NONE', *, *, #14934, .F. ) ;
#23238 = ORIENTED_EDGE ( 'NONE', *, *, #48813, .T. ) ;
#23239 = CARTESIAN_POINT ( 'NONE',  ( 44.99506233596247995, 23.32283626942318833, 7.455576670931136185 ) ) ;
#23240 = DIRECTION ( 'NONE',  ( 3.614007241618348278E-16, 1.000000000000000000, 0.000000000000000000 ) ) ;
#23241 = VERTEX_POINT ( 'NONE', #46037 ) ;
#23242 = DIRECTION ( 'NONE',  ( 0.4374820812098862421, -0.3178493372392685590, -0.8411784753765542133 ) ) ;
#23243 = CYLINDRICAL_SURFACE ( 'NONE', #34235, 1.750000000000001554 ) ;
#23244 = FACE_OUTER_BOUND ( 'NONE', #14133, .T. ) ;
#23245 = VECTOR ( 'NONE', #34404, 1000.000000000000000 ) ;
#23246 = CARTESIAN_POINT ( 'NONE',  ( 12.15085308559846844, -11.68662139125803989, 2.590526750877053086 ) ) ;
#23247 = ORIENTED_EDGE ( 'NONE', *, *, #24617, .T. ) ;
#23248 = VECTOR ( 'NONE', #13030, 1000.000000000000000 ) ;
#23249 = CARTESIAN_POINT ( 'NONE',  ( 193.3040265531851105, -1.750000000000009992, -159.1817124430720298 ) ) ;
#23250 = CARTESIAN_POINT ( 'NONE',  ( -6.695973446814940111, 1.750000000000023759, 40.81828755692798438 ) ) ;
#23251 = CARTESIAN_POINT ( 'NONE',  ( -69.99999999999879208, 16.00000000000000000, 5.000000000000004441 ) ) ;
#23252=STYLED_ITEM('',(#50747),#39816);
#23253 = EDGE_CURVE ( 'NONE', #11545, #26016, #2224, .T. ) ;
#23254 = AXIS2_PLACEMENT_3D ( 'NONE', #15625, #31297, #50473 ) ;
#23255 = FACE_OUTER_BOUND ( 'NONE', #48985, .T. ) ;
#23256 = VERTEX_POINT ( 'NONE', #37901 ) ;
#23257 = CARTESIAN_POINT ( 'NONE',  ( 166.9999999999999716, -93.50000000000005684, -340.0000000000001137 ) ) ;
#23258 = CARTESIAN_POINT ( 'NONE',  ( -33.43156050989129824, 4.370686678976795747, 8.807470649214879543 ) ) ;
#23259 = CARTESIAN_POINT ( 'NONE',  ( -14.49999999999999822, -46.40197772635230677, 5.828307196921268307 ) ) ;
#23260 = ORIENTED_EDGE ( 'NONE', *, *, #31803, .T. ) ;
#23261 = SURFACE_SIDE_STYLE ('',( #47338 ) ) ;
#23262 = AXIS2_PLACEMENT_3D ( 'NONE', #48635, #25097, #1496 ) ;
#23263 = DIRECTION ( 'NONE',  ( 1.000000000000000000, 0.000000000000000000, 0.000000000000000000 ) ) ;
#23264 = ORIENTED_EDGE ( 'NONE', *, *, #35405, .F. ) ;
#23265 = CARTESIAN_POINT ( 'NONE',  ( -86.69597344681494633, -1.750000000000010658, -79.18171244307201562 ) ) ;
#23266 = DIRECTION ( 'NONE',  ( 0.000000000000000000, 0.000000000000000000, 1.000000000000000000 ) ) ;
#23267 = CARTESIAN_POINT ( 'NONE',  ( 185.0000000000000000, -93.49999999999998579, -340.0000000000001137 ) ) ;
#23268 = CARTESIAN_POINT ( 'NONE',  ( -44.94597344681493922, 2.143131898507880377E-16, 122.5682875569279702 ) ) ;
#23269 = ORIENTED_EDGE ( 'NONE', *, *, #718, .T. ) ;
#23270 = FACE_OUTER_BOUND ( 'NONE', #37691, .T. ) ;
#23271 = VERTEX_POINT ( 'NONE', #41723 ) ;
#23272 = ORIENTED_EDGE ( 'NONE', *, *, #28385, .T. ) ;
#23273 = CARTESIAN_POINT ( 'NONE',  ( -88.44597344681497475, 0.000000000000000000, -40.93171244307205825 ) ) ;
#23274 = ORIENTED_EDGE ( 'NONE', *, *, #7416, .F. ) ;
#23276 = CIRCLE ( 'NONE', #41308, 10.00000000000000000 ) ;
#23275 = FACE_OUTER_BOUND ( 'NONE', #21976, .T. ) ;
#23277 = CARTESIAN_POINT ( 'NONE',  ( -49.46074318306825290, 9.578883844007165749, 8.807470649214879543 ) ) ;
#23278 = VECTOR ( 'NONE', #35312, 1000.000000000000000 ) ;
#23279 = EDGE_CURVE ( 'NONE', #11818, #33150, #45041, .T. ) ;
#23280 = VECTOR ( 'NONE', #19801, 1000.000000000000000 ) ;
#23281 = CARTESIAN_POINT ( 'NONE',  ( 0.4402948852767718524, -2.015117899693914527, 9.894754715216725671 ) ) ;
#23282 = ORIENTED_EDGE ( 'NONE', *, *, #44608, .F. ) ;
#23284 = B_SPLINE_CURVE_WITH_KNOTS ( 'NONE', 3,
 ( #5537, #2205, #32248, #1456, #47842, #36362 ),
 .UNSPECIFIED., .F., .F.,
 ( 4, 2, 4 ),
 ( 8.498374721940738929E-18, 0.009877169331704831884, 0.01975433866340964989 ),
 .UNSPECIFIED. ) ;
#23283 = CIRCLE ( 'NONE', #1196, 2.000000000000001776 ) ;
#23285 = EDGE_CURVE ( 'NONE', #40502, #40611, #49126, .T. ) ;
#23286 = LINE ( 'NONE', #12498, #2865 ) ;
#23287 = DIRECTION ( 'NONE',  ( -1.000000000000000000, 0.000000000000000000, 0.000000000000000000 ) ) ;
#23288 = EDGE_CURVE ( 'NONE', #47457, #32283, #21971, .T. ) ;
#23289 = CARTESIAN_POINT ( 'NONE',  ( -208.4459734468149463, 0.000000000000000000, 79.06828755692797017 ) ) ;
#23290 = EDGE_LOOP ( 'NONE', ( #41779, #42846, #35033, #50109 ) ) ;
#23291 = CARTESIAN_POINT ( 'NONE',  ( 35.51846793572394034, -35.99772139009119343, 7.906207997025717304 ) ) ;
#23292 = CYLINDRICAL_SURFACE ( 'NONE', #39293, 1.750000000000036193 ) ;
#23293 = ORIENTED_EDGE ( 'NONE', *, *, #43836, .T. ) ;
#23294 = ORIENTED_EDGE ( 'NONE', *, *, #10781, .T. ) ;
#23295 = ORIENTED_EDGE ( 'NONE', *, *, #24735, .T. ) ;
#23296 = DIRECTION ( 'NONE',  ( -0.000000000000000000, -1.000000000000000000, -0.000000000000000000 ) ) ;
#23297 = EDGE_CURVE ( 'NONE', #15732, #20063, #28883, .T. ) ;
#23298 = EDGE_CURVE ( 'NONE', #18793, #3991, #39159, .T. ) ;
#23299 = DIRECTION ( 'NONE',  ( 0.000000000000000000, 0.000000000000000000, 1.000000000000000000 ) ) ;
#23300 = PRODUCT_DEFINITION_SHAPE ( 'NONE', 'NONE',  #13035 ) ;
#23301 = ORIENTED_EDGE ( 'NONE', *, *, #25881, .F. ) ;
#23302 = FACE_OUTER_BOUND ( 'NONE', #14771, .T. ) ;
#23303 = DIRECTION ( 'NONE',  ( 0.000000000000000000, 0.000000000000000000, -1.000000000000000000 ) ) ;
#23304 = EDGE_CURVE ( 'NONE', #7866, #1161, #11437, .T. ) ;
#23305 =( BOUNDED_CURVE ( )  B_SPLINE_CURVE ( 3, ( #27813, #43448, #50600, #15747 ),
 .UNSPECIFIED., .F., .F. ) 
 B_SPLINE_CURVE_WITH_KNOTS ( ( 4, 4 ),
 ( 1.570796326794896558, 3.141592653589793116 ),
 .UNSPECIFIED. ) 
 CURVE ( )  GEOMETRIC_REPRESENTATION_ITEM ( )  RATIONAL_B_SPLINE_CURVE ( ( 1.000000000000000000, 0.8047378541243649375, 0.8047378541243649375, 1.000000000000000000 ) ) 
 REPRESENTATION_ITEM ( '' )  );
#23306 = CARTESIAN_POINT ( 'NONE',  ( -45.42829307628559832, -21.98948915213271960, 8.356839323120299312 ) ) ;
#23307 = AXIS2_PLACEMENT_3D ( 'NONE', #50022, #27498, #34704 ) ;
#23308 = CARTESIAN_POINT ( 'NONE',  ( -128.4459734468149179, 0.000000000000000000, -157.4317124430720582 ) ) ;
#23309 = CARTESIAN_POINT ( 'NONE',  ( 210.0000000000000568, 0.000000000000000000, 160.8182875569279702 ) ) ;
#23310 = CARTESIAN_POINT ( 'NONE',  ( 6.174150299305392053, -50.00000000000000711, 8.807470649214879543 ) ) ;
#23311 = LINE ( 'NONE', #38986, #29835 ) ;
#23312 = VECTOR ( 'NONE', #14745, 1000.000000000000000 ) ;
#23313 = FACE_OUTER_BOUND ( 'NONE', #18183, .T. ) ;
#23314 = CARTESIAN_POINT ( 'NONE',  ( 31.55402655318503236, -1.025126265847089213, -160.9317124430720014 ) ) ;
#23315 = CARTESIAN_POINT ( 'NONE',  ( -168.4459734468149463, 0.000000000000000000, 119.0682875569279702 ) ) ;
#23316 = EDGE_CURVE ( 'NONE', #22117, #26100, #41489, .T. ) ;
#23317 = EDGE_CURVE ( 'NONE', #28357, #11655, #38398, .T. ) ;
#23318 = VERTEX_POINT ( 'NONE', #1103 ) ;
#23319 = CARTESIAN_POINT ( 'NONE',  ( -8.445973446814964092, 1.025126265847097207, 82.56828755692798438 ) ) ;
#23320 = DIRECTION ( 'NONE',  ( -1.000000000000000000, -0.000000000000000000, -0.000000000000000000 ) ) ;
#23321 = EDGE_CURVE ( 'NONE', #31351, #11996, #6570, .T. ) ;
#23322 = EDGE_CURVE ( 'NONE', #27491, #20536, #39865, .T. ) ;
#23323 = VECTOR ( 'NONE', #8542, 1000.000000000000000 ) ;
#23324 = CARTESIAN_POINT ( 'NONE',  ( -128.4459734468149179, 0.000000000000000000, -120.9317124430720156 ) ) ;
#23325 = CARTESIAN_POINT ( 'NONE',  ( -46.11867747200561496, 19.86470446310265103, -8.016098858316205167 ) ) ;
#23326 = ORIENTED_EDGE ( 'NONE', *, *, #873, .T. ) ;
#23327 = FACE_BOUND ( 'NONE', #13634, .T. ) ;
#23328 = EDGE_CURVE ( 'NONE', #26449, #18811, #34542, .T. ) ;
#23329 =( BOUNDED_CURVE ( )  B_SPLINE_CURVE ( 3, ( #956, #16853, #5033, #32754 ),
 .UNSPECIFIED., .F., .F. ) 
 B_SPLINE_CURVE_WITH_KNOTS ( ( 4, 4 ),
 ( 3.141592653589793116, 4.712388980384689674 ),
 .UNSPECIFIED. ) 
 CURVE ( )  GEOMETRIC_REPRESENTATION_ITEM ( )  RATIONAL_B_SPLINE_CURVE ( ( 1.000000000000000000, 0.8047378541243649375, 0.8047378541243649375, 1.000000000000000000 ) ) 
 REPRESENTATION_ITEM ( '' )  );
#23330 = CARTESIAN_POINT ( 'NONE',  ( 344.0000000000000000, -167.0000000000001137, -342.0000000000002842 ) ) ;
#23331 = CARTESIAN_POINT ( 'NONE',  ( 191.5540265531851105, 0.000000000000000000, 165.0000000000000000 ) ) ;
#23332 = VECTOR ( 'NONE', #9929, 1000.000000000000000 ) ;
#23333 = CARTESIAN_POINT ( 'NONE',  ( 152.2789002873379900, -1.750000000000009548, 161.8434138227750907 ) ) ;
#23334 = ORIENTED_EDGE ( 'NONE', *, *, #49905, .F. ) ;
#23335 = ORIENTED_EDGE ( 'NONE', *, *, #11099, .F. ) ;
#23336 = CARTESIAN_POINT ( 'NONE',  ( 0.1287570809895575430, 0.3962735484563150168, 10.00000000000000000 ) ) ;
#23337 = EDGE_LOOP ( 'NONE', ( #7978, #19240, #44588, #13515, #47528, #18239 ) ) ;
#23338 = CARTESIAN_POINT ( 'NONE',  ( 339.9999999999998863, -185.0000000000001421, 355.9999999999997726 ) ) ;
#23339 = CARTESIAN_POINT ( 'NONE',  ( -10.49999999999999467, -46.01315789473684248, -5.916985404131818171 ) ) ;
#23340 = ORIENTED_EDGE ( 'NONE', *, *, #26476, .T. ) ;
#23341 = CARTESIAN_POINT ( 'NONE',  ( 340.0000000000000568, 185.0000000000000284, 343.9999999999997726 ) ) ;
#23342 = ADVANCED_FACE ( 'NONE', ( #36263 ), #8804, .T. ) ;
#23343 = ORIENTED_EDGE ( 'NONE', *, *, #17379, .T. ) ;
#23344 = AXIS2_PLACEMENT_3D ( 'NONE', #40765, #34088, #18408 ) ;
#23345 = EDGE_CURVE ( 'NONE', #16751, #5777, #50124, .T. ) ;
#23346 = EDGE_CURVE ( 'NONE', #45648, #4709, #30692, .T. ) ;
#23347 = VERTEX_POINT ( 'NONE', #46297 ) ;
#23348 = CARTESIAN_POINT ( 'NONE',  ( -15.00000000000000000, -46.01315789473684248, 5.916985404131813731 ) ) ;
#23349 = CARTESIAN_POINT ( 'NONE',  ( -70.00000000000002842, 16.00000000000000000, -90.00000000000000000 ) ) ;
#23350 =( REPRESENTATION_RELATIONSHIP ('NONE','NONE', #45699, #39915 ) REPRESENTATION_RELATIONSHIP_WITH_TRANSFORMATION ( #14604 )SHAPE_REPRESENTATION_RELATIONSHIP( ) );
#23351 = VECTOR ( 'NONE', #12641, 1000.000000000000114 ) ;
#23352 = VECTOR ( 'NONE', #5908, 1000.000000000000000 ) ;
#23353 = ORIENTED_EDGE ( 'NONE', *, *, #48359, .F. ) ;
#23354 = DIRECTION ( 'NONE',  ( -1.000000000000000000, -0.000000000000000000, -0.000000000000000000 ) ) ;
#23355 = CYLINDRICAL_SURFACE ( 'NONE', #6250, 4.000000000000003553 ) ;
#23356 = ADVANCED_FACE ( 'NONE', ( #42715 ), #7592, .F. ) ;
#23357 = CARTESIAN_POINT ( 'NONE',  ( -177.4999999999999716, 112.5000000000000000, -10.00000000000000000 ) ) ;
#23358 = VERTEX_POINT ( 'NONE', #32397 ) ;
#23359 = FACE_OUTER_BOUND ( 'NONE', #17606, .T. ) ;
#23360 = EDGE_CURVE ( 'NONE', #4790, #30864, #15089, .T. ) ;
#23361 = CARTESIAN_POINT ( 'NONE',  ( 339.9999999999999432, 181.0000000000000284, -356.0000000000002274 ) ) ;
#23362 = PRESENTATION_LAYER_ASSIGNMENT (  '', '', ( #25019 ) ) ;
#23363 = VERTEX_POINT ( 'NONE', #3468 ) ;
#23364 = DIRECTION ( 'NONE',  ( 1.000000000000000000, 0.000000000000000000, 0.000000000000000000 ) ) ;
#23365 = VECTOR ( 'NONE', #30508, 1000.000000000000000 ) ;
#23366 = DIRECTION ( 'NONE',  ( 1.000000000000000000, 0.000000000000000000, 0.000000000000000000 ) ) ;
#23367 = ORIENTED_EDGE ( 'NONE', *, *, #34932, .F. ) ;
#23368 = DIRECTION ( 'NONE',  ( 1.000000000000000000, 0.000000000000000000, 0.000000000000000000 ) ) ;
#23369 = LINE ( 'NONE', #38993, #25725 ) ;
#23370 = DIRECTION ( 'NONE',  ( 6.203854594147707562E-25, -2.067951531382569187E-25, 1.000000000000000000 ) ) ;
#23371 = ORIENTED_EDGE ( 'NONE', *, *, #36689, .T. ) ;
#23372 = EDGE_CURVE ( 'NONE', #30042, #43155, #20034, .T. ) ;
#23373 = CARTESIAN_POINT ( 'NONE',  ( 210.0000000000000568, 0.000000000000000000, 120.8182875569279702 ) ) ;
#23374 = FACE_OUTER_BOUND ( 'NONE', #24657, .T. ) ;
#23375 = DIRECTION ( 'NONE',  ( 0.4436251537532894806, 0.000000000000000000, -0.8962124318248270161 ) ) ;
#23376 = CARTESIAN_POINT ( 'NONE',  ( 71.55402655318505367, 0.000000000000000000, -120.9317124430720725 ) ) ;
#23377 = VERTEX_POINT ( 'NONE', #7860 ) ;
#23378 = EDGE_CURVE ( 'NONE', #9039, #29500, #27343, .T. ) ;
#23379 = CARTESIAN_POINT ( 'NONE',  ( 0.3862712429686727678, 1.188820645368945605, 3.333333333333333481 ) ) ;
#23380 = SURFACE_SIDE_STYLE ('',( #19264 ) ) ;
#23381 = CARTESIAN_POINT ( 'NONE',  ( 20.40054609052976531, -26.26366202847973597, -3.760136334089591248 ) ) ;
#23382 = ORIENTED_EDGE ( 'NONE', *, *, #43549, .F. ) ;
#23383 = VERTEX_POINT ( 'NONE', #23503 ) ;
#23384 = CARTESIAN_POINT ( 'NONE',  ( 9.999999999999998224, 8.486842105263161073, -25.00000000000000000 ) ) ;
#23385 = CARTESIAN_POINT ( 'NONE',  ( 341.6568542494923690, -164.9999999999999716, 339.9999999999998295 ) ) ;
#23386 = ADVANCED_FACE ( 'NONE', ( #47995 ), #44664, .T. ) ;
#23387 = VECTOR ( 'NONE', #5235, 1000.000000000000000 ) ;
#23388 = EDGE_CURVE ( 'NONE', #27797, #49664, #44175, .T. ) ;
#23389 = PRESENTATION_STYLE_ASSIGNMENT (( #2856 ) ) ;
#23390 = LINE ( 'NONE', #23643, #38898 ) ;
#23391 = VECTOR ( 'NONE', #32057, 1000.000000000000000 ) ;
#23392 = CARTESIAN_POINT ( 'NONE',  ( 155.0540265531850537, -1.025126265847089657, -120.9317124430720440 ) ) ;
#23393 = ORIENTED_EDGE ( 'NONE', *, *, #11712, .T. ) ;
#23394 = EDGE_CURVE ( 'NONE', #35332, #5910, #34147, .T. ) ;
#23395 = CARTESIAN_POINT ( 'NONE',  ( -69.99999999999909051, 17.00000000000000000, 0.000000000000000000 ) ) ;
#23396 = EDGE_CURVE ( 'NONE', #43423, #34859, #524, .T. ) ;
#23397 = CIRCLE ( 'NONE', #34068, 4.000000000000003553 ) ;
#23398 = CARTESIAN_POINT ( 'NONE',  ( -0.3862712429686809279, -1.188820645368943163, 3.333333333333333481 ) ) ;
#23399 = CARTESIAN_POINT ( 'NONE',  ( 339.9999999999999432, -164.9999999999999432, -356.0000000000002274 ) ) ;
#23400 = PRESENTATION_STYLE_ASSIGNMENT (( #15956 ) ) ;
#23401 = ADVANCED_FACE ( 'NONE', ( #10049 ), #16995, .F. ) ;
#23402 = PRESENTATION_LAYER_ASSIGNMENT (  '', '', ( #11089 ) ) ;
#23403 = ORIENTED_EDGE ( 'NONE', *, *, #7437, .F. ) ;
#23404 = CARTESIAN_POINT ( 'NONE',  ( 0.000000000000000000, 165.2000000000000171, 340.1999999999997044 ) ) ;
#23405 = ORIENTED_EDGE ( 'NONE', *, *, #35355, .T. ) ;
#23406 = VECTOR ( 'NONE', #3047, 1000.000000000000000 ) ;
#23407 = CARTESIAN_POINT ( 'NONE',  ( -88.44597344681497475, 0.000000000000000000, -40.93171244307205825 ) ) ;
#23408 = VECTOR ( 'NONE', #5122, 1000.000000000000000 ) ;
#23409 = LINE ( 'NONE', #15699, #44996 ) ;
#23410 = EDGE_LOOP ( 'NONE', ( #7, #50711, #36751, #3108, #4863, #38280 ) ) ;
#23411 = DIRECTION ( 'NONE',  ( -0.000000000000000000, -0.000000000000000000, -1.000000000000000000 ) ) ;
#23412 = FACE_OUTER_BOUND ( 'NONE', #16784, .T. ) ;
#23413 = VECTOR ( 'NONE', #17156, 1000.000000000000114 ) ;
#23414 = DIRECTION ( 'NONE',  ( -1.000000000000000000, 0.000000000000000000, 9.251858538542979716E-16 ) ) ;
#23415 = CARTESIAN_POINT ( 'NONE',  ( -168.4459734468149463, 0.000000000000000000, 159.0682875569279702 ) ) ;
#23416 = AXIS2_PLACEMENT_3D ( 'NONE', #26297, #18576, #2437 ) ;
#23417 = EDGE_LOOP ( 'NONE', ( #50131, #2596, #43230, #3462 ) ) ;
#23418 = CARTESIAN_POINT ( 'NONE',  ( 80.00000000000092371, 17.00000000000000000, 0.000000000000000000 ) ) ;
#23419 = EDGE_CURVE ( 'NONE', #30554, #14213, #37737, .T. ) ;
#23420 = CARTESIAN_POINT ( 'NONE',  ( 30.00000000000153833, 17.00000000000000000, 60.00000000000000000 ) ) ;
#23421 = ORIENTED_EDGE ( 'NONE', *, *, #40875, .T. ) ;
#23422 = DIRECTION ( 'NONE',  ( 1.000000000000000000, 0.000000000000000000, 0.000000000000000000 ) ) ;
#23423 = DIRECTION ( 'NONE',  ( 4.758098676964956461E-16, 1.000000000000000000, 0.000000000000000000 ) ) ;
#23424 =( BOUNDED_CURVE ( )  B_SPLINE_CURVE ( 3, ( #47551, #38643, #3458, #11680 ),
 .UNSPECIFIED., .F., .F. ) 
 B_SPLINE_CURVE_WITH_KNOTS ( ( 4, 4 ),
 ( 3.141592653589793116, 4.712388980384689674 ),
 .UNSPECIFIED. ) 
 CURVE ( )  GEOMETRIC_REPRESENTATION_ITEM ( )  RATIONAL_B_SPLINE_CURVE ( ( 1.000000000000000000, 0.8047378541243649375, 0.8047378541243649375, 1.000000000000000000 ) ) 
 REPRESENTATION_ITEM ( '' )  );
#23425 = CARTESIAN_POINT ( 'NONE',  ( -207.7210997126620384, -1.750000000000009548, -0.2068387089191121020 ) ) ;
#23426 = UNCERTAINTY_MEASURE_WITH_UNIT (LENGTH_MEASURE( 1.000000000000000082E-05 ), #10973, 'distance_accuracy_value', 'NONE');
#23427 = CARTESIAN_POINT ( 'NONE',  ( -7.822422304254325276, -2.816136035261162185, 230.0000000000000000 ) ) ;
#23428 = ORIENTED_EDGE ( 'NONE', *, *, #42917, .F. ) ;
#23429 = VERTEX_POINT ( 'NONE', #1853 ) ;
#23430 = DIRECTION ( 'NONE',  ( -0.000000000000000000, -6.123233995736766036E-17, 1.000000000000000000 ) ) ;
#23431 = ORIENTED_EDGE ( 'NONE', *, *, #17092, .F. ) ;
#23432 = CARTESIAN_POINT ( 'NONE',  ( 191.5540265531851105, 0.000000000000000000, -77.43171244307204404 ) ) ;
#23433 = CARTESIAN_POINT ( 'NONE',  ( 154.1026953830863420, -97.66198943095992036, -17.48025818148969890 ) ) ;
#23434 = DIRECTION ( 'NONE',  ( -4.758098676964956461E-16, 0.000000000000000000, -1.000000000000000000 ) ) ;
#23435 = VECTOR ( 'NONE', #2961, 1000.000000000000000 ) ;
#23436 = ORIENTED_EDGE ( 'NONE', *, *, #43808, .F. ) ;
#23437 = PLANE ( 'NONE',  #38300 ) ;
#23438 = ORIENTED_EDGE ( 'NONE', *, *, #34657, .T. ) ;
#23439 = ADVANCED_FACE ( 'NONE', ( #13139 ), #25705, .T. ) ;
#23440 = AXIS2_PLACEMENT_3D ( 'NONE', #33258, #12960, #49091 ) ;
#23441 = CARTESIAN_POINT ( 'NONE',  ( -165.0000000000000284, 17.00000000000000000, -114.9999999999999858 ) ) ;
#23442 = DIRECTION ( 'NONE',  ( -0.000000000000000000, -0.000000000000000000, -1.000000000000000000 ) ) ;
#23444 = AXIS2_PLACEMENT_3D ( 'NONE', #31522, #15356, #18674 ) ;
#23443 = LINE ( 'NONE', #46736, #38658 ) ;
#23445 = ORIENTED_EDGE ( 'NONE', *, *, #48086, .T. ) ;
#23446 = ORIENTED_EDGE ( 'NONE', *, *, #41822, .T. ) ;
#23447 = VERTEX_POINT ( 'NONE', #44908 ) ;
#23448 = DIRECTION ( 'NONE',  ( 0.000000000000000000, 1.000000000000000000, -1.822804496942679766E-16 ) ) ;
#23449 = CARTESIAN_POINT ( 'NONE',  ( -46.69597344681494633, 1.750000000000010214, 40.81828755692798438 ) ) ;
#23450 = CARTESIAN_POINT ( 'NONE',  ( 2.637606039711250183, 0.1407378881970818563, 9.847478953136986846 ) ) ;
#23451 = ORIENTED_EDGE ( 'NONE', *, *, #37886, .F. ) ;
#23452 = CARTESIAN_POINT ( 'NONE',  ( -1.057156451998854996, 0.7920882637787067804, 9.943883492372851407 ) ) ;
#23453 = ORIENTED_EDGE ( 'NONE', *, *, #18181, .T. ) ;
#23454 = CARTESIAN_POINT ( 'NONE',  ( -8.445973446814962315, 1.025126265847096985, -160.9317124430720014 ) ) ;
#23455 = VERTEX_POINT ( 'NONE', #5188 ) ;
#23456 = CARTESIAN_POINT ( 'NONE',  ( -64.99999999999783995, 17.00000000000000000, 115.0000000000000142 ) ) ;
#23457 = CARTESIAN_POINT ( 'NONE',  ( -34.08355720199904226, 2.371364769369340042, 7.455576670931136185 ) ) ;
#23458 = DIRECTION ( 'NONE',  ( 0.4740998230350172427, 0.3386427307392981256, -0.8127425537743157014 ) ) ;
#23459 = EDGE_CURVE ( 'NONE', #37912, #16652, #8727, .T. ) ;
#23460 = ADVANCED_FACE ( 'NONE', ( #17753 ), #44420, .T. ) ;
#23461 = CARTESIAN_POINT ( 'NONE',  ( 4.763548243873389154, -16.57409059453848599, 8.727788335465566760 ) ) ;
#23462 = EDGE_LOOP ( 'NONE', ( #50514, #6762, #29120 ) ) ;
#23463 = ORIENTED_EDGE ( 'NONE', *, *, #3581, .T. ) ;
#23464 = CARTESIAN_POINT ( 'NONE',  ( 0.000000000000000000, 0.000000000000000000, 900.0000000000000000 ) ) ;
#23465 = EDGE_CURVE ( 'NONE', #891, #47169, #48248, .T. ) ;
#23466 = ADVANCED_FACE ( 'NONE', ( #24954, #40603 ), #2344, .T. ) ;
#23467 = CARTESIAN_POINT ( 'NONE',  ( -166.6959734468149463, -1.750000000000009992, 160.8182875569279702 ) ) ;
#23468 = DIRECTION ( 'NONE',  ( -1.000000000000000000, 0.000000000000000000, 0.000000000000000000 ) ) ;
#23469 = EDGE_CURVE ( 'NONE', #6842, #11488, #44572, .T. ) ;
#23470 = EDGE_CURVE ( 'NONE', #36660, #21982, #17249, .T. ) ;
#23471 = AXIS2_PLACEMENT_3D ( 'NONE', #2886, #15228, #19561 ) ;
#23472 = CARTESIAN_POINT ( 'NONE',  ( -126.6959734468149321, 1.749999999999997335, -79.18171244307201562 ) ) ;
#23473 = AXIS2_PLACEMENT_3D ( 'NONE', #36966, #21526, #5372 ) ;
#23474 = AXIS2_PLACEMENT_3D ( 'NONE', #11892, #23939, #8553 ) ;
#23475 = CARTESIAN_POINT ( 'NONE',  ( 36.01122090644292228, 10.59066248886193407, -2.490396854064191867 ) ) ;
#23476 = ORIENTED_EDGE ( 'NONE', *, *, #11162, .F. ) ;
#23477 = CYLINDRICAL_SURFACE ( 'NONE', #6530, 3.750000000000000000 ) ;
#23478 = EDGE_CURVE ( 'NONE', #16604, #6362, #25451, .T. ) ;
#23479 = LINE ( 'NONE', #3445, #19761 ) ;
#23480 = ORIENTED_EDGE ( 'NONE', *, *, #32954, .T. ) ;
#23481 =( BOUNDED_CURVE ( )  B_SPLINE_CURVE ( 3, ( #35047, #4230, #50615, #47026 ),
 .UNSPECIFIED., .F., .F. ) 
 B_SPLINE_CURVE_WITH_KNOTS ( ( 4, 4 ),
 ( 1.570796326794896558, 3.141592653589793116 ),
 .UNSPECIFIED. ) 
 CURVE ( )  GEOMETRIC_REPRESENTATION_ITEM ( )  RATIONAL_B_SPLINE_CURVE ( ( 1.000000000000000000, 0.8047378541243649375, 0.8047378541243649375, 1.000000000000000000 ) ) 
 REPRESENTATION_ITEM ( '' )  );
#23482 = AXIS2_PLACEMENT_3D ( 'NONE', #5436, #36771, #1604 ) ;
#23483 = FACE_OUTER_BOUND ( 'NONE', #45189, .T. ) ;
#23484 = PRESENTATION_LAYER_ASSIGNMENT (  '', '', ( #6273 ) ) ;
#23485 = CARTESIAN_POINT ( 'NONE',  ( -6.695973446814940111, 1.750000000000023759, -39.18171244307202983 ) ) ;
#23486 =( BOUNDED_CURVE ( )  B_SPLINE_CURVE ( 3, ( #5088, #47908, #28954, #9452 ),
 .UNSPECIFIED., .F., .F. ) 
 B_SPLINE_CURVE_WITH_KNOTS ( ( 4, 4 ),
 ( 3.141592653589793116, 4.712388980384689674 ),
 .UNSPECIFIED. ) 
 CURVE ( )  GEOMETRIC_REPRESENTATION_ITEM ( )  RATIONAL_B_SPLINE_CURVE ( ( 1.000000000000000000, 0.8047378541243649375, 0.8047378541243649375, 1.000000000000000000 ) ) 
 REPRESENTATION_ITEM ( '' )  );
#23487 = ORIENTED_EDGE ( 'NONE', *, *, #35999, .T. ) ;
#23488 = ORIENTED_EDGE ( 'NONE', *, *, #1241, .T. ) ;
#23489 = LINE ( 'NONE', #19372, #34079 ) ;
#23490 = CIRCLE ( 'NONE', #25102, 3.749999999999975575 ) ;
#23491 = LINE ( 'NONE', #39147, #47587 ) ;
#23492 = VERTEX_POINT ( 'NONE', #37284 ) ;
#23493 = VERTEX_POINT ( 'NONE', #48992 ) ;
#23494 = CARTESIAN_POINT ( 'NONE',  ( 195.0540265531851105, 2.143131898507880377E-16, -157.4317124430720582 ) ) ;
#23495 = CARTESIAN_POINT ( 'NONE',  ( -0.4166666666666664631, 0.000000000000000000, 10.00000000000000000 ) ) ;
#23496 = CARTESIAN_POINT ( 'NONE',  ( -8.277096487746778308, 50.00000000000000711, 7.455576670931136185 ) ) ;
#23497 = CARTESIAN_POINT ( 'NONE',  ( 153.3040265531850537, 1.750000000000009992, 160.8182875569279702 ) ) ;
#23498 = VERTEX_POINT ( 'NONE', #33659 ) ;
#23499 = VERTEX_POINT ( 'NONE', #50254 ) ;
#23500 = VERTEX_POINT ( 'NONE', #7215 ) ;
#23501 = EDGE_CURVE ( 'NONE', #12400, #18141, #23109, .T. ) ;
#23502 = LINE ( 'NONE', #26333, #34910 ) ;
#23503 = CARTESIAN_POINT ( 'NONE',  ( -168.4459734468149463, 0.000000000000000000, 39.06828755692798438 ) ) ;
#23504 = EDGE_LOOP ( 'NONE', ( #25677, #48053, #45991, #18913 ) ) ;
#23505 = CARTESIAN_POINT ( 'NONE',  ( -239.0000000000000853, -165.6999999999999602, 250.3600000000000136 ) ) ;
#23506 = AXIS2_PLACEMENT_3D ( 'NONE', #21715, #17367, #9917 ) ;
#23507 = DIRECTION ( 'NONE',  ( -3.172065784643302499E-16, -1.000000000000000000, 2.537652627714642000E-15 ) ) ;
#23508 = DIRECTION ( 'NONE',  ( -0.000000000000000000, -0.000000000000000000, -1.000000000000000000 ) ) ;
#23509 = ORIENTED_EDGE ( 'NONE', *, *, #18884, .T. ) ;
#23510 = ORIENTED_EDGE ( 'NONE', *, *, #6186, .T. ) ;
#23511 = DIRECTION ( 'NONE',  ( -1.000000000000000000, -0.000000000000000000, -0.000000000000000000 ) ) ;
#23512 = CARTESIAN_POINT ( 'NONE',  ( 166.9999999999999716, -184.9999999999999716, -344.0000000000001137 ) ) ;
#23513 = CARTESIAN_POINT ( 'NONE',  ( 4.353119224256710496, 9.002796955358187247, 0.000000000000000000 ) ) ;
#23514 = UNCERTAINTY_MEASURE_WITH_UNIT (LENGTH_MEASURE( 1.000000000000000082E-05 ), #13364, 'distance_accuracy_value', 'NONE');
#23515 = EDGE_LOOP ( 'NONE', ( #6461, #13676, #21297, #5377, #31649, #20399, #2096, #19681, #37638, #32824, #32966, #39535, #7493, #44987, #21254, #33719, #8148, #49214, #43879, #5442, #25381, #2374, #21195, #18767, #35034, #31831, #50380, #48940, #37143, #8261, #47978, #9457 ) ) ;
#23516 = ORIENTED_EDGE ( 'NONE', *, *, #25535, .T. ) ;
#23517 = FACE_OUTER_BOUND ( 'NONE', #33735, .T. ) ;
#23518 = ORIENTED_EDGE ( 'NONE', *, *, #16501, .F. ) ;
#23519 = CYLINDRICAL_SURFACE ( 'NONE', #46086, 1.750000000000036193 ) ;
#23520 = CARTESIAN_POINT ( 'NONE',  ( 84.99999999999997158, 17.00000000000000000, -114.9999999999999858 ) ) ;
#23521 = CARTESIAN_POINT ( 'NONE',  ( -14.99999999999812594, 17.00000000000000000, 65.00000000000000000 ) ) ;
#23522 = EDGE_CURVE ( 'NONE', #6202, #35055, #22281, .T. ) ;
#23523 = VERTEX_POINT ( 'NONE', #30826 ) ;
#23524 = CARTESIAN_POINT ( 'NONE',  ( 1.377509002708426689, -0.6027468487254984408, 9.927319414211227766 ) ) ;
#23525 = B_SPLINE_CURVE_WITH_KNOTS ( 'NONE', 3,
 ( #36807, #13427, #48031, #28329 ),
 .UNSPECIFIED., .F., .F.,
 ( 4, 4 ),
 ( 0.0009679537044784459771, 0.001281751046851268335 ),
 .UNSPECIFIED. ) ;
#23526 = LINE ( 'NONE', #39186, #3535 ) ;
#23527 = CARTESIAN_POINT ( 'NONE',  ( 30.00000000000062172, 17.00000000000000000, -54.99999999999999289 ) ) ;
#23528 = AXIS2_PLACEMENT_3D ( 'NONE', #15599, #34863, #4050 ) ;
#23529 = EDGE_CURVE ( 'NONE', #43783, #21151, #39690, .T. ) ;
#23530 = CARTESIAN_POINT ( 'NONE',  ( -0.3862712429686977478, 1.188820645368937390, -10.00000000000000000 ) ) ;
#23531 = ADVANCED_FACE ( 'NONE', ( #41602 ), #26960, .T. ) ;
#23532 = VERTEX_POINT ( 'NONE', #11315 ) ;
#23533 = EDGE_CURVE ( 'NONE', #4976, #692, #37776, .T. ) ;
#23534 = DIRECTION ( 'NONE',  ( -1.000000000000000000, 0.000000000000000000, 0.000000000000000000 ) ) ;
#23535 = CYLINDRICAL_SURFACE ( 'NONE', #17635, 1.750000000000001554 ) ;
#23536 = LINE ( 'NONE', #39446, #42674 ) ;
#23537 = ORIENTED_EDGE ( 'NONE', *, *, #12430, .T. ) ;
#23538 = DIRECTION ( 'NONE',  ( 0.000000000000000000, 0.000000000000000000, -1.000000000000000000 ) ) ;
#23539 = AXIS2_PLACEMENT_3D ( 'NONE', #19457, #35144, #50721 ) ;
#23540 = FACE_OUTER_BOUND ( 'NONE', #28842, .T. ) ;
#23541 = ORIENTED_EDGE ( 'NONE', *, *, #24513, .T. ) ;
#23542 = DIRECTION ( 'NONE',  ( 0.000000000000000000, 0.000000000000000000, -1.000000000000000000 ) ) ;
#23543 = CARTESIAN_POINT ( 'NONE',  ( 10.50000000000000178, -46.01315789473684248, -25.00000000000000000 ) ) ;
#23544 = CARTESIAN_POINT ( 'NONE',  ( -88.44597344681494633, 1.025126265847089435, -40.93171244307204404 ) ) ;
#23545 = VERTEX_POINT ( 'NONE', #29803 ) ;
#23546 = CARTESIAN_POINT ( 'NONE',  ( -125.6708471809678542, -1.749999999999996669, -38.15658617722495194 ) ) ;
#23547 = ORIENTED_EDGE ( 'NONE', *, *, #40394, .T. ) ;
#23548 = EDGE_LOOP ( 'NONE', ( #18682, #46107, #3310, #29205, #30464, #41742 ) ) ;
#23549 = CARTESIAN_POINT ( 'NONE',  ( 30.77287599203632951, 12.70002479445995824, 3.199614146704519602 ) ) ;
#23550 = CARTESIAN_POINT ( 'NONE',  ( -0.3139796262078424216, 1.230474926876623076, 9.975314328424618182 ) ) ;
#23551 = ORIENTED_EDGE ( 'NONE', *, *, #3949, .F. ) ;
#23552 = CARTESIAN_POINT ( 'NONE',  ( -7.372990760266265653, 0.000000000000000000, 0.000000000000000000 ) ) ;
#23553 = DIRECTION ( 'NONE',  ( 0.000000000000000000, 0.000000000000000000, -1.000000000000000000 ) ) ;
#23554 = DIRECTION ( 'NONE',  ( -1.586032892321652236E-16, -1.000000000000000000, -6.853681917100419162E-49 ) ) ;
#23555 = ORIENTED_EDGE ( 'NONE', *, *, #13688, .T. ) ;
#23556 = EDGE_CURVE ( 'NONE', #13632, #14882, #34681, .T. ) ;
#23557 = CARTESIAN_POINT ( 'NONE',  ( 169.0000000000000000, 2.775557561562891351E-14, -111.0000000000001563 ) ) ;
#23558 = PLANE ( 'NONE',  #27507 ) ;
#23559 = LINE ( 'NONE', #19704, #16043 ) ;
#23560 = EDGE_LOOP ( 'NONE', ( #31011, #4857, #15908, #20327 ) ) ;
#23561 = CARTESIAN_POINT ( 'NONE',  ( 13.59579750444771307, -10.60877755095900632, 8.727788335465566760 ) ) ;
#23562 = CARTESIAN_POINT ( 'NONE',  ( 339.9999999999999432, -168.9999999999999432, -356.0000000000002274 ) ) ;
#23563 = EDGE_LOOP ( 'NONE', ( #32952, #10301, #32470, #40200 ) ) ;
#23564 = ORIENTED_EDGE ( 'NONE', *, *, #1607, .T. ) ;
#23565 = ORIENTED_EDGE ( 'NONE', *, *, #17858, .F. ) ;
#23566 = FACE_OUTER_BOUND ( 'NONE', #12209, .T. ) ;
#23567 = CARTESIAN_POINT ( 'NONE',  ( 167.0000000000000000, -168.9999999999993747, -115.0000000000001847 ) ) ;
#23568 = ORIENTED_EDGE ( 'NONE', *, *, #44095, .T. ) ;
#23569 = CARTESIAN_POINT ( 'NONE',  ( -124.9459734468149463, 2.143131898507847836E-16, 2.568287556927950632 ) ) ;
#23570 = CARTESIAN_POINT ( 'NONE',  ( 195.0540265531851105, 2.143131898507880377E-16, -80.93171244307201562 ) ) ;
#23571 = CARTESIAN_POINT ( 'NONE',  ( -48.44597344681495343, 0.000000000000000000, 159.0682875569279702 ) ) ;
#23572 = CARTESIAN_POINT ( 'NONE',  ( -6.875132362119187768, 50.00000000000000711, 8.356839323120299312 ) ) ;
#23573 = DIRECTION ( 'NONE',  ( -1.000000000000000000, -0.000000000000000000, -0.000000000000000000 ) ) ;
#23574 = AXIS2_PLACEMENT_3D ( 'NONE', #41994, #41490, #49141 ) ;
#23575 = DIRECTION ( 'NONE',  ( -0.000000000000000000, -1.000000000000000000, -0.000000000000000000 ) ) ;
#23576 = CARTESIAN_POINT ( 'NONE',  ( 181.0000000000000000, -184.9999999999999716, -344.0000000000001137 ) ) ;
#23577 = DIRECTION ( 'NONE',  ( 0.000000000000000000, -0.000000000000000000, 1.000000000000000000 ) ) ;
#23578 = CARTESIAN_POINT ( 'NONE',  ( 33.38053581724552288, 17.16548397897151546, 4.835783797351798974 ) ) ;
#23579 = FACE_OUTER_BOUND ( 'NONE', #21354, .T. ) ;
#23580 = CARTESIAN_POINT ( 'NONE',  ( 35.00000000000216716, 17.00000000000000000, 95.00000000000000000 ) ) ;
#23581 = LINE ( 'NONE', #43827, #45342 ) ;
#23582 = DIRECTION ( 'NONE',  ( 0.000000000000000000, 0.000000000000000000, -1.000000000000000000 ) ) ;
#23583 = ORIENTED_EDGE ( 'NONE', *, *, #40232, .T. ) ;
#23584 = EDGE_CURVE ( 'NONE', #15590, #541, #2588, .T. ) ;
#23585 = CARTESIAN_POINT ( 'NONE',  ( 181.0000000000000568, 175.0000000000000284, 343.9999999999998863 ) ) ;
#23586 = VECTOR ( 'NONE', #11651, 1000.000000000000000 ) ;
#23587 = CARTESIAN_POINT ( 'NONE',  ( 5.551115123125782702E-14, -168.9999999999999432, 343.9999999999997726 ) ) ;
#23588 = LINE ( 'NONE', #27191, #22539 ) ;
#23589 = CARTESIAN_POINT ( 'NONE',  ( 30.12518629743562926, 14.70074613238908157, 1.847720168420772691 ) ) ;
#23590 = EDGE_LOOP ( 'NONE', ( #15290, #19261, #43024, #27340, #9279, #41609 ) ) ;
#23591 = DIRECTION ( 'NONE',  ( 0.000000000000000000, 0.000000000000000000, 1.000000000000000000 ) ) ;
#23592 = ORIENTED_EDGE ( 'NONE', *, *, #25591, .T. ) ;
#23593 = CARTESIAN_POINT ( 'NONE',  ( 33.86622497129647513, -3.037805405904928868, 7.906207997025717304 ) ) ;
#23594 = ORIENTED_EDGE ( 'NONE', *, *, #43218, .F. ) ;
#23595 = LINE ( 'NONE', #7452, #29527 ) ;
#23596 = DIRECTION ( 'NONE',  ( 0.000000000000000000, 0.000000000000000000, -1.000000000000000000 ) ) ;
#23597 = EDGE_LOOP ( 'NONE', ( #49938, #11811, #5852 ) ) ;
#23598 = LINE ( 'NONE', #16163, #3583 ) ;
#23599 = VERTEX_POINT ( 'NONE', #3606 ) ;
#23600 = VECTOR ( 'NONE', #37544, 1000.000000000000000 ) ;
#23601 = ORIENTED_EDGE ( 'NONE', *, *, #5993, .T. ) ;
#23602 = LINE ( 'NONE', #19754, #49073 ) ;
#23603 = CARTESIAN_POINT ( 'NONE',  ( 341.6568542494922553, -165.0000000000001137, -340.0000000000002842 ) ) ;
#23604 = VERTEX_POINT ( 'NONE', #41852 ) ;
#23605 = CARTESIAN_POINT ( 'NONE',  ( -26.18032376592659105, 21.95228666728381128, 7.455576670931136185 ) ) ;
#23606 = CARTESIAN_POINT ( 'NONE',  ( -1.365263087672800246, 0.5437404457009007430, 9.958264684458713489 ) ) ;
#23607 = LINE ( 'NONE', #23357, #13433 ) ;
#23608 = ORIENTED_EDGE ( 'NONE', *, *, #5264, .T. ) ;
#23609 = EDGE_CURVE ( 'NONE', #35393, #18024, #20338, .T. ) ;
#23610 = DIRECTION ( 'NONE',  ( 0.000000000000000000, -0.000000000000000000, -1.000000000000000000 ) ) ;
#23611 = CARTESIAN_POINT ( 'NONE',  ( 2.499999999999945377, -224.9999999999999716, -240.0000000000000000 ) ) ;
#23612 =( BOUNDED_CURVE ( )  B_SPLINE_CURVE ( 3, ( #33180, #48507, #11267, #42798 ),
 .UNSPECIFIED., .F., .F. ) 
 B_SPLINE_CURVE_WITH_KNOTS ( ( 4, 4 ),
 ( 4.712388980384689674, 6.283185307179586232 ),
 .UNSPECIFIED. ) 
 CURVE ( )  GEOMETRIC_REPRESENTATION_ITEM ( )  RATIONAL_B_SPLINE_CURVE ( ( 1.000000000000000000, 0.8047378541243649375, 0.8047378541243649375, 1.000000000000000000 ) ) 
 REPRESENTATION_ITEM ( '' )  );
#23613 = EDGE_CURVE ( 'NONE', #40073, #31274, #33915, .T. ) ;
#23614 = EDGE_LOOP ( 'NONE', ( #8600, #43023, #28460, #39509, #25211, #6012 ) ) ;
#23615 = CARTESIAN_POINT ( 'NONE',  ( -2.945500763482279627, -16.64098165802040086, -9.008049429158100807 ) ) ;
#23616 = DIRECTION ( 'NONE',  ( -1.000000000000000000, 0.000000000000000000, 0.000000000000000000 ) ) ;
#23617 = EDGE_LOOP ( 'NONE', ( #7957, #12139, #14274, #8538 ) ) ;
#23618 = LINE ( 'NONE', #32, #36899 ) ;
#23619 =( BOUNDED_CURVE ( )  B_SPLINE_CURVE ( 3, ( #28882, #16579, #12720, #25536 ),
 .UNSPECIFIED., .F., .F. ) 
 B_SPLINE_CURVE_WITH_KNOTS ( ( 4, 4 ),
 ( 3.141592653589793116, 4.712388980384689674 ),
 .UNSPECIFIED. ) 
 CURVE ( )  GEOMETRIC_REPRESENTATION_ITEM ( )  RATIONAL_B_SPLINE_CURVE ( ( 1.000000000000000000, 0.8047378541243649375, 0.8047378541243649375, 1.000000000000000000 ) ) 
 REPRESENTATION_ITEM ( '' )  );
#23620 = B_SPLINE_CURVE_WITH_KNOTS ( 'NONE', 3,
 ( #32535, #8165, #20711, #9160 ),
 .UNSPECIFIED., .F., .F.,
 ( 4, 4 ),
 ( 0.000000000000000000, 0.2562577668812812681 ),
 .UNSPECIFIED. ) ;
#23621 = LINE ( 'NONE', #32345, #35813 ) ;
#23622 = B_SPLINE_SURFACE_WITH_KNOTS ( 'NONE', 3, 3, ( 
 ( #39079, #7509, #46456, #15964 ),
 ( #24178, #4670, #35478, #12118 ),
 ( #39835, #11347, #15448, #23909 ),
 ( #12352, #67, #23658, #27763 ) ),
 .UNSPECIFIED., .F., .F., .F.,
 ( 4, 4 ),
 ( 4, 4 ),
 ( 0.000000000000000000, 1.000000000000000000 ),
 ( 0.000000000000000000, 1.000000000000000000 ),
 .UNSPECIFIED. ) ;
#23623 = ORIENTED_EDGE ( 'NONE', *, *, #10586, .F. ) ;
#23624 = CARTESIAN_POINT ( 'NONE',  ( -204.9459734468149463, 2.143131898507880377E-16, -37.43171244307205825 ) ) ;
#23625 = DIRECTION ( 'NONE',  ( 0.000000000000000000, -1.000000000000000000, 0.000000000000000000 ) ) ;
#23626 = DIRECTION ( 'NONE',  ( 0.000000000000000000, -1.000000000000000000, 0.000000000000000000 ) ) ;
#23627 = LINE ( 'NONE', #7734, #50087 ) ;
#23628 = ORIENTED_EDGE ( 'NONE', *, *, #30409, .F. ) ;
#23629 = CARTESIAN_POINT ( 'NONE',  ( -5.888214538810513154, -16.20866436362413410, 8.727788335465566760 ) ) ;
#23630 = PLANE ( 'NONE',  #11982 ) ;
#23631 =( BOUNDED_CURVE ( )  B_SPLINE_CURVE ( 3, ( #37478, #17932, #36465, #28751 ),
 .UNSPECIFIED., .F., .F. ) 
 B_SPLINE_CURVE_WITH_KNOTS ( ( 4, 4 ),
 ( 4.712388980384689674, 6.283185307179586232 ),
 .UNSPECIFIED. ) 
 CURVE ( )  GEOMETRIC_REPRESENTATION_ITEM ( )  RATIONAL_B_SPLINE_CURVE ( ( 1.000000000000000000, 0.8047378541243649375, 0.8047378541243649375, 1.000000000000000000 ) ) 
 REPRESENTATION_ITEM ( '' )  );
#23632 = CARTESIAN_POINT ( 'NONE',  ( -0.1287570809895658697, 0.3962735484563123523, 10.00000000000000000 ) ) ;
#23633 = VERTEX_POINT ( 'NONE', #30068 ) ;
#23634 = EDGE_CURVE ( 'NONE', #8918, #4845, #45673, .T. ) ;
#23635 = ORIENTED_EDGE ( 'NONE', *, *, #27935, .T. ) ;
#23636 = APPLICATION_PROTOCOL_DEFINITION ( 'draft international standard', 'automotive_design', 1998, #21692 ) ;
#23637 = LINE ( 'NONE', #23384, #4835 ) ;
#23638 = CARTESIAN_POINT ( 'NONE',  ( -124.9459734468149463, 2.143131898507847836E-16, -40.93171244307202983 ) ) ;
#23639 = ADVANCED_FACE ( 'NONE', ( #6959 ), #38024, .T. ) ;
#23640 = AXIS2_PLACEMENT_3D ( 'NONE', #32676, #48273, #28824 ) ;
#23641 = EDGE_CURVE ( 'NONE', #41219, #25957, #32790, .T. ) ;
#23642 = CARTESIAN_POINT ( 'NONE',  ( -204.9459734468149463, 2.143131898507880377E-16, -40.93171244307202983 ) ) ;
#23643 = CARTESIAN_POINT ( 'NONE',  ( -69.99999999999783995, 17.00000000000000000, 95.00000000000000000 ) ) ;
#23644 = CARTESIAN_POINT ( 'NONE',  ( 210.0000000000000568, 0.000000000000000000, 2.568287556927987048 ) ) ;
#23645 = ORIENTED_EDGE ( 'NONE', *, *, #9852, .T. ) ;
#23646 = CARTESIAN_POINT ( 'NONE',  ( -48.44597344681496054, 1.025126265847089435, -77.43171244307200141 ) ) ;
#23647 = EDGE_CURVE ( 'NONE', #11684, #26946, #22607, .T. ) ;
#23648 = FACE_OUTER_BOUND ( 'NONE', #20942, .T. ) ;
#23649 = CLOSED_SHELL ( 'NONE', ( #38454, #41241, #30012, #41543, #32714, #3350, #18528, #40434, #14742, #19911, #34627, #36375, #41185, #6078, #36535, #20616, #37023, #13381, #25912, #50553, #38187, #1991, #40601, #49123, #31798, #47859, #44952, #48704, #21155, #37144, #36253, #30126, #9841, #27793, #15870, #43499, #44323, #41576, #7985, #7833, #4898, #34125, #45278, #9805, #30882, #45224, #33039, #47747, #19436, #14701, #40900, #36205, #48776, #19546, #13971, #20048, #20904, #15829, #19023, #50690, #46212, #14994, #22664, #8619, #1087, #40790, #44916, #2599, #33429, #50564, #13711, #20709, #34920, #19571, #50093, #28041, #16439, #5131, #4572, #10858, #21687, #46534, #8756, #26732, #18388, #5539, #42285, #37524, #10651, #25491, #14645, #14004, #43671, #40503, #2136, #8123, #46220, #36572, #39826, #45026, #1889, #17716, #43291, #34654, #11581, #33346, #138, #42824, #25518, #32287, #38051, #13623, #29002, #10201, #14891, #21179, #13426, #32803, #29361, #18042, #48064, #39175, #23087, #32578, #24780, #29629, #29702, #4972, #49184, #13894, #22171, #7172, #25532, #21948, #49262, #28913, #27147, #21570, #32699, #8446, #15943, #41277, #108, #14938, #45843, #43032, #14150, #13252, #8994, #9610, #6083, #6693, #24637, #21754, #2289, #30842, #45000, #31344, #35071, #2034, #16031, #28226, #14941, #12441, #37446, #42162, #30869, #15936, #23174, #2797, #12941, #34957, #44115, #39295, #33355, #47074, #23971, #4304 ) ) ;
#23650 = B_SPLINE_CURVE_WITH_KNOTS ( 'NONE', 3,
 ( #7678, #7430, #15879, #39495 ),
 .UNSPECIFIED., .F., .F.,
 ( 4, 4 ),
 ( 0.001152428489661413242, 0.001623376834729681802 ),
 .UNSPECIFIED. ) ;
#23651 = ADVANCED_FACE ( 'NONE', ( #22852 ), #18738, .T. ) ;
#23652 = DIRECTION ( 'NONE',  ( 2.958228394578793832E-31, 0.000000000000000000, 1.000000000000000000 ) ) ;
#23653 = VERTEX_POINT ( 'NONE', #288 ) ;
#23654 = CARTESIAN_POINT ( 'NONE',  ( 343.9999999999999432, -174.9999999999999432, 359.9999999999998295 ) ) ;
#23655 = ORIENTED_EDGE ( 'NONE', *, *, #36978, .T. ) ;
#23656 = APPLICATION_CONTEXT ( 'automotive_design' ) ;
#23657 = ORIENTED_EDGE ( 'NONE', *, *, #20837, .F. ) ;
#23658 = CARTESIAN_POINT ( 'NONE',  ( -5.888214538810513154, -16.20866436362413410, 8.727788335465566760 ) ) ;
#23659 = DIRECTION ( 'NONE',  ( 0.000000000000000000, -1.000000000000000000, -3.186989995019654210E-49 ) ) ;
#23660 =( NAMED_UNIT ( * ) SI_UNIT ( $, .STERADIAN. ) SOLID_ANGLE_UNIT ( ) );
#23661 = ORIENTED_EDGE ( 'NONE', *, *, #42760, .T. ) ;
#23662 = CARTESIAN_POINT ( 'NONE',  ( 181.0000000000000000, -272.4999999999999432, -339.9999999999998863 ) ) ;
#23663 = DIRECTION ( 'NONE',  ( 0.000000000000000000, 0.000000000000000000, 1.000000000000000000 ) ) ;
#23664 = ORIENTED_EDGE ( 'NONE', *, *, #25841, .T. ) ;
#23665 = CARTESIAN_POINT ( 'NONE',  ( 164.9999999999999716, 17.00000000000000000, -25.00000000000000711 ) ) ;
#23666 = CARTESIAN_POINT ( 'NONE',  ( 169.0000000000000000, -174.9999999999999716, -111.0000000000001563 ) ) ;
#23667 = CARTESIAN_POINT ( 'NONE',  ( -208.4459734468148611, -1.025126265847089213, -0.9317124430720324924 ) ) ;
#23668 = DIRECTION ( 'NONE',  ( 1.333906992743555050E-23, -1.000000000000000000, 0.000000000000000000 ) ) ;
#23669 = ORIENTED_EDGE ( 'NONE', *, *, #24063, .T. ) ;
#23671 = VERTEX_POINT ( 'NONE', #15419 ) ;
#23670 = EDGE_CURVE ( 'NONE', #13422, #47734, #31844, .T. ) ;
#23672 = CARTESIAN_POINT ( 'NONE',  ( 111.5540265531850679, 0.000000000000000000, 2.568287556927950632 ) ) ;
#23673 = EDGE_CURVE ( 'NONE', #13148, #13812, #6509, .T. ) ;
#23674 = AXIS2_PLACEMENT_3D ( 'NONE', #14992, #41681, #6294 ) ;
#23675 = EDGE_CURVE ( 'NONE', #49920, #11818, #20021, .T. ) ;
#23676 = ADVANCED_FACE ( 'NONE', ( #32087 ), #39794, .T. ) ;
#23677 = AXIS2_PLACEMENT_3D ( 'NONE', #15890, #35413, #23847 ) ;
#23678 = EDGE_LOOP ( 'NONE', ( #49408, #46704, #44083, #5595, #24029 ) ) ;
#23679 = DIRECTION ( 'NONE',  ( -1.000000000000000000, 0.000000000000000000, 0.000000000000000000 ) ) ;
#23680 = CARTESIAN_POINT ( 'NONE',  ( -208.4459734468149463, 0.000000000000000000, 119.0682875569279702 ) ) ;
#23681 = CARTESIAN_POINT ( 'NONE',  ( -119.9999999999997158, 16.00000000000000000, -60.00000000000000000 ) ) ;
#23682 = ORIENTED_EDGE ( 'NONE', *, *, #16153, .T. ) ;
#23684 = AXIS2_PLACEMENT_3D ( 'NONE', #10565, #45435, #3112 ) ;
#23683 = CARTESIAN_POINT ( 'NONE',  ( 35.05402655318504657, 2.143131898507880377E-16, -37.43171244307200141 ) ) ;
#23685 = CIRCLE ( 'NONE', #30230, 3.500000000000003109 ) ;
#23686 = ADVANCED_FACE ( 'NONE', ( #23879 ), #43120, .F. ) ;
#23687 = ORIENTED_EDGE ( 'NONE', *, *, #29644, .F. ) ;
#23688 = EDGE_CURVE ( 'NONE', #50585, #48233, #8745, .T. ) ;
#23689 = CARTESIAN_POINT ( 'NONE',  ( 30.00000000000092726, 16.00000000000000000, -24.99999999999999289 ) ) ;
#23690 = AXIS2_PLACEMENT_3D ( 'NONE', #37233, #48446, #44863 ) ;
#23691 = CARTESIAN_POINT ( 'NONE',  ( 135.0000000000019043, 16.00000000000000000, 65.00000000000000000 ) ) ;
#23692 = AXIS2_PLACEMENT_3D ( 'NONE', #37013, #14633, #1832 ) ;
#23693 = CARTESIAN_POINT ( 'NONE',  ( -1.249999999999999778, 0.000000000000000000, -3.333333333333333481 ) ) ;
#23694 = VERTEX_POINT ( 'NONE', #35708 ) ;
#23695 = ORIENTED_EDGE ( 'NONE', *, *, #33045, .T. ) ;
#23696 = ORIENTED_EDGE ( 'NONE', *, *, #4094, .F. ) ;
#23697 = CARTESIAN_POINT ( 'NONE',  ( -207.7210997126620384, 1.750000000000010436, 119.7931612910808781 ) ) ;
#23698 = LINE ( 'NONE', #16250, #31629 ) ;
#23699 = CARTESIAN_POINT ( 'NONE',  ( 183.0000000000000000, -81.49999999999997158, -350.0000000000001705 ) ) ;
#23700 = VERTEX_POINT ( 'NONE', #4378 ) ;
#23701 = CARTESIAN_POINT ( 'NONE',  ( 114.3291528190321173, 1.749999999999996225, 161.8434138227750907 ) ) ;
#23702 = ORIENTED_EDGE ( 'NONE', *, *, #31474, .F. ) ;
#23703 = EDGE_CURVE ( 'NONE', #14213, #31506, #11829, .T. ) ;
#23704 = CARTESIAN_POINT ( 'NONE',  ( -45.67084718096785423, -1.750000000000009548, 81.84341382277507648 ) ) ;
#23705 = ORIENTED_EDGE ( 'NONE', *, *, #5754, .F. ) ;
#23706 = CARTESIAN_POINT ( 'NONE',  ( 164.9999999999999716, 15.00000000000000000, 115.0000000000000142 ) ) ;
#23707 = CARTESIAN_POINT ( 'NONE',  ( 0.000000000000000000, 181.0000000000000284, -360.0000000000002274 ) ) ;
#23708 = CARTESIAN_POINT ( 'NONE',  ( 35.05402655318504657, 2.143131898507880377E-16, 165.0000000000000000 ) ) ;
#23709 = ADVANCED_FACE ( 'NONE', ( #546 ), #40044, .T. ) ;
#23710 = EDGE_CURVE ( 'NONE', #44854, #42571, #27589, .T. ) ;
#23711 = CARTESIAN_POINT ( 'NONE',  ( -0.6440276692615888310, -16.64212148744554298, -9.683996418299976483 ) ) ;
#23712 = CARTESIAN_POINT ( 'NONE',  ( 166.9999999999999716, -272.5000000000000000, -110.9999999999999005 ) ) ;
#23713 = ORIENTED_EDGE ( 'NONE', *, *, #43986, .F. ) ;
#23714 = ORIENTED_EDGE ( 'NONE', *, *, #3916, .T. ) ;
#23715 = PLANE ( 'NONE',  #5054 ) ;
#23716 = DIRECTION ( 'NONE',  ( -0.000000000000000000, -1.000000000000000000, -0.000000000000000000 ) ) ;
#23717 = CARTESIAN_POINT ( 'NONE',  ( 210.0000000000000568, 0.000000000000000000, 40.81828755692798438 ) ) ;
#23718 = VECTOR ( 'NONE', #20936, 1000.000000000000000 ) ;
#23719 = FACE_OUTER_BOUND ( 'NONE', #50582, .T. ) ;
#23720 =( BOUNDED_CURVE ( )  B_SPLINE_CURVE ( 3, ( #25685, #32890, #44149, #20810 ),
 .UNSPECIFIED., .F., .F. ) 
 B_SPLINE_CURVE_WITH_KNOTS ( ( 4, 4 ),
 ( 0.000000000000000000, 1.570796326794896558 ),
 .UNSPECIFIED. ) 
 CURVE ( )  GEOMETRIC_REPRESENTATION_ITEM ( )  RATIONAL_B_SPLINE_CURVE ( ( 1.000000000000000000, 0.8047378541243649375, 0.8047378541243649375, 1.000000000000000000 ) ) 
 REPRESENTATION_ITEM ( '' )  );
#23721 = DIRECTION ( 'NONE',  ( -0.000000000000000000, 1.000000000000000000, 0.000000000000000000 ) ) ;
#23722 = VERTEX_POINT ( 'NONE', #4130 ) ;
#23723 = EDGE_CURVE ( 'NONE', #19705, #28470, #21980, .T. ) ;
#23724 = CIRCLE ( 'NONE', #17945, 50.00000000000000000 ) ;
#23725 = CARTESIAN_POINT ( 'NONE',  ( 10.50000000000000178, -46.51315789473684248, 6.315789473684215061 ) ) ;
#23726 = LINE ( 'NONE', #27320, #17307 ) ;
#23727 = ORIENTED_EDGE ( 'NONE', *, *, #22678, .F. ) ;
#23728 = AXIS2_PLACEMENT_3D ( 'NONE', #28638, #40706, #21192 ) ;
#23729 = CARTESIAN_POINT ( 'NONE',  ( 1.249999999999999778, 0.000000000000000000, 3.333333333333333481 ) ) ;
#23730 = EDGE_CURVE ( 'NONE', #41145, #41350, #5440, .T. ) ;
#23731 = CARTESIAN_POINT ( 'NONE',  ( -128.4459734468149463, 1.025126265847081664, 42.56828755692797017 ) ) ;
#23732 = DIRECTION ( 'NONE',  ( -1.000000000000000000, -0.000000000000000000, -0.000000000000000000 ) ) ;
#23733 = VERTEX_POINT ( 'NONE', #35447 ) ;
#23734 = ORIENTED_EDGE ( 'NONE', *, *, #24654, .F. ) ;
#23735 = CARTESIAN_POINT ( 'NONE',  ( 0.000000000000000000, 17.00000000000000000, 0.000000000000000000 ) ) ;
#23736 = DIRECTION ( 'NONE',  ( 2.775557561562891351E-16, 0.7071067811865477948, 0.7071067811865473507 ) ) ;
#23737 = ADVANCED_FACE ( 'NONE', ( #11574 ), #8489, .F. ) ;
#23738 = EDGE_CURVE ( 'NONE', #11190, #37195, #20279, .T. ) ;
#23739 = ORIENTED_EDGE ( 'NONE', *, *, #28962, .T. ) ;
#23740 = ORIENTED_EDGE ( 'NONE', *, *, #28688, .F. ) ;
#23741 = DIRECTION ( 'NONE',  ( 0.000000000000000000, -1.000000000000000000, 8.021842663476564905E-17 ) ) ;
#23742 = CYLINDRICAL_SURFACE ( 'NONE', #2801, 1.750000000000001554 ) ;
#23743 = CARTESIAN_POINT ( 'NONE',  ( -204.9459734468149463, 2.143131898507880377E-16, 42.56828755692798438 ) ) ;
#23744 = DIRECTION ( 'NONE',  ( 0.000000000000000000, 2.537652627714643577E-15, 1.000000000000000000 ) ) ;
#23745 = VERTEX_POINT ( 'NONE', #19503 ) ;
#23746 = ORIENTED_EDGE ( 'NONE', *, *, #4628, .T. ) ;
#23747 = ORIENTED_EDGE ( 'NONE', *, *, #20839, .T. ) ;
#23748 = EDGE_CURVE ( 'NONE', #12164, #23225, #7984, .T. ) ;
#23749 = AXIS2_PLACEMENT_3D ( 'NONE', #40772, #5100, #24377 ) ;
#23750 = EDGE_CURVE ( 'NONE', #50718, #36234, #31337, .T. ) ;
#23751 = LINE ( 'NONE', #24509, #37374 ) ;
#23752 = VECTOR ( 'NONE', #1268, 1000.000000000000000 ) ;
#23753 = EDGE_CURVE ( 'NONE', #35737, #2212, #23621, .T. ) ;
#23754 = ORIENTED_EDGE ( 'NONE', *, *, #22390, .T. ) ;
#23755 = VECTOR ( 'NONE', #42693, 1000.000000000000000 ) ;
#23756 = FACE_OUTER_BOUND ( 'NONE', #33041, .T. ) ;
#23757 = CARTESIAN_POINT ( 'NONE',  ( 34.32915281903212446, -1.750000000000009326, 159.7931612910809065 ) ) ;
#23758 = DIRECTION ( 'NONE',  ( -1.000000000000000000, -0.000000000000000000, -0.000000000000000000 ) ) ;
#23759 = ORIENTED_EDGE ( 'NONE', *, *, #38878, .F. ) ;
#23760 = EDGE_LOOP ( 'NONE', ( #10327, #14785, #1845, #48649 ) ) ;
#23761 = DIRECTION ( 'NONE',  ( -1.000000000000000000, 1.586032892321652236E-16, 1.586032892321651989E-16 ) ) ;
#23762 = AXIS2_PLACEMENT_3D ( 'NONE', #41041, #33859, #2784 ) ;
#23763 = LINE ( 'NONE', #15042, #7914 ) ;
#23764 = EDGE_CURVE ( 'NONE', #48770, #46883, #9481, .T. ) ;
#23765 = DIRECTION ( 'NONE',  ( -1.586032892321652236E-16, -1.000000000000000000, -2.288264760618012091E-48 ) ) ;
#23766 = EDGE_LOOP ( 'NONE', ( #30684, #9488, #9826, #26676 ) ) ;
#23767 = ORIENTED_EDGE ( 'NONE', *, *, #41926, .F. ) ;
#23768 = DIRECTION ( 'NONE',  ( -1.000000000000000000, 0.000000000000000000, 0.000000000000000000 ) ) ;
#23769 = EDGE_LOOP ( 'NONE', ( #1645, #17406, #6687, #33480 ) ) ;
#23770 = DIRECTION ( 'NONE',  ( -0.000000000000000000, -0.000000000000000000, -1.000000000000000000 ) ) ;
#23771 = CARTESIAN_POINT ( 'NONE',  ( 153.2026953830863647, -97.66198943095992036, 23.74256005001722158 ) ) ;
#23772 = PLANE ( 'NONE',  #31896 ) ;
#23773 = CARTESIAN_POINT ( 'NONE',  ( -168.4459734468149747, -1.025126265847089879, 82.56828755692798438 ) ) ;
#23774 = ORIENTED_EDGE ( 'NONE', *, *, #25661, .T. ) ;
#23775 = LINE ( 'NONE', #11461, #40635 ) ;
#23776 = LINE ( 'NONE', #46567, #23210 ) ;
#23777 = DIRECTION ( 'NONE',  ( 1.000000000000000000, 0.000000000000000000, -4.758098676964956461E-16 ) ) ;
#23778 = LINE ( 'NONE', #5020, #45140 ) ;
#23779 =( BOUNDED_CURVE ( )  B_SPLINE_CURVE ( 3, ( #10314, #25710, #25972, #49511 ),
 .UNSPECIFIED., .F., .F. ) 
 B_SPLINE_CURVE_WITH_KNOTS ( ( 4, 4 ),
 ( 3.141592653589793116, 4.712388980384693227 ),
 .UNSPECIFIED. ) 
 CURVE ( )  GEOMETRIC_REPRESENTATION_ITEM ( )  RATIONAL_B_SPLINE_CURVE ( ( 1.000000000000000000, 0.8047378541243641603, 0.8047378541243641603, 1.000000000000000000 ) ) 
 REPRESENTATION_ITEM ( '' )  );
#23780 = LINE ( 'NONE', #11983, #48237 ) ;
#23781 =( BOUNDED_CURVE ( )  B_SPLINE_CURVE ( 3, ( #32583, #48167, #5360, #40027 ),
 .UNSPECIFIED., .F., .F. ) 
 B_SPLINE_CURVE_WITH_KNOTS ( ( 4, 4 ),
 ( 0.000000000000000000, 1.570796326794896558 ),
 .UNSPECIFIED. ) 
 CURVE ( )  GEOMETRIC_REPRESENTATION_ITEM ( )  RATIONAL_B_SPLINE_CURVE ( ( 1.000000000000000000, 0.8047378541243649375, 0.8047378541243649375, 1.000000000000000000 ) ) 
 REPRESENTATION_ITEM ( '' )  );
#23782 = CARTESIAN_POINT ( 'NONE',  ( 1.250000000000000222, 0.000000000000000000, -10.00000000000000000 ) ) ;
#23783 = CARTESIAN_POINT ( 'NONE',  ( 167.5000000000000000, 102.5000000000000142, 10.00000000000000000 ) ) ;
#23784 = EDGE_CURVE ( 'NONE', #16307, #10704, #13649, .T. ) ;
#23785 = VECTOR ( 'NONE', #2941, 1000.000000000000000 ) ;
#23786 = VERTEX_POINT ( 'NONE', #1037 ) ;
#23787 = VECTOR ( 'NONE', #16709, 1000.000000000000000 ) ;
#23788 = FACE_OUTER_BOUND ( 'NONE', #28959, .T. ) ;
#23789 = VECTOR ( 'NONE', #32490, 1000.000000000000000 ) ;
#23790 = ORIENTED_EDGE ( 'NONE', *, *, #31606, .T. ) ;
#23791 = LINE ( 'NONE', #43018, #16543 ) ;
#23792 = CARTESIAN_POINT ( 'NONE',  ( 181.0000000000000000, -272.4999999999999432, -339.9999999999998863 ) ) ;
#23793 = VECTOR ( 'NONE', #30964, 1000.000000000000000 ) ;
#23794 = CARTESIAN_POINT ( 'NONE',  ( 79.99999999999997158, 17.00000000000000000, -114.9999999999999858 ) ) ;
#23795 = COLOUR_RGB ( '',0.7921568627450980005, 0.8196078431372548767, 0.9333333333333333481 ) ;
#23796 = VERTEX_POINT ( 'NONE', #17187 ) ;
#23797 = CARTESIAN_POINT ( 'NONE',  ( 0.6126904405382156416, 1.085824959725723016, 9.981352469109932457 ) ) ;
#23798 = ORIENTED_EDGE ( 'NONE', *, *, #6798, .F. ) ;
#23799 = ORIENTED_EDGE ( 'NONE', *, *, #38401, .F. ) ;
#23800 = CARTESIAN_POINT ( 'NONE',  ( -1.222012661920452326, 0.2471648704738776681, 9.981352469109934233 ) ) ;
#23801 = CARTESIAN_POINT ( 'NONE',  ( 298.7932379171858770, -227.3959007404659474, 296.3011729072026696 ) ) ;
#23802 = EDGE_CURVE ( 'NONE', #34812, #29100, #48934, .T. ) ;
#23803 = EDGE_CURVE ( 'NONE', #21335, #26878, #30839, .T. ) ;
#23804 = EDGE_LOOP ( 'NONE', ( #3422, #12310, #46836, #7743 ) ) ;
#23805 = FACE_OUTER_BOUND ( 'NONE', #41508, .T. ) ;
#23806 = CARTESIAN_POINT ( 'NONE',  ( 115.0540265531850395, 2.143131898507847836E-16, -117.4317124430720725 ) ) ;
#23807 = EDGE_CURVE ( 'NONE', #9256, #16065, #40540, .T. ) ;
#23808 = LINE ( 'NONE', #969, #33344 ) ;
#23809 = ORIENTED_EDGE ( 'NONE', *, *, #18580, .T. ) ;
#23811 = EDGE_CURVE ( 'NONE', #19067, #38090, #44362, .T. ) ;
#23810 = LINE ( 'NONE', #12758, #20909 ) ;
#23812 = DIRECTION ( 'NONE',  ( 0.000000000000000000, 0.000000000000000000, 1.000000000000000000 ) ) ;
#23813 = EDGE_CURVE ( 'NONE', #9286, #16306, #2045, .T. ) ;
#23814 = CARTESIAN_POINT ( 'NONE',  ( 113.3040265531850537, -1.749999999999997335, 120.8182875569279702 ) ) ;
#23815 = ORIENTED_EDGE ( 'NONE', *, *, #39589, .T. ) ;
#23816 = DIRECTION ( 'NONE',  ( -1.000000000000000000, -0.000000000000000000, -0.000000000000000000 ) ) ;
#23817 = LINE ( 'NONE', #4317, #12218 ) ;
#23818 = ORIENTED_EDGE ( 'NONE', *, *, #30216, .T. ) ;
#23819 = VERTEX_POINT ( 'NONE', #12830 ) ;
#23820 = ORIENTED_EDGE ( 'NONE', *, *, #8244, .F. ) ;
#23821 = DIRECTION ( 'NONE',  ( -7.793956916774524585E-48, 0.000000000000000000, -1.000000000000000000 ) ) ;
#23822 = ADVANCED_FACE ( 'NONE', ( #24890 ), #13582, .F. ) ;
#23823 = DIRECTION ( 'NONE',  ( -1.000000000000000000, -0.000000000000000000, -0.000000000000000000 ) ) ;
#23824 = ORIENTED_EDGE ( 'NONE', *, *, #30895, .F. ) ;
#23825 = VECTOR ( 'NONE', #28020, 1000.000000000000114 ) ;
#23826 = CARTESIAN_POINT ( 'NONE',  ( -4.672045878990125800, 33.19353511768168374, 1.847720168420772691 ) ) ;
#23827 = DIRECTION ( 'NONE',  ( -1.000000000000000000, 0.000000000000000000, 0.000000000000000000 ) ) ;
#23828 = CARTESIAN_POINT ( 'NONE',  ( 340.0000000000000568, 181.0000000000000284, 355.9999999999998295 ) ) ;
#23829 = AXIS2_PLACEMENT_3D ( 'NONE', #41254, #21499, #49164 ) ;
#23830 = CYLINDRICAL_SURFACE ( 'NONE', #16179, 4.000000000000003553 ) ;
#23831 = CARTESIAN_POINT ( 'NONE',  ( -168.4459734468149463, 0.000000000000000000, -157.4317124430720582 ) ) ;
#23832 = CARTESIAN_POINT ( 'NONE',  ( 1.249999999999999778, 0.000000000000000000, 10.00000000000000000 ) ) ;
#23833 = DIRECTION ( 'NONE',  ( -0.000000000000000000, -0.000000000000000000, -1.000000000000000000 ) ) ;
#23834 = SURFACE_STYLE_USAGE ( .BOTH. , #3818 ) ;
#23835 = CARTESIAN_POINT ( 'NONE',  ( -14.99999999999782041, 17.00000000000000000, 95.00000000000000000 ) ) ;
#23836 = AXIS2_PLACEMENT_3D ( 'NONE', #49758, #7221, #14657 ) ;
#23837 = LINE ( 'NONE', #43064, #1073 ) ;
#23838 = VECTOR ( 'NONE', #15635, 1000.000000000000000 ) ;
#23839 = FACE_BOUND ( 'NONE', #11685, .T. ) ;
#23840 = DIRECTION ( 'NONE',  ( 0.000000000000000000, 0.000000000000000000, 1.000000000000000000 ) ) ;
#23841 = LINE ( 'NONE', #19295, #34915 ) ;
#23842 = FACE_OUTER_BOUND ( 'NONE', #8402, .T. ) ;
#23843 = CARTESIAN_POINT ( 'NONE',  ( -38.06347959788612201, 17.13191708601497609, -8.080361901872242569 ) ) ;
#23844 = VERTEX_POINT ( 'NONE', #17439 ) ;
#23845 = CARTESIAN_POINT ( 'NONE',  ( -4.999999999999997335, 204.9999999999999716, -234.7500000000000000 ) ) ;
#23846 = EDGE_CURVE ( 'NONE', #920, #32767, #33354, .T. ) ;
#23847 = DIRECTION ( 'NONE',  ( -1.000000000000000000, 0.000000000000000000, -0.000000000000000000 ) ) ;
#23848 = CARTESIAN_POINT ( 'NONE',  ( 35.00000000000091660, 17.00000000000000000, -24.99999999999999289 ) ) ;
#23849 = LINE ( 'NONE', #258, #7433 ) ;
#23850 = EDGE_CURVE ( 'NONE', #15777, #22294, #20775, .T. ) ;
#23851 = ORIENTED_EDGE ( 'NONE', *, *, #28462, .T. ) ;
#23852 = DIRECTION ( 'NONE',  ( -1.000000000000000000, -0.000000000000000000, -0.000000000000000000 ) ) ;
#23853 = ORIENTED_EDGE ( 'NONE', *, *, #4127, .T. ) ;
#23854 = CARTESIAN_POINT ( 'NONE',  ( -0.5000000000000000000, 0.5000000000000000000, 1000.000000000000000 ) ) ;
#23855 = VERTEX_POINT ( 'NONE', #13819 ) ;
#23856 = DIRECTION ( 'NONE',  ( 1.000000000000000000, 0.000000000000000000, -0.000000000000000000 ) ) ;
#23857 = CARTESIAN_POINT ( 'NONE',  ( -119.9999999999997158, 17.00000000000000000, -60.00000000000000000 ) ) ;
#23858 = EDGE_LOOP ( 'NONE', ( #44382, #46239, #7994, #8330, #17611, #27648 ) ) ;
#23859 = CARTESIAN_POINT ( 'NONE',  ( -206.6959734468149463, 1.750000000000009992, 160.8182875569279702 ) ) ;
#23860 = ORIENTED_EDGE ( 'NONE', *, *, #10516, .F. ) ;
#23861 = CIRCLE ( 'NONE', #30407, 0.5000000000000004441 ) ;
#23862 = EDGE_LOOP ( 'NONE', ( #40980, #13091, #49446, #974 ) ) ;
#23863 = FACE_OUTER_BOUND ( 'NONE', #27555, .T. ) ;
#23864 = CARTESIAN_POINT ( 'NONE',  ( 155.0540265531850537, 2.143131898507880377E-16, 122.5682875569279702 ) ) ;
#23865 = ORIENTED_EDGE ( 'NONE', *, *, #39328, .T. ) ;
#23866 = DIRECTION ( 'NONE',  ( 1.000000000000000000, 0.000000000000000000, 0.000000000000000000 ) ) ;
#23867 = CARTESIAN_POINT ( 'NONE',  ( 111.5540265531850537, 1.025126265847081442, -0.9317124430720195027 ) ) ;
#23868 = VECTOR ( 'NONE', #3412, 1000.000000000000000 ) ;
#23869 = CARTESIAN_POINT ( 'NONE',  ( 191.5540265531850537, 1.025126265847089213, 162.5682875569279133 ) ) ;
#23870 = VECTOR ( 'NONE', #12472, 1000.000000000000000 ) ;
#23871 = CARTESIAN_POINT ( 'NONE',  ( 210.0000000000000568, 0.000000000000000000, -159.1817124430720298 ) ) ;
#23872 = DIRECTION ( 'NONE',  ( 0.000000000000000000, -1.000000000000000000, 0.000000000000000000 ) ) ;
#23873 = VERTEX_POINT ( 'NONE', #44856 ) ;
#23874 = CARTESIAN_POINT ( 'NONE',  ( -4.641001526964560142, -50.00000000000000711, -8.016098858316199838 ) ) ;
#23875 = CARTESIAN_POINT ( 'NONE',  ( 155.0540265531850537, 2.143131898507880377E-16, 42.56828755692798438 ) ) ;
#23876 = ORIENTED_EDGE ( 'NONE', *, *, #41883, .F. ) ;
#23877 = CARTESIAN_POINT ( 'NONE',  ( 0.000000000000000000, 17.00000000000000000, 0.000000000000000000 ) ) ;
#23878 = EDGE_CURVE ( 'NONE', #12755, #27291, #25391, .T. ) ;
#23879 = FACE_OUTER_BOUND ( 'NONE', #4752, .T. ) ;
#23880 = ORIENTED_EDGE ( 'NONE', *, *, #29405, .F. ) ;
#23881 = CARTESIAN_POINT ( 'NONE',  ( -1.042245359060422816, -0.7067879234688214662, 9.974012008644017158 ) ) ;
#23882 = CARTESIAN_POINT ( 'NONE',  ( 0.3862712429686894766, -1.188820645368940276, -10.00000000000000000 ) ) ;
#23883 = CARTESIAN_POINT ( 'NONE',  ( 152.2789002873379900, 1.750000000000009326, -158.1565861772249377 ) ) ;
#23884 = CYLINDRICAL_SURFACE ( 'NONE', #14090, 2.000000000000001776 ) ;
#23885 = ORIENTED_EDGE ( 'NONE', *, *, #16405, .F. ) ;
#23886 = CARTESIAN_POINT ( 'NONE',  ( 0.000000000000000000, 17.00000000000000000, 0.000000000000000000 ) ) ;
#23887 = CARTESIAN_POINT ( 'NONE',  ( 135.0000000000009663, 17.00000000000000000, -24.99999999999999289 ) ) ;
#23888 = VECTOR ( 'NONE', #3565, 1000.000000000000000 ) ;
#23889 = CARTESIAN_POINT ( 'NONE',  ( 44.99506233596247995, 23.32283626942318833, 7.455576670931136185 ) ) ;
#23890 = ORIENTED_EDGE ( 'NONE', *, *, #15994, .F. ) ;
#23892 = ORIENTED_EDGE ( 'NONE', *, *, #9042, .T. ) ;
#23891 = AXIS2_PLACEMENT_3D ( 'NONE', #39742, #12778, #35898 ) ;
#23893 = DIRECTION ( 'NONE',  ( 1.000000000000000000, -1.043609643147651723E-14, -1.744890010039029680E-14 ) ) ;
#23894 = CARTESIAN_POINT ( 'NONE',  ( -208.4459734468148611, 1.025126265847089657, -80.93171244307201562 ) ) ;
#23895 = PLANE ( 'NONE',  #30764 ) ;
#23896 = CARTESIAN_POINT ( 'NONE',  ( 356.0000000000000000, -165.0000000000001137, -94.00000000000019895 ) ) ;
#23897 = CARTESIAN_POINT ( 'NONE',  ( 111.5540265531850679, 0.000000000000000000, -0.9317124430719969652 ) ) ;
#23898 = ORIENTED_EDGE ( 'NONE', *, *, #38861, .F. ) ;
#23899 = CARTESIAN_POINT ( 'NONE',  ( 343.9999999999999432, -185.0000000000000284, 359.9999999999998295 ) ) ;
#23901 = CIRCLE ( 'NONE', #5873, 1.750000000000001554 ) ;
#23900 = CARTESIAN_POINT ( 'NONE',  ( 224.9999999999999716, -164.9999999999999716, 444.9999999999998295 ) ) ;
#23902 = DIRECTION ( 'NONE',  ( 1.000000000000000000, 0.000000000000000000, 0.000000000000000000 ) ) ;
#23903 = LINE ( 'NONE', #12344, #13321 ) ;
#23904 = EDGE_LOOP ( 'NONE', ( #45073, #166, #23890, #49695 ) ) ;
#23905 = CARTESIAN_POINT ( 'NONE',  ( 35.00000000000061107, 17.00000000000000000, -30.00000000000000000 ) ) ;
#23906 = EDGE_LOOP ( 'NONE', ( #2299, #18276, #50072 ) ) ;
#23907 = DIRECTION ( 'NONE',  ( 0.000000000000000000, 0.000000000000000000, 1.000000000000000000 ) ) ;
#23908 = EDGE_LOOP ( 'NONE', ( #15718, #26406, #38888, #16487 ) ) ;
#23909 = CARTESIAN_POINT ( 'NONE',  ( 0.3370904143228959926, -0.2449105217885284291, 10.00000000000000000 ) ) ;
#23910 = CARTESIAN_POINT ( 'NONE',  ( -207.7210997126620384, -1.750000000000009548, 159.7931612910809065 ) ) ;
#23911 = LINE ( 'NONE', #16974, #6003 ) ;
#23912 = CARTESIAN_POINT ( 'NONE',  ( 195.0540265531851105, 1.025126265847089657, 42.56828755692799149 ) ) ;
#23913 = ORIENTED_EDGE ( 'NONE', *, *, #5449, .F. ) ;
#23914 =( BOUNDED_CURVE ( )  B_SPLINE_CURVE ( 3, ( #17353, #44783, #41200, #33282 ),
 .UNSPECIFIED., .F., .F. ) 
 B_SPLINE_CURVE_WITH_KNOTS ( ( 4, 4 ),
 ( 0.000000000000000000, 1.570796326794896558 ),
 .UNSPECIFIED. ) 
 CURVE ( )  GEOMETRIC_REPRESENTATION_ITEM ( )  RATIONAL_B_SPLINE_CURVE ( ( 1.000000000000000000, 0.8047378541243649375, 0.8047378541243649375, 1.000000000000000000 ) ) 
 REPRESENTATION_ITEM ( '' )  );
#23915 = LINE ( 'NONE', #4169, #8928 ) ;
#23916 = CYLINDRICAL_SURFACE ( 'NONE', #25429, 1.750000000000001554 ) ;
#23917 = VERTEX_POINT ( 'NONE', #29491 ) ;
#23918 = CARTESIAN_POINT ( 'NONE',  ( -8.445973446814976526, 0.000000000000000000, -0.9317124430720524764 ) ) ;
#23919 = CARTESIAN_POINT ( 'NONE',  ( 153.3040265531850537, -1.750000000000010658, 120.8182875569279702 ) ) ;
#23920 = CARTESIAN_POINT ( 'NONE',  ( 35.05402655318504657, 1.025126265847089879, 82.56828755692798438 ) ) ;
#23921 = CARTESIAN_POINT ( 'NONE',  ( -5.647304616913629616, 2.688010569040066411, 23.74256005001722158 ) ) ;
#23922 =( BOUNDED_CURVE ( )  B_SPLINE_CURVE ( 3, ( #41991, #22241, #37913, #49641 ),
 .UNSPECIFIED., .F., .F. ) 
 B_SPLINE_CURVE_WITH_KNOTS ( ( 4, 4 ),
 ( 3.141592653589793116, 4.712388980384689674 ),
 .UNSPECIFIED. ) 
 CURVE ( )  GEOMETRIC_REPRESENTATION_ITEM ( )  RATIONAL_B_SPLINE_CURVE ( ( 1.000000000000000000, 0.8047378541243649375, 0.8047378541243649375, 1.000000000000000000 ) ) 
 REPRESENTATION_ITEM ( '' )  );
#23923 = VECTOR ( 'NONE', #25200, 1000.000000000000000 ) ;
#23924 = ORIENTED_EDGE ( 'NONE', *, *, #31152, .F. ) ;
#23925 = ORIENTED_EDGE ( 'NONE', *, *, #37750, .F. ) ;
#23926 = DIRECTION ( 'NONE',  ( -0.000000000000000000, -0.000000000000000000, -1.000000000000000000 ) ) ;
#23927 = ORIENTED_EDGE ( 'NONE', *, *, #44105, .T. ) ;
#23928 = AXIS2_PLACEMENT_3D ( 'NONE', #14431, #21620, #13672 ) ;
#23929 = CARTESIAN_POINT ( 'NONE',  ( 344.0000000000000000, 175.0000000000000284, -106.0000000000001990 ) ) ;
#23930 = CARTESIAN_POINT ( 'NONE',  ( 154.3291528190321458, -1.750000000000009548, 81.84341382277507648 ) ) ;
#23931 = CARTESIAN_POINT ( 'NONE',  ( 35.05402655318504657, -1.025126265847089657, -120.9317124430720440 ) ) ;
#23932 = VERTEX_POINT ( 'NONE', #36456 ) ;
#23933 = CARTESIAN_POINT ( 'NONE',  ( -28.52604530808686079, -41.07801380285659576, -3.760136334089591248 ) ) ;
#23934 = ADVANCED_FACE ( 'NONE', ( #45109 ), #1296, .T. ) ;
#23935 = VERTEX_POINT ( 'NONE', #16945 ) ;
#23936 =( BOUNDED_CURVE ( )  B_SPLINE_CURVE ( 3, ( #45174, #42548, #23056, #38727 ),
 .UNSPECIFIED., .F., .F. ) 
 B_SPLINE_CURVE_WITH_KNOTS ( ( 4, 4 ),
 ( 0.000000000000000000, 1.570796326794896558 ),
 .UNSPECIFIED. ) 
 CURVE ( )  GEOMETRIC_REPRESENTATION_ITEM ( )  RATIONAL_B_SPLINE_CURVE ( ( 1.000000000000000000, 0.8047378541243649375, 0.8047378541243649375, 1.000000000000000000 ) ) 
 REPRESENTATION_ITEM ( '' )  );
#23937 = VERTEX_POINT ( 'NONE', #32599 ) ;
#23938 = EDGE_CURVE ( 'NONE', #27459, #5553, #48183, .T. ) ;
#23939 = DIRECTION ( 'NONE',  ( 0.000000000000000000, 0.000000000000000000, 1.000000000000000000 ) ) ;
#23940 = EDGE_CURVE ( 'NONE', #42175, #4762, #32857, .T. ) ;
#23941 = CARTESIAN_POINT ( 'NONE',  ( -1.066995270233474624, 50.00000000000000711, -3.760136334089591248 ) ) ;
#23942 = VERTEX_POINT ( 'NONE', #44600 ) ;
#23943 = ORIENTED_EDGE ( 'NONE', *, *, #25726, .T. ) ;
#23944 = ORIENTED_EDGE ( 'NONE', *, *, #28633, .T. ) ;
#23945 = LINE ( 'NONE', #3419, #39441 ) ;
#23946 = CARTESIAN_POINT ( 'NONE',  ( 115.0540265531850395, 2.143131898507847836E-16, -117.4317124430720725 ) ) ;
#23947 = DIRECTION ( 'NONE',  ( 0.000000000000000000, 0.000000000000000000, -1.000000000000000000 ) ) ;
#23948 = AXIS2_PLACEMENT_3D ( 'NONE', #10607, #26271, #41911 ) ;
#23949 = ADVANCED_FACE ( 'NONE', ( #25147 ), #40791, .T. ) ;
#23950 = ORIENTED_EDGE ( 'NONE', *, *, #31352, .F. ) ;
#23951 = FACE_OUTER_BOUND ( 'NONE', #46554, .T. ) ;
#23952 = EDGE_LOOP ( 'NONE', ( #47469, #20083, #37706, #35222 ) ) ;
#23953 = CARTESIAN_POINT ( 'NONE',  ( -16.02661358026017879, -4.530191650547607196, -9.683996418299976483 ) ) ;
#23954 = ORIENTED_EDGE ( 'NONE', *, *, #33677, .T. ) ;
#23955 = ADVANCED_FACE ( 'NONE', ( #34115 ), #42043, .T. ) ;
#23956 = DIRECTION ( 'NONE',  ( 1.000000000000000000, 0.000000000000000000, 0.000000000000000000 ) ) ;
#23957 = CARTESIAN_POINT ( 'NONE',  ( 85.00000000000056843, 17.00000000000000000, -54.99999999999999289 ) ) ;
#23958 = CARTESIAN_POINT ( 'NONE',  ( -2.538055338523173443, -50.00000000000000000, -9.367992836599951190 ) ) ;
#23959 = DIRECTION ( 'NONE',  ( -0.4055129968046615185, 0.4055129968046615185, -0.8192181753629523833 ) ) ;
#23960 = CARTESIAN_POINT ( 'NONE',  ( 135.0000000000000000, 17.00000000000000000, -114.9999999999999858 ) ) ;
#23961 = CARTESIAN_POINT ( 'NONE',  ( 4.672045878990125800, -50.00000000000000711, 1.847720168420772691 ) ) ;
#23962 = VERTEX_POINT ( 'NONE', #45358 ) ;
#23963 = EDGE_LOOP ( 'NONE', ( #1272, #20146, #10297 ) ) ;
#23964 = CARTESIAN_POINT ( 'NONE',  ( -128.4459734468149179, 0.000000000000000000, -120.9317124430720156 ) ) ;
#23965 = AXIS2_PLACEMENT_3D ( 'NONE', #20600, #36280, #48010 ) ;
#23966 = CARTESIAN_POINT ( 'NONE',  ( -40.32982405930701475, -10.56057144604259079, -9.387872844313825738 ) ) ;
#23967 = CARTESIAN_POINT ( 'NONE',  ( 153.3040265531850537, 0.000000000000000000, 165.0000000000000000 ) ) ;
#23968 = EDGE_CURVE ( 'NONE', #37688, #20047, #22293, .T. ) ;
#23969 = EDGE_CURVE ( 'NONE', #11650, #7708, #46216, .T. ) ;
#23970 = CIRCLE ( 'NONE', #31378, 4.000000000000003553 ) ;
#23971 = ADVANCED_FACE ( 'NONE', ( #14590 ), #35950, .T. ) ;
#23972 = EDGE_CURVE ( 'NONE', #40787, #11639, #10494, .T. ) ;
#23973 = CARTESIAN_POINT ( 'NONE',  ( 15.00000000000000000, -46.51315789473684248, -6.315789473684215949 ) ) ;
#23974 = VECTOR ( 'NONE', #7583, 1000.000000000000000 ) ;
#23975 = CARTESIAN_POINT ( 'NONE',  ( 358.3431457505076310, 165.0000000000002274, -340.0000000000002842 ) ) ;
#23976 = ADVANCED_FACE ( 'NONE', ( #41544 ), #37710, .T. ) ;
#23977 = VERTEX_POINT ( 'NONE', #7156 ) ;
#23978 = CARTESIAN_POINT ( 'NONE',  ( -114.9999999999994031, 16.00000000000000000, -54.99999999999999289 ) ) ;
#23979 = EDGE_CURVE ( 'NONE', #48228, #13812, #29841, .T. ) ;
#23980 = CARTESIAN_POINT ( 'NONE',  ( 2.500000000000003997, 194.9999999999999716, -240.0000000000000000 ) ) ;
#23981 = ORIENTED_EDGE ( 'NONE', *, *, #3386, .F. ) ;
#23982 = DIRECTION ( 'NONE',  ( 0.000000000000000000, 0.000000000000000000, -1.000000000000000000 ) ) ;
#23983 = CARTESIAN_POINT ( 'NONE',  ( 10.49999999999996092, 13.48684210526315574, -20.00000000000000000 ) ) ;
#23984 = DIRECTION ( 'NONE',  ( 0.000000000000000000, -1.000000000000000000, 0.000000000000000000 ) ) ;
#23985 = VECTOR ( 'NONE', #34174, 1000.000000000000000 ) ;
#23986 = VERTEX_POINT ( 'NONE', #41786 ) ;
#23987 = VERTEX_POINT ( 'NONE', #15103 ) ;
#23988 = EDGE_CURVE ( 'NONE', #25227, #7200, #30500, .T. ) ;
#23989 = LINE ( 'NONE', #11938, #35749 ) ;
#23990 = CARTESIAN_POINT ( 'NONE',  ( -1.011271242968693862, 0.7347315653655780432, 10.00000000000000000 ) ) ;
#23991 = EDGE_CURVE ( 'NONE', #47198, #45035, #445, .T. ) ;
#23992 = EDGE_LOOP ( 'NONE', ( #25087, #17491, #14790, #8503 ) ) ;
#23993 = EDGE_CURVE ( 'NONE', #31669, #20047, #37970, .T. ) ;
#23994 = ORIENTED_EDGE ( 'NONE', *, *, #48664, .F. ) ;
#23995 = CARTESIAN_POINT ( 'NONE',  ( 31.55402655318503236, 0.000000000000000000, 119.0682875569279702 ) ) ;
#23996 = DIRECTION ( 'NONE',  ( 0.000000000000000000, 0.2223603367690656640, 0.9749645535258950613 ) ) ;
#23997 = DIRECTION ( 'NONE',  ( 1.000000000000000000, 0.000000000000000000, -0.000000000000000000 ) ) ;
#23998 = CARTESIAN_POINT ( 'NONE',  ( 10.49999999999996447, 8.875661936878628921, -18.94832733001756253 ) ) ;
#23999 = CARTESIAN_POINT ( 'NONE',  ( 181.0000000000000000, -97.49999999999998579, -350.0000000000001705 ) ) ;
#24000 = VECTOR ( 'NONE', #33990, 1000.000000000000000 ) ;
#24001 = ORIENTED_EDGE ( 'NONE', *, *, #26811, .T. ) ;
#24002 = ORIENTED_EDGE ( 'NONE', *, *, #22363, .F. ) ;
#24003 = VECTOR ( 'NONE', #2739, 1000.000000000000000 ) ;
#24004 = ORIENTED_EDGE ( 'NONE', *, *, #43769, .T. ) ;
#24005 = B_SPLINE_CURVE_WITH_KNOTS ( 'NONE', 3,
 ( #38095, #2906, #49820, #23452 ),
 .UNSPECIFIED., .F., .F.,
 ( 4, 4 ),
 ( 0.0006669682284780878911, 0.0007799402130919236807 ),
 .UNSPECIFIED. ) ;
#24006 = VECTOR ( 'NONE', #14299, 1000.000000000000000 ) ;
#24007 = ADVANCED_FACE ( 'NONE', ( #3037 ), #30007, .T. ) ;
#24008 = DIRECTION ( 'NONE',  ( -7.793956916774524585E-48, 0.000000000000000000, -1.000000000000000000 ) ) ;
#24009 = ORIENTED_EDGE ( 'NONE', *, *, #48063, .T. ) ;
#24010 = VECTOR ( 'NONE', #24982, 1000.000000000000000 ) ;
#24011 = DIRECTION ( 'NONE',  ( 1.000000000000000000, -0.000000000000000000, 0.000000000000000000 ) ) ;
#24012 = VERTEX_POINT ( 'NONE', #49196 ) ;
#24013 = VERTEX_POINT ( 'NONE', #14081 ) ;
#24014 = DIRECTION ( 'NONE',  ( 0.000000000000000000, 0.000000000000000000, 1.000000000000000000 ) ) ;
#24015 = DIRECTION ( 'NONE',  ( -0.000000000000000000, -0.000000000000000000, 1.000000000000000000 ) ) ;
#24016 = ORIENTED_EDGE ( 'NONE', *, *, #16404, .F. ) ;
#24017 = VERTEX_POINT ( 'NONE', #43562 ) ;
#24019 = EDGE_CURVE ( 'NONE', #2059, #13008, #16017, .T. ) ;
#24018 = ADVANCED_BREP_SHAPE_REPRESENTATION ( '', ( #5950, #45486 ), #11091 ) ;
#24020 = LINE ( 'NONE', #39674, #34824 ) ;
#24021 = CARTESIAN_POINT ( 'NONE',  ( 35.05402655318504657, 1.025126265847089435, -157.4317124430720582 ) ) ;
#24022 = ORIENTED_EDGE ( 'NONE', *, *, #15278, .T. ) ;
#24023 = DIRECTION ( 'NONE',  ( 0.000000000000000000, -0.9230769230769231282, 0.3846153846153845812 ) ) ;
#24024 = FACE_OUTER_BOUND ( 'NONE', #40152, .T. ) ;
#24025 = CARTESIAN_POINT ( 'NONE',  ( 151.5540265531850537, 0.000000000000000000, -157.4317124430720582 ) ) ;
#24026 =( BOUNDED_CURVE ( )  B_SPLINE_CURVE ( 3, ( #10260, #20785, #36467, #37235 ),
 .UNSPECIFIED., .F., .F. ) 
 B_SPLINE_CURVE_WITH_KNOTS ( ( 4, 4 ),
 ( 4.712388980384689674, 6.283185307179586232 ),
 .UNSPECIFIED. ) 
 CURVE ( )  GEOMETRIC_REPRESENTATION_ITEM ( )  RATIONAL_B_SPLINE_CURVE ( ( 1.000000000000000000, 0.8047378541243649375, 0.8047378541243649375, 1.000000000000000000 ) ) 
 REPRESENTATION_ITEM ( '' )  );
#24027 = ADVANCED_FACE ( 'NONE', ( #31022 ), #19189, .F. ) ;
#24028 = DIRECTION ( 'NONE',  ( -0.000000000000000000, -0.000000000000000000, -1.000000000000000000 ) ) ;
#24029 = ORIENTED_EDGE ( 'NONE', *, *, #20906, .F. ) ;
#24030 = DIRECTION ( 'NONE',  ( -0.000000000000000000, -0.000000000000000000, -1.000000000000000000 ) ) ;
#24031 = CARTESIAN_POINT ( 'NONE',  ( -0.02889939370780074401, 1.394750214493988283, 9.955131761384901523 ) ) ;
#24032 = CARTESIAN_POINT ( 'NONE',  ( 168.9999999999999716, -272.4999999999999432, -341.9999999999999432 ) ) ;
#24033 = CARTESIAN_POINT ( 'NONE',  ( 80.00000000000092371, 16.00000000000000000, -24.99999999999999289 ) ) ;
#24034 = EDGE_CURVE ( 'NONE', #5399, #13539, #46820, .T. ) ;
#24035 = EDGE_CURVE ( 'NONE', #19888, #50159, #25282, .T. ) ;
#24036 = VECTOR ( 'NONE', #6360, 1000.000000000000000 ) ;
#24037 =( REPRESENTATION_RELATIONSHIP ('NONE','NONE', #45699, #3157 ) REPRESENTATION_RELATIONSHIP_WITH_TRANSFORMATION ( #32872 )SHAPE_REPRESENTATION_RELATIONSHIP( ) );
#24038 = EDGE_CURVE ( 'NONE', #5374, #42585, #22550, .T. ) ;
#24039 = CARTESIAN_POINT ( 'NONE',  ( 168.9999999999999716, -7.999999999999952038, 339.9999999999998295 ) ) ;
#24040 = VECTOR ( 'NONE', #1938, 1000.000000000000000 ) ;
#24041 = EDGE_CURVE ( 'NONE', #14784, #2021, #11764, .T. ) ;
#24042 = LINE ( 'NONE', #20940, #29111 ) ;
#24043 = CARTESIAN_POINT ( 'NONE',  ( -168.4459734468149747, 2.143131898507880377E-16, -160.9317124430720298 ) ) ;
#24044 = AXIS2_PLACEMENT_3D ( 'NONE', #3249, #34577, #34081 ) ;
#24045 = EDGE_CURVE ( 'NONE', #2948, #5419, #46286, .T. ) ;
#24046 = EDGE_CURVE ( 'NONE', #42094, #36068, #720, .T. ) ;
#24047 = ORIENTED_EDGE ( 'NONE', *, *, #42164, .T. ) ;
#24048 = DIRECTION ( 'NONE',  ( 0.000000000000000000, 0.000000000000000000, -1.000000000000000000 ) ) ;
#24049 = VECTOR ( 'NONE', #25163, 1000.000000000000000 ) ;
#24050 = CARTESIAN_POINT ( 'NONE',  ( 0.2773062244624638351, -1.251557370488896481, 9.948547179989619238 ) ) ;
#24051 = VERTEX_POINT ( 'NONE', #227 ) ;
#24052 = CARTESIAN_POINT ( 'NONE',  ( -85.67084718096784002, -1.750000000000009548, -78.15658617722490931 ) ) ;
#24053 = FACE_OUTER_BOUND ( 'NONE', #18677, .T. ) ;
#24054 = DIRECTION ( 'NONE',  ( -0.000000000000000000, -1.000000000000000000, -0.000000000000000000 ) ) ;
#24055 = ORIENTED_EDGE ( 'NONE', *, *, #49008, .F. ) ;
#24056 = CARTESIAN_POINT ( 'NONE',  ( 33.30402655318503946, 0.000000000000000000, 165.0000000000000000 ) ) ;
#24057 = B_SPLINE_SURFACE_WITH_KNOTS ( 'NONE', 3, 3, ( 
 ( #44, #31854, #16193, #24154 ),
 ( #15676, #35719, #31348, #12578 ),
 ( #16683, #4139, #43370, #299 ),
 ( #15941, #31609, #47194, #4648 ) ),
 .UNSPECIFIED., .F., .F., .F.,
 ( 4, 4 ),
 ( 4, 4 ),
 ( 0.000000000000000000, 1.000000000000000000 ),
 ( 0.000000000000000000, 1.000000000000000000 ),
 .UNSPECIFIED. ) ;
#24058 = ORIENTED_EDGE ( 'NONE', *, *, #43451, .T. ) ;
#24059 = VERTEX_POINT ( 'NONE', #43303 ) ;
#24060 = FACE_OUTER_BOUND ( 'NONE', #11396, .T. ) ;
#24061 = CARTESIAN_POINT ( 'NONE',  ( -6.695973446814940111, 1.750000000000024203, 80.81828755692798438 ) ) ;
#24062 = ORIENTED_EDGE ( 'NONE', *, *, #11881, .F. ) ;
#24063 = EDGE_CURVE ( 'NONE', #15809, #10936, #42540, .T. ) ;
#24064 = CARTESIAN_POINT ( 'NONE',  ( -1.335416683881408995, 0.4035165624839831544, 9.955131761384903299 ) ) ;
#24065 = CARTESIAN_POINT ( 'NONE',  ( 344.0000000000000568, 167.0000000000000000, 341.9999999999998863 ) ) ;
#24066 = ORIENTED_EDGE ( 'NONE', *, *, #38775, .T. ) ;
#24067 = DIRECTION ( 'NONE',  ( 0.000000000000000000, 0.000000000000000000, 1.000000000000000000 ) ) ;
#24068 = ORIENTED_EDGE ( 'NONE', *, *, #23096, .F. ) ;
#24069 = DIRECTION ( 'NONE',  ( 0.000000000000000000, 0.000000000000000000, -1.000000000000000000 ) ) ;
#24070 = CYLINDRICAL_SURFACE ( 'NONE', #19318, 1.750000000000015543 ) ;
#24071 = CARTESIAN_POINT ( 'NONE',  ( -164.4973046169135955, -98.56198943095992604, -18.45589678844777382 ) ) ;
#24072 = ORIENTED_EDGE ( 'NONE', *, *, #29686, .T. ) ;
#24073 = DIRECTION ( 'NONE',  ( 0.000000000000000000, 0.000000000000000000, -1.000000000000000000 ) ) ;
#24074 = AXIS2_PLACEMENT_3D ( 'NONE', #13215, #20405, #1931 ) ;
#24075 = CARTESIAN_POINT ( 'NONE',  ( 359.9999999999999432, -181.0000000000001421, 356.0000000000000000 ) ) ;
#24076 = AXIS2_PLACEMENT_3D ( 'NONE', #25951, #21575, #33645 ) ;
#24077 = VERTEX_POINT ( 'NONE', #7930 ) ;
#24078 = ORIENTED_EDGE ( 'NONE', *, *, #30935, .F. ) ;
#24079 = ORIENTED_EDGE ( 'NONE', *, *, #14396, .F. ) ;
#24080 = CARTESIAN_POINT ( 'NONE',  ( -14.99999999999876366, 17.00000000000000000, 5.000000000000004441 ) ) ;
#24081 = AXIS2_PLACEMENT_3D ( 'NONE', #8941, #11785, #39245 ) ;
#24082 = CARTESIAN_POINT ( 'NONE',  ( 155.0540265531850537, -1.025126265847088991, 2.568287556927986159 ) ) ;
#24083 = ORIENTED_EDGE ( 'NONE', *, *, #48331, .T. ) ;
#24084=STYLED_ITEM('',(#50747),#39561);
#24085 = CARTESIAN_POINT ( 'NONE',  ( 339.9999999999999432, -168.9999999999999432, -344.0000000000001705 ) ) ;
#24086 = DIRECTION ( 'NONE',  ( 1.000000000000000000, 0.000000000000000000, 0.000000000000000000 ) ) ;
#24087 = VECTOR ( 'NONE', #19977, 1000.000000000000000 ) ;
#24088 = CARTESIAN_POINT ( 'NONE',  ( -14.76429217231967428, -8.192625680377590314, 9.178419661560148768 ) ) ;
#24089 =( BOUNDED_CURVE ( )  B_SPLINE_CURVE ( 3, ( #11305, #26195, #34408, #38519 ),
 .UNSPECIFIED., .F., .F. ) 
 B_SPLINE_CURVE_WITH_KNOTS ( ( 4, 4 ),
 ( 0.000000000000000000, 1.570796326794896558 ),
 .UNSPECIFIED. ) 
 CURVE ( )  GEOMETRIC_REPRESENTATION_ITEM ( )  RATIONAL_B_SPLINE_CURVE ( ( 1.000000000000000000, 0.8047378541243649375, 0.8047378541243649375, 1.000000000000000000 ) ) 
 REPRESENTATION_ITEM ( '' )  );
#24090 = DIRECTION ( 'NONE',  ( 3.469446951953611724E-16, 0.000000000000000000, 1.000000000000000000 ) ) ;
#24091 = PLANE ( 'NONE',  #23891 ) ;
#24092 = FACE_BOUND ( 'NONE', #24332, .T. ) ;
#24093 = DIRECTION ( 'NONE',  ( -0.000000000000000000, -0.000000000000000000, 1.000000000000000000 ) ) ;
#24094 = FILL_AREA_STYLE ('',( #19970 ) ) ;
#24095 =( BOUNDED_CURVE ( )  B_SPLINE_CURVE ( 3, ( #21864, #5944, #45165, #25453 ),
 .UNSPECIFIED., .F., .F. ) 
 B_SPLINE_CURVE_WITH_KNOTS ( ( 4, 4 ),
 ( 1.570796326794896558, 3.141592653589793116 ),
 .UNSPECIFIED. ) 
 CURVE ( )  GEOMETRIC_REPRESENTATION_ITEM ( )  RATIONAL_B_SPLINE_CURVE ( ( 1.000000000000000000, 0.8047378541243649375, 0.8047378541243649375, 1.000000000000000000 ) ) 
 REPRESENTATION_ITEM ( '' )  );
#24096 = CARTESIAN_POINT ( 'NONE',  ( -64.99999999999877787, 17.00000000000000000, 5.000000000000004441 ) ) ;
#24097 = FACE_OUTER_BOUND ( 'NONE', #33409, .T. ) ;
#24098 = DIRECTION ( 'NONE',  ( 0.000000000000000000, 1.000000000000000000, 0.000000000000000000 ) ) ;
#24099 = EDGE_CURVE ( 'NONE', #15667, #16553, #39228, .T. ) ;
#24100 = CIRCLE ( 'NONE', #31456, 2.000000000000001776 ) ;
#24101 = ADVANCED_FACE ( 'NONE', ( #19957 ), #480, .F. ) ;
#24102 = DIRECTION ( 'NONE',  ( 3.469446951953616950E-15, 0.000000000000000000, -1.000000000000000000 ) ) ;
#24103 = CARTESIAN_POINT ( 'NONE',  ( 152.2789002873379900, 1.750000000000010436, 119.7931612910808781 ) ) ;
#24104 = VERTEX_POINT ( 'NONE', #47625 ) ;
#24105 = CARTESIAN_POINT ( 'NONE',  ( -177.4999999999999716, -112.5000000000000000, -10.00000000000000000 ) ) ;
#24106 = ADVANCED_FACE ( 'NONE', ( #38718 ), #34878, .F. ) ;
#24107 = DIRECTION ( 'NONE',  ( 0.000000000000000000, 1.000000000000000000, 0.000000000000000000 ) ) ;
#24108 = CARTESIAN_POINT ( 'NONE',  ( -4.999999999999997335, 214.9999999999999716, -234.7500000000000000 ) ) ;
#24109 = CARTESIAN_POINT ( 'NONE',  ( -49.67735855322972327, 8.912210285362091255, 8.356839323120299312 ) ) ;
#24110 = B_SPLINE_CURVE_WITH_KNOTS ( 'NONE', 3,
 ( #43816, #48130, #8930, #24584 ),
 .UNSPECIFIED., .F., .F.,
 ( 4, 4 ),
 ( 0.0006669682284780878911, 0.0007799402130920260294 ),
 .UNSPECIFIED. ) ;
#24111 = ADVANCED_FACE ( 'NONE', ( #12512 ), #50458, .F. ) ;
#24112 = EDGE_CURVE ( 'NONE', #11165, #26268, #43049, .T. ) ;
#24113 = ORIENTED_EDGE ( 'NONE', *, *, #14270, .F. ) ;
#24114 = PRESENTATION_STYLE_ASSIGNMENT (( #1008 ) ) ;
#24115 = VECTOR ( 'NONE', #1283, 1000.000000000000000 ) ;
#24116 = CARTESIAN_POINT ( 'NONE',  ( 164.9999999999999716, -93.49999999999998579, -350.0000000000001705 ) ) ;
#24117 = VECTOR ( 'NONE', #43792, 1000.000000000000000 ) ;
#24118 = ORIENTED_EDGE ( 'NONE', *, *, #14543, .T. ) ;
#24119 = DIRECTION ( 'NONE',  ( -0.4740998230350175202, -0.3386427307392980701, -0.8127425537743157014 ) ) ;
#24120 = AXIS2_PLACEMENT_3D ( 'NONE', #7192, #2569, #50227 ) ;
#24121 = CARTESIAN_POINT ( 'NONE',  ( 344.0000000000000568, 167.0000000000000000, 341.9999999999998863 ) ) ;
#24122 = DIRECTION ( 'NONE',  ( 1.000000000000000000, 0.000000000000000000, 0.000000000000000000 ) ) ;
#24123 = EDGE_CURVE ( 'NONE', #36125, #19216, #46614, .T. ) ;
#24124 = ORIENTED_EDGE ( 'NONE', *, *, #28791, .T. ) ;
#24125 = DIRECTION ( 'NONE',  ( -3.172065784643302499E-16, -1.000000000000000000, 0.000000000000000000 ) ) ;
#24126 = EDGE_LOOP ( 'NONE', ( #5875, #21768 ) ) ;
#24127 = AXIS2_PLACEMENT_3D ( 'NONE', #12809, #28468, #24125 ) ;
#24128 = EDGE_LOOP ( 'NONE', ( #26834, #38204, #38373, #41404, #39733, #32127 ) ) ;
#24129 = DIRECTION ( 'NONE',  ( 1.000000000000000000, 0.000000000000000000, 0.000000000000000000 ) ) ;
#24130 = CARTESIAN_POINT ( 'NONE',  ( -0.4426377647354682865, -1.666766018367764834, 9.928159647716134018 ) ) ;
#24131 = ORIENTED_EDGE ( 'NONE', *, *, #26022, .T. ) ;
#24132 = CARTESIAN_POINT ( 'NONE',  ( 167.0000000000000000, -174.9999999999999716, -99.00000000000014211 ) ) ;
#24133 = CARTESIAN_POINT ( 'NONE',  ( -1.114871695981121125, 0.4953159757245923500, 9.963925895596188909 ) ) ;
#24134 = CARTESIAN_POINT ( 'NONE',  ( 214.9999999999999432, -172.9999999999999716, 252.0000000000000000 ) ) ;
#24135 = CARTESIAN_POINT ( 'NONE',  ( -69.99999999999879208, 17.00000000000000000, 5.000000000000004441 ) ) ;
#24136 = ORIENTED_EDGE ( 'NONE', *, *, #36339, .T. ) ;
#24137 = CARTESIAN_POINT ( 'NONE',  ( 164.9999999999999716, -272.4999999999999432, -349.9999999999999432 ) ) ;
#24138 = AXIS2_PLACEMENT_3D ( 'NONE', #17634, #30189, #7359 ) ;
#24139 = ORIENTED_EDGE ( 'NONE', *, *, #24660, .T. ) ;
#24140 = CARTESIAN_POINT ( 'NONE',  ( 151.5540265531850537, 0.000000000000000000, 82.56828755692798438 ) ) ;
#24141 = LINE ( 'NONE', #19766, #44959 ) ;
#24142 = ORIENTED_EDGE ( 'NONE', *, *, #18298, .T. ) ;
#24143 = DIRECTION ( 'NONE',  ( 1.000000000000000000, 0.000000000000000000, 0.000000000000000000 ) ) ;
#24144 = CARTESIAN_POINT ( 'NONE',  ( 73.30402655318508209, 0.000000000000000000, 165.0000000000000000 ) ) ;
#24145 = VERTEX_POINT ( 'NONE', #38976 ) ;
#24146 = EDGE_CURVE ( 'NONE', #32176, #30532, #8175, .T. ) ;
#24147 = FACE_OUTER_BOUND ( 'NONE', #45887, .T. ) ;
#24148 = CARTESIAN_POINT ( 'NONE',  ( -32.87128375420900284, -6.537745902885379046, -8.466730184410787174 ) ) ;
#24149 = FACE_OUTER_BOUND ( 'NONE', #11082, .T. ) ;
#24150 = DIRECTION ( 'NONE',  ( -1.586032892321652236E-16, 3.421138828918010427E-49, -1.000000000000000000 ) ) ;
#24151 = ORIENTED_EDGE ( 'NONE', *, *, #9273, .F. ) ;
#24152 = AXIS2_PLACEMENT_3D ( 'NONE', #44972, #37581, #37339 ) ;
#24153 = DIRECTION ( 'NONE',  ( 1.000000000000000000, 0.000000000000000000, 0.000000000000000000 ) ) ;
#24154 = CARTESIAN_POINT ( 'NONE',  ( 0.3862712429686978033, -1.188820645368937834, 10.00000000000000000 ) ) ;
#24155 = AXIS2_PLACEMENT_3D ( 'NONE', #35107, #50681, #31758 ) ;
#24156 = CARTESIAN_POINT ( 'NONE',  ( -14.49999999999999822, -46.51315789473684248, 6.315789473684215949 ) ) ;
#24157 = ORIENTED_EDGE ( 'NONE', *, *, #22593, .T. ) ;
#24158 = VECTOR ( 'NONE', #9551, 1000.000000000000000 ) ;
#24159 = EDGE_LOOP ( 'NONE', ( #49761, #41522, #8163 ) ) ;
#24160 = CARTESIAN_POINT ( 'NONE',  ( -0.3862712429686809279, -1.188820645368942941, 9.972675548442463622 ) ) ;
#24161 = DIRECTION ( 'NONE',  ( 0.000000000000000000, 0.000000000000000000, 1.000000000000000000 ) ) ;
#24162 = DIRECTION ( 'NONE',  ( 1.000000000000000000, 0.000000000000000000, -0.000000000000000000 ) ) ;
#24163 = FACE_OUTER_BOUND ( 'NONE', #15413, .T. ) ;
#24164 = CARTESIAN_POINT ( 'NONE',  ( 1.104213410210670876, 0.6509177773818231039, 9.976582533991679824 ) ) ;
#24165 = ORIENTED_EDGE ( 'NONE', *, *, #37230, .F. ) ;
#24166 = CARTESIAN_POINT ( 'NONE',  ( 135.0000000000015632, 17.00000000000000000, 35.00000000000000000 ) ) ;
#24167 = FACE_OUTER_BOUND ( 'NONE', #5548, .T. ) ;
#24168 = CARTESIAN_POINT ( 'NONE',  ( 114.3291528190321173, 1.749999999999996669, -40.20683870891911482 ) ) ;
#24169 = DIRECTION ( 'NONE',  ( -0.000000000000000000, -0.000000000000000000, -1.000000000000000000 ) ) ;
#24170 = ORIENTED_EDGE ( 'NONE', *, *, #38744, .T. ) ;
#24171 = VECTOR ( 'NONE', #37859, 1000.000000000000000 ) ;
#24172 = FACE_BOUND ( 'NONE', #12187, .T. ) ;
#24173 = ORIENTED_EDGE ( 'NONE', *, *, #45696, .T. ) ;
#24174 = CARTESIAN_POINT ( 'NONE',  ( 343.9999999999999432, -165.0000000000001137, -106.0000000000001990 ) ) ;
#24175 = VECTOR ( 'NONE', #46954, 1000.000000000000000 ) ;
#24176 = ORIENTED_EDGE ( 'NONE', *, *, #15588, .F. ) ;
#24177 = ADVANCED_FACE ( 'NONE', ( #43809 ), #13013, .T. ) ;
#24178 = CARTESIAN_POINT ( 'NONE',  ( -23.82716369509181575, -44.49195112875988656, 8.356839323120299312 ) ) ;
#24179 = CARTESIAN_POINT ( 'NONE',  ( 75.05402655318509630, 2.143131898507880377E-16, 39.06828755692795596 ) ) ;
#24180 = CARTESIAN_POINT ( 'NONE',  ( 175.0000000000000000, 0.000000000000000000, 122.5000000000000142 ) ) ;
#24181 = CARTESIAN_POINT ( 'NONE',  ( 194.3291528190321742, 1.750000000000009548, 41.84341382277508359 ) ) ;
#24182 = VERTEX_POINT ( 'NONE', #13261 ) ;
#24183 = CARTESIAN_POINT ( 'NONE',  ( -125.6708471809678542, 1.749999999999996669, -0.2068387089191042749 ) ) ;
#24184 = CARTESIAN_POINT ( 'NONE',  ( 359.9999999999998295, 183.3431457505078015, -358.3431457505079152 ) ) ;
#24185 = VERTEX_POINT ( 'NONE', #44299 ) ;
#24186 = CARTESIAN_POINT ( 'NONE',  ( -0.8282505383454070724, -1.889063466747028297, 9.894754715216727448 ) ) ;
#24187 = VECTOR ( 'NONE', #44456, 1000.000000000000000 ) ;
#24188 = DIRECTION ( 'NONE',  ( -0.000000000000000000, -0.000000000000000000, -1.000000000000000000 ) ) ;
#24189 = CARTESIAN_POINT ( 'NONE',  ( 360.0000000000000568, 169.0000000000000284, 343.9999999999998863 ) ) ;
#24190 = CARTESIAN_POINT ( 'NONE',  ( 4.999999999999999112, 175.0000000000000284, -350.0000000000002274 ) ) ;
#24191 = EDGE_LOOP ( 'NONE', ( #10269, #47960, #42692, #32203 ) ) ;
#24192 = VERTEX_POINT ( 'NONE', #40736 ) ;
#24193 = CARTESIAN_POINT ( 'NONE',  ( 210.0000000000000568, 0.000000000000000000, 42.56828755692799149 ) ) ;
#24194 = AXIS2_PLACEMENT_3D ( 'NONE', #2977, #49139, #45053 ) ;
#24195 = ORIENTED_EDGE ( 'NONE', *, *, #39990, .T. ) ;
#24196 = CARTESIAN_POINT ( 'NONE',  ( 0.8101544858819106354, 3.892041491916302220, 3.247139498068311703 ) ) ;
#24197 = DIRECTION ( 'NONE',  ( 1.000000000000000000, 0.000000000000000000, 0.000000000000000000 ) ) ;
#24198 = DIRECTION ( 'NONE',  ( -0.000000000000000000, -0.000000000000000000, -1.000000000000000000 ) ) ;
#24199 = ORIENTED_EDGE ( 'NONE', *, *, #23802, .T. ) ;
#24200 = CARTESIAN_POINT ( 'NONE',  ( -22.69295089195507487, -45.31600496604688999, 7.455576670931136185 ) ) ;
#24201 = EDGE_CURVE ( 'NONE', #26366, #46042, #9677, .T. ) ;
#24202 = CARTESIAN_POINT ( 'NONE',  ( -351.8129087874521588, 2.688010569040066411, 224.7724958161647635 ) ) ;
#24203 = LINE ( 'NONE', #39864, #49248 ) ;
#24204 = VECTOR ( 'NONE', #14559, 1000.000000000000000 ) ;
#24205 = ORIENTED_EDGE ( 'NONE', *, *, #9676, .F. ) ;
#24206 = ORIENTED_EDGE ( 'NONE', *, *, #34597, .F. ) ;
#24207 = VERTEX_POINT ( 'NONE', #36913 ) ;
#24208 = LINE ( 'NONE', #32155, #8299 ) ;
#24209 = LINE ( 'NONE', #48509, #43708 ) ;
#24210 = VECTOR ( 'NONE', #17518, 1000.000000000000000 ) ;
#24211 = PRODUCT_DEFINITION_CONTEXT ( 'detailed design', #40744, 'design' ) ;
#24212 = ORIENTED_EDGE ( 'NONE', *, *, #9505, .T. ) ;
#24213 = CARTESIAN_POINT ( 'NONE',  ( 344.0000000000000000, 167.0000000000001990, -342.0000000000002842 ) ) ;
#24214 = EDGE_LOOP ( 'NONE', ( #23295, #26528, #46555, #21547 ) ) ;
#24215 = DIRECTION ( 'NONE',  ( -1.000000000000000000, 0.000000000000000000, 0.000000000000000000 ) ) ;
#24216 = ORIENTED_EDGE ( 'NONE', *, *, #50355, .T. ) ;
#24217 = DIRECTION ( 'NONE',  ( 1.734723475976807094E-18, 0.9979060257988422444, 0.06468047367142777671 ) ) ;
#24218 = CARTESIAN_POINT ( 'NONE',  ( 80.00000000000153477, 17.00000000000000000, 60.00000000000000000 ) ) ;
#24219 = DIRECTION ( 'NONE',  ( -0.9928768384869219865, 0.000000000000000000, -0.1191452206184307749 ) ) ;
#24220 = DIRECTION ( 'NONE',  ( -0.000000000000000000, 1.000000000000000000, 6.123233995736766036E-17 ) ) ;
#24221 = CARTESIAN_POINT ( 'NONE',  ( -48.44597344681495343, 0.000000000000000000, 82.56828755692798438 ) ) ;
#24222 = CARTESIAN_POINT ( 'NONE',  ( -44.94597344681493922, 2.143131898507880377E-16, 119.0682875569279702 ) ) ;
#24223 = AXIS2_PLACEMENT_3D ( 'NONE', #23044, #8430, #7666 ) ;
#24224 = DIRECTION ( 'NONE',  ( -0.000000000000000000, -0.000000000000000000, -1.000000000000000000 ) ) ;
#24225 = ORIENTED_EDGE ( 'NONE', *, *, #5237, .T. ) ;
#24226 = ORIENTED_EDGE ( 'NONE', *, *, #15155, .T. ) ;
#24227 = DIRECTION ( 'NONE',  ( 1.000000000000000000, 0.000000000000000000, -4.625929269271687073E-16 ) ) ;
#24228 = AXIS2_PLACEMENT_3D ( 'NONE', #26225, #41870, #22362 ) ;
#24229 = CARTESIAN_POINT ( 'NONE',  ( -47.72109971266203132, -1.750000000000010214, 79.79316129108087807 ) ) ;
#24230 = CARTESIAN_POINT ( 'NONE',  ( 31.55402655318503236, 0.000000000000000000, -40.93171244307205825 ) ) ;
#24231 = AXIS2_PLACEMENT_3D ( 'NONE', #5705, #1871, #5958 ) ;
#24232 =( BOUNDED_CURVE ( )  B_SPLINE_CURVE ( 3, ( #12292, #44329, #9197, #44564 ),
 .UNSPECIFIED., .F., .F. ) 
 B_SPLINE_CURVE_WITH_KNOTS ( ( 4, 4 ),
 ( 0.000000000000000000, 1.570796326794896558 ),
 .UNSPECIFIED. ) 
 CURVE ( )  GEOMETRIC_REPRESENTATION_ITEM ( )  RATIONAL_B_SPLINE_CURVE ( ( 1.000000000000000000, 0.8047378541243649375, 0.8047378541243649375, 1.000000000000000000 ) ) 
 REPRESENTATION_ITEM ( '' )  );
#24233 = PLANE ( 'NONE',  #11773 ) ;
#24234 = DIRECTION ( 'NONE',  ( 1.000000000000000000, 0.000000000000000000, 0.000000000000000000 ) ) ;
#24235 = ORIENTED_EDGE ( 'NONE', *, *, #19752, .F. ) ;
#24236 = EDGE_CURVE ( 'NONE', #22111, #17682, #24832, .T. ) ;
#24237 = DIRECTION ( 'NONE',  ( 0.000000000000000000, -0.000000000000000000, -1.000000000000000000 ) ) ;
#24238 =( BOUNDED_CURVE ( )  B_SPLINE_CURVE ( 3, ( #17214, #17714, #49215, #1816 ),
 .UNSPECIFIED., .F., .F. ) 
 B_SPLINE_CURVE_WITH_KNOTS ( ( 4, 4 ),
 ( 4.712388980384689674, 6.283185307179586232 ),
 .UNSPECIFIED. ) 
 CURVE ( )  GEOMETRIC_REPRESENTATION_ITEM ( )  RATIONAL_B_SPLINE_CURVE ( ( 1.000000000000000000, 0.8047378541243649375, 0.8047378541243649375, 1.000000000000000000 ) ) 
 REPRESENTATION_ITEM ( '' )  );
#24239 = DIRECTION ( 'NONE',  ( 0.000000000000000000, 0.000000000000000000, -1.000000000000000000 ) ) ;
#24240 = ORIENTED_EDGE ( 'NONE', *, *, #37620, .F. ) ;
#24241 = CARTESIAN_POINT ( 'NONE',  ( 115.0540265531850395, 2.143131898507847836E-16, 82.56828755692797017 ) ) ;
#24242 = DIRECTION ( 'NONE',  ( 1.000000000000000000, 0.000000000000000000, 0.000000000000000000 ) ) ;
#24243 = CARTESIAN_POINT ( 'NONE',  ( -168.4459734468149747, 2.143131898507880377E-16, -160.9317124430720298 ) ) ;
#24244 = CARTESIAN_POINT ( 'NONE',  ( 181.0000000000000000, -164.9999999999999432, -342.0000000000001137 ) ) ;
#24245 = EDGE_CURVE ( 'NONE', #48040, #22825, #20983, .T. ) ;
#24246 = EDGE_CURVE ( 'NONE', #13764, #39166, #7768, .T. ) ;
#24247 =( BOUNDED_CURVE ( )  B_SPLINE_CURVE ( 3, ( #12759, #47359, #12254, #43550 ),
 .UNSPECIFIED., .F., .F. ) 
 B_SPLINE_CURVE_WITH_KNOTS ( ( 4, 4 ),
 ( 4.712388980384689674, 6.283185307179586232 ),
 .UNSPECIFIED. ) 
 CURVE ( )  GEOMETRIC_REPRESENTATION_ITEM ( )  RATIONAL_B_SPLINE_CURVE ( ( 1.000000000000000000, 0.8047378541243649375, 0.8047378541243649375, 1.000000000000000000 ) ) 
 REPRESENTATION_ITEM ( '' )  );
#24248 = ORIENTED_EDGE ( 'NONE', *, *, #31088, .F. ) ;
#24249 = EDGE_LOOP ( 'NONE', ( #39356, #31667, #15401, #45783, #10997, #29717 ) ) ;
#24250 = CARTESIAN_POINT ( 'NONE',  ( 155.0540265531850537, 2.143131898507890731E-16, -165.0000000000000000 ) ) ;
#24251 = CARTESIAN_POINT ( 'NONE',  ( 155.0540265531850537, 2.143131898507880377E-16, -0.9317124430720247208 ) ) ;
#24252 = EDGE_CURVE ( 'NONE', #17436, #6557, #11803, .T. ) ;
#24253 = COLOUR_RGB ( '',0.7921568627450980005, 0.8196078431372548767, 0.9333333333333333481 ) ;
#24254 = ORIENTED_EDGE ( 'NONE', *, *, #42409, .T. ) ;
#24255 = VERTEX_POINT ( 'NONE', #5060 ) ;
#24256 = DIRECTION ( 'NONE',  ( 0.000000000000000000, -1.000000000000000000, 0.000000000000000000 ) ) ;
#24257 = CARTESIAN_POINT ( 'NONE',  ( -204.9459734468148895, -1.025126265847089657, 79.06828755692797017 ) ) ;
#24258 = CARTESIAN_POINT ( 'NONE',  ( 45.21167770612395742, 22.65616271077811206, 7.906207997025717304 ) ) ;
#24259 = DIRECTION ( 'NONE',  ( 0.000000000000000000, 0.000000000000000000, 1.000000000000000000 ) ) ;
#24260 = VECTOR ( 'NONE', #14664, 1000.000000000000000 ) ;
#24261 = ORIENTED_EDGE ( 'NONE', *, *, #7871, .T. ) ;
#24262 = ORIENTED_EDGE ( 'NONE', *, *, #37894, .F. ) ;
#24263 = ORIENTED_EDGE ( 'NONE', *, *, #37948, .F. ) ;
#24264 = EDGE_CURVE ( 'NONE', #2158, #45646, #18724, .T. ) ;
#24265 = EDGE_CURVE ( 'NONE', #40248, #970, #9171, .T. ) ;
#24266 = VECTOR ( 'NONE', #9596, 1000.000000000000000 ) ;
#24267 = CARTESIAN_POINT ( 'NONE',  ( 73.30402655318508209, -1.750000000000010214, 40.81828755692798438 ) ) ;
#24268 = EDGE_CURVE ( 'NONE', #23500, #14588, #38035, .T. ) ;
#24269 = EDGE_CURVE ( 'NONE', #9972, #6508, #1488, .T. ) ;
#24270 = CYLINDRICAL_SURFACE ( 'NONE', #4961, 4.000000000000003553 ) ;
#24271 = EDGE_LOOP ( 'NONE', ( #29227, #6388, #36454, #26742 ) ) ;
#24272 = EDGE_LOOP ( 'NONE', ( #29093, #36348, #34870, #34736 ) ) ;
#24273 = CARTESIAN_POINT ( 'NONE',  ( 1.437255894074055185, -3.713052624461447682, -1.301042606982605321E-15 ) ) ;
#24274 = CARTESIAN_POINT ( 'NONE',  ( -5.888214538810513154, -16.20866436362413410, 8.727788335465566760 ) ) ;
#24275 = EDGE_CURVE ( 'NONE', #27078, #15078, #17127, .T. ) ;
#24276 = CARTESIAN_POINT ( 'NONE',  ( 29.61572577327002520, 16.11461842845735859, 8.807470649214879543 ) ) ;
#24277 = ORIENTED_EDGE ( 'NONE', *, *, #40636, .F. ) ;
#24278 = ORIENTED_EDGE ( 'NONE', *, *, #31353, .F. ) ;
#24279 = DIRECTION ( 'NONE',  ( 3.469446951953616950E-15, 0.000000000000000000, 1.000000000000000000 ) ) ;
#24280 = CARTESIAN_POINT ( 'NONE',  ( 2.499999999999945377, -224.9999999999999716, -224.9999999999999716 ) ) ;
#24281 = ORIENTED_EDGE ( 'NONE', *, *, #22677, .F. ) ;
#24282 = VECTOR ( 'NONE', #50376, 1000.000000000000000 ) ;
#24283 = CARTESIAN_POINT ( 'NONE',  ( -84.94597344681494633, 2.143131898507880377E-16, 122.5682875569279702 ) ) ;
#24284 = CARTESIAN_POINT ( 'NONE',  ( -48.44597344681495343, 0.000000000000000000, 119.0682875569279702 ) ) ;
#24285 = CARTESIAN_POINT ( 'NONE',  ( -44.94597344681493922, 2.143131898507880377E-16, 39.06828755692798438 ) ) ;
#24286 = AXIS2_PLACEMENT_3D ( 'NONE', #29540, #9539, #37519 ) ;
#24287 = CARTESIAN_POINT ( 'NONE',  ( 0.000000000000000000, 181.0000000000000284, -340.0000000000001705 ) ) ;
#24288 = AXIS2_PLACEMENT_3D ( 'NONE', #35771, #23442, #20084 ) ;
#24289 = ORIENTED_EDGE ( 'NONE', *, *, #6086, .F. ) ;
#24290 = PLANE ( 'NONE',  #11143 ) ;
#24291 = FACE_OUTER_BOUND ( 'NONE', #43282, .T. ) ;
#24292 = CARTESIAN_POINT ( 'NONE',  ( 358.0000000000001137, 180.9999999999999716, 355.9999999999997726 ) ) ;
#24293 = EDGE_CURVE ( 'NONE', #48817, #21466, #8921, .T. ) ;
#24294 = DIRECTION ( 'NONE',  ( -0.000000000000000000, -0.000000000000000000, -1.000000000000000000 ) ) ;
#24295 = VECTOR ( 'NONE', #20587, 1000.000000000000000 ) ;
#24296 = EDGE_CURVE ( 'NONE', #41468, #4473, #32545, .T. ) ;
#24297 = EDGE_CURVE ( 'NONE', #28175, #15426, #36545, .T. ) ;
#24298 = VECTOR ( 'NONE', #1553, 1000.000000000000000 ) ;
#24299 = CARTESIAN_POINT ( 'NONE',  ( 33.30402655318503946, 1.750000000000010658, 120.8182875569279702 ) ) ;
#24300 = EDGE_CURVE ( 'NONE', #3318, #9286, #11948, .T. ) ;
#24301 = CARTESIAN_POINT ( 'NONE',  ( -8.445973446814964092, -1.025126265847097651, -117.4317124430720014 ) ) ;
#24302 = DIRECTION ( 'NONE',  ( -0.000000000000000000, 0.000000000000000000, 1.000000000000000000 ) ) ;
#24303 = EDGE_CURVE ( 'NONE', #19185, #18367, #11497, .T. ) ;
#24304 = VECTOR ( 'NONE', #8794, 1000.000000000000000 ) ;
#24305 = ORIENTED_EDGE ( 'NONE', *, *, #28027, .T. ) ;
#24306 = CARTESIAN_POINT ( 'NONE',  ( 358.0000000000001137, 171.9999999999998295, 3.000000000000002665 ) ) ;
#24307 = CARTESIAN_POINT ( 'NONE',  ( -35.34822294759187145, -12.62826869953532416, -3.721387749823057423 ) ) ;
#24308 = ORIENTED_EDGE ( 'NONE', *, *, #25545, .F. ) ;
#24309 = LINE ( 'NONE', #27645, #50707 ) ;
#24310 = CARTESIAN_POINT ( 'NONE',  ( 35.51846793572394034, -35.99772139009119343, 7.906207997025717304 ) ) ;
#24311 = DIRECTION ( 'NONE',  ( 0.1346615698592613930, 0.000000000000000000, -0.9908916497796513845 ) ) ;
#24312 = ORIENTED_EDGE ( 'NONE', *, *, #38242, .T. ) ;
#24313 = CARTESIAN_POINT ( 'NONE',  ( 0.6803378293928957765, 1.026336842001439154, 9.975326647351305809 ) ) ;
#24314 = EDGE_LOOP ( 'NONE', ( #12419, #33224, #15410, #41338 ) ) ;
#24315 = ORIENTED_EDGE ( 'NONE', *, *, #3172, .T. ) ;
#24316 = CARTESIAN_POINT ( 'NONE',  ( -4.207128120815918256E-14, 3.058192377181588826E-14, 10.00000000000000000 ) ) ;
#24317 = FACE_OUTER_BOUND ( 'NONE', #544, .T. ) ;
#24318 = AXIS2_PLACEMENT_3D ( 'NONE', #39221, #28172, #7658 ) ;
#24319 = VERTEX_POINT ( 'NONE', #25086 ) ;
#24320 = CARTESIAN_POINT ( 'NONE',  ( -24.47767542868268364, 23.18653802921800278, 8.807470649214879543 ) ) ;
#24321 = DIRECTION ( 'NONE',  ( 0.000000000000000000, 0.000000000000000000, 1.000000000000000000 ) ) ;
#24322 = EDGE_CURVE ( 'NONE', #42490, #48152, #16739, .T. ) ;
#24323 = AXIS2_PLACEMENT_3D ( 'NONE', #5760, #29121, #44985 ) ;
#24324 = ORIENTED_EDGE ( 'NONE', *, *, #20181, .F. ) ;
#24325 = DIRECTION ( 'NONE',  ( -1.000000000000000000, -0.000000000000000000, -0.000000000000000000 ) ) ;
#24326 = EDGE_CURVE ( 'NONE', #20536, #27491, #34886, .T. ) ;
#24327 = ORIENTED_EDGE ( 'NONE', *, *, #14300, .T. ) ;
#24328 = CARTESIAN_POINT ( 'NONE',  ( 71.55402655318505367, 0.000000000000000000, 122.5682875569279844 ) ) ;
#24329 = LINE ( 'NONE', #13249, #18507 ) ;
#24330 = DIRECTION ( 'NONE',  ( -1.000000000000000000, 0.000000000000000000, 0.000000000000000000 ) ) ;
#24331 = ADVANCED_FACE ( 'NONE', ( #45051 ), #26595, .F. ) ;
#24332 = EDGE_LOOP ( 'NONE', ( #49977, #17468 ) ) ;
#24333 = EDGE_CURVE ( 'NONE', #39140, #2997, #22485, .T. ) ;
#24334 = CARTESIAN_POINT ( 'NONE',  ( 35.00000000000061107, 17.00000000000000000, -54.99999999999999289 ) ) ;
#24335 = LINE ( 'NONE', #11505, #44999 ) ;
#24336 = EDGE_LOOP ( 'NONE', ( #46565, #45214, #38814, #45989 ) ) ;
#24337 = ORIENTED_EDGE ( 'NONE', *, *, #6201, .F. ) ;
#24338 = ORIENTED_EDGE ( 'NONE', *, *, #32113, .F. ) ;
#24339 = CARTESIAN_POINT ( 'NONE',  ( 4.204997580903516941, 7.611558401714507482, 225.0000000000000000 ) ) ;
#24340 = EDGE_CURVE ( 'NONE', #38537, #14624, #2727, .T. ) ;
#24341 = EDGE_CURVE ( 'NONE', #11190, #6144, #17039, .T. ) ;
#24342 = DIRECTION ( 'NONE',  ( 1.000000000000000000, -3.172065799423185948E-16, 1.587271980518778491E-16 ) ) ;
#24343 = ORIENTED_EDGE ( 'NONE', *, *, #44747, .T. ) ;
#24344 = VECTOR ( 'NONE', #9470, 1000.000000000000000 ) ;
#24345 = DIRECTION ( 'NONE',  ( -3.172065784643302499E-16, -1.000000000000000000, 2.537652627714642000E-15 ) ) ;
#24346 = DIRECTION ( 'NONE',  ( 0.000000000000000000, 0.000000000000000000, 1.000000000000000000 ) ) ;
#24347 = LINE ( 'NONE', #4578, #21452 ) ;
#24348 = CARTESIAN_POINT ( 'NONE',  ( 111.5540265531850679, 0.000000000000000000, -37.43171244307205825 ) ) ;
#24349 = CARTESIAN_POINT ( 'NONE',  ( 360.0000000000000568, 165.0000000000000000, -94.00000000000019895 ) ) ;
#24350 = CARTESIAN_POINT ( 'NONE',  ( -5.000000000000000000, -165.1999999999999602, 340.1999999999997044 ) ) ;
#24351 = CARTESIAN_POINT ( 'NONE',  ( 175.0000000000000000, 15.00000000000000000, 122.5000000000000142 ) ) ;
#24352 = FACE_OUTER_BOUND ( 'NONE', #37502, .T. ) ;
#24353 = DIRECTION ( 'NONE',  ( 0.000000000000000000, -1.000000000000000000, 3.469446951953611033E-15 ) ) ;
#24354 = CARTESIAN_POINT ( 'NONE',  ( 1.320835335343329753, -0.01943189459118491516, 9.943883492372847854 ) ) ;
#24355 = PLANE ( 'NONE',  #24921 ) ;
#24356 = AXIS2_PLACEMENT_3D ( 'NONE', #1606, #10310, #24956 ) ;
#24357 = EDGE_CURVE ( 'NONE', #49308, #5026, #6337, .T. ) ;
#24358 = CARTESIAN_POINT ( 'NONE',  ( 135.0000000000003411, 16.00000000000000000, -84.99999999999998579 ) ) ;
#24359 = ORIENTED_EDGE ( 'NONE', *, *, #43147, .T. ) ;
#24360 = DIRECTION ( 'NONE',  ( 0.000000000000000000, 0.000000000000000000, -1.000000000000000000 ) ) ;
#24361 = DIRECTION ( 'NONE',  ( -0.000000000000000000, -0.000000000000000000, -1.000000000000000000 ) ) ;
#24362 = CARTESIAN_POINT ( 'NONE',  ( 210.0000000000000568, 0.000000000000000000, 2.568287556927987048 ) ) ;
#24363 = LINE ( 'NONE', #44324, #48353 ) ;
#24364 = ORIENTED_EDGE ( 'NONE', *, *, #22216, .F. ) ;
#24365 = CARTESIAN_POINT ( 'NONE',  ( -14.49999999999999822, -46.51315789473684248, -6.315789473684215949 ) ) ;
#24366 = DIRECTION ( 'NONE',  ( 0.000000000000000000, -1.000000000000000000, 0.000000000000000000 ) ) ;
#24367 = ORIENTED_EDGE ( 'NONE', *, *, #11162, .T. ) ;
#24368 = CARTESIAN_POINT ( 'NONE',  ( 85.00000000000184741, 17.00000000000000000, 90.00000000000000000 ) ) ;
#24370 = EDGE_CURVE ( 'NONE', #21159, #32283, #27239, .T. ) ;
#24369 = LINE ( 'NONE', #31570, #15942 ) ;
#24371 = LINE ( 'NONE', #759, #29281 ) ;
#24372 = VERTEX_POINT ( 'NONE', #18871 ) ;
#24373 = CARTESIAN_POINT ( 'NONE',  ( -567.5000000000000000, -72.50000000000001421, -183.5999999999997954 ) ) ;
#24374 = ORIENTED_EDGE ( 'NONE', *, *, #49096, .T. ) ;
#24375 = ORIENTED_EDGE ( 'NONE', *, *, #22101, .F. ) ;
#24376 = ORIENTED_EDGE ( 'NONE', *, *, #16002, .F. ) ;
#24377 = DIRECTION ( 'NONE',  ( 0.000000000000000000, 0.000000000000000000, -1.000000000000000000 ) ) ;
#24378 = FACE_OUTER_BOUND ( 'NONE', #2957, .T. ) ;
#24379 = EDGE_CURVE ( 'NONE', #4784, #47768, #24842, .T. ) ;
#24380 = ORIENTED_EDGE ( 'NONE', *, *, #23394, .T. ) ;
#24381 = LINE ( 'NONE', #21022, #11491 ) ;
#24382 = CARTESIAN_POINT ( 'NONE',  ( 7.499999999999996447, 194.9999999999999716, -240.0000000000000000 ) ) ;
#24383 = CARTESIAN_POINT ( 'NONE',  ( 85.00000000000123634, 16.00000000000000000, 30.00000000000000000 ) ) ;
#24384 = CARTESIAN_POINT ( 'NONE',  ( 21.23829395927641883, 7.611558401714507482, 229.0000000000000000 ) ) ;
#24385 = ORIENTED_EDGE ( 'NONE', *, *, #28846, .F. ) ;
#24386 = DIRECTION ( 'NONE',  ( 0.000000000000000000, 0.000000000000000000, -1.000000000000000000 ) ) ;
#24387 = EDGE_CURVE ( 'NONE', #17244, #34689, #49387, .T. ) ;
#24388 = ORIENTED_EDGE ( 'NONE', *, *, #27165, .F. ) ;
#24389 = EDGE_CURVE ( 'NONE', #3971, #38882, #46046, .T. ) ;
#24390 = AXIS2_PLACEMENT_3D ( 'NONE', #42732, #2981, #30972 ) ;
#24391 = LINE ( 'NONE', #8740, #15269 ) ;
#24392 = DIRECTION ( 'NONE',  ( 0.000000000000000000, 0.000000000000000000, -1.000000000000000000 ) ) ;
#24393 = ORIENTED_EDGE ( 'NONE', *, *, #34201, .F. ) ;
#24394 = CARTESIAN_POINT ( 'NONE',  ( 164.9999999999999716, 16.00000000000000000, -114.9999999999999858 ) ) ;
#24395 =( BOUNDED_CURVE ( )  B_SPLINE_CURVE ( 3, ( #5279, #16581, #676, #12467 ),
 .UNSPECIFIED., .F., .F. ) 
 B_SPLINE_CURVE_WITH_KNOTS ( ( 4, 4 ),
 ( 1.570796326794896558, 3.141592653589793116 ),
 .UNSPECIFIED. ) 
 CURVE ( )  GEOMETRIC_REPRESENTATION_ITEM ( )  RATIONAL_B_SPLINE_CURVE ( ( 1.000000000000000000, 0.8047378541243649375, 0.8047378541243649375, 1.000000000000000000 ) ) 
 REPRESENTATION_ITEM ( '' )  );
#24396 = ADVANCED_FACE ( 'NONE', ( #29431 ), #29940, .F. ) ;
#24397 = DIRECTION ( 'NONE',  ( 1.000000000000000000, 0.000000000000000000, 4.758098658057970186E-16 ) ) ;
#24398 = ORIENTED_EDGE ( 'NONE', *, *, #48979, .T. ) ;
#24399 = B_SPLINE_CURVE_WITH_KNOTS ( 'NONE', 3,
 ( #19454, #15106, #46378, #19960 ),
 .UNSPECIFIED., .F., .F.,
 ( 4, 4 ),
 ( 0.000000000000000000, 0.0001252128669263166563 ),
 .UNSPECIFIED. ) ;
#24400 = DIRECTION ( 'NONE',  ( -1.000000000000000000, -0.000000000000000000, -0.000000000000000000 ) ) ;
#24401 = EDGE_CURVE ( 'NONE', #18807, #48817, #30525, .T. ) ;
#24402 = CARTESIAN_POINT ( 'NONE',  ( -12.97493236725075683, 11.05939663307000664, 8.953103998512858652 ) ) ;
#24403 = PLANE ( 'NONE',  #1673 ) ;
#24404 = EDGE_CURVE ( 'NONE', #27650, #47604, #50097, .T. ) ;
#24405 = CARTESIAN_POINT ( 'NONE',  ( -4.945973446814917018, 1.025126265847097207, 39.06828755692796307 ) ) ;
#24406 = ORIENTED_EDGE ( 'NONE', *, *, #26827, .T. ) ;
#24407 = DIRECTION ( 'NONE',  ( 0.000000000000000000, 0.000000000000000000, 1.000000000000000000 ) ) ;
#24408 = DIRECTION ( 'NONE',  ( -0.000000000000000000, -1.000000000000000000, -0.000000000000000000 ) ) ;
#24409 = EDGE_CURVE ( 'NONE', #1177, #45648, #14019, .T. ) ;
#24410 = DIRECTION ( 'NONE',  ( 0.000000000000000000, -0.000000000000000000, -1.000000000000000000 ) ) ;
#24411 = ORIENTED_EDGE ( 'NONE', *, *, #14563, .T. ) ;
#24412 = VERTEX_POINT ( 'NONE', #45554 ) ;
#24413 = APPLICATION_PROTOCOL_DEFINITION ( 'draft international standard', 'automotive_design', 1998, #30246 ) ;
#24414 = CARTESIAN_POINT ( 'NONE',  ( 34.32915281903212446, -1.750000000000009548, -160.2068387089191219 ) ) ;
#24415 = DIRECTION ( 'NONE',  ( -1.000000000000000000, 0.000000000000000000, 0.000000000000000000 ) ) ;
#24416 = LINE ( 'NONE', #20549, #45523 ) ;
#24417 = CARTESIAN_POINT ( 'NONE',  ( -20.00000000000003197, 16.00000000000000000, -90.00000000000000000 ) ) ;
#24418 = FACE_OUTER_BOUND ( 'NONE', #40721, .T. ) ;
#24419 = ORIENTED_EDGE ( 'NONE', *, *, #16124, .T. ) ;
#24420 = DIRECTION ( 'NONE',  ( -0.000000000000000000, -0.000000000000000000, 1.000000000000000000 ) ) ;
#24421 = CARTESIAN_POINT ( 'NONE',  ( -204.9459734468149747, 0.000000000000000000, 162.5682875569279702 ) ) ;
#24422 = DIRECTION ( 'NONE',  ( -1.000000000000000000, -0.000000000000000000, -0.000000000000000000 ) ) ;
#24423 = DIRECTION ( 'NONE',  ( -0.000000000000000000, -0.000000000000000000, 1.000000000000000000 ) ) ;
#24424 = VERTEX_POINT ( 'NONE', #15313 ) ;
#24425 = LINE ( 'NONE', #8017, #33021 ) ;
#24426 = VERTEX_POINT ( 'NONE', #4510 ) ;
#24427 = CARTESIAN_POINT ( 'NONE',  ( 342.0000000000000000, 175.0000000000000284, -94.00000000000019895 ) ) ;
#24428 = ORIENTED_EDGE ( 'NONE', *, *, #30281, .T. ) ;
#24429 = DIRECTION ( 'NONE',  ( 0.000000000000000000, -0.000000000000000000, -1.000000000000000000 ) ) ;
#24430 = CARTESIAN_POINT ( 'NONE',  ( 341.9999999999999432, -182.1715728752539576, -357.1715728752541281 ) ) ;
#24431 = CARTESIAN_POINT ( 'NONE',  ( -86.69597344681494633, 1.750000000000010214, 40.81828755692798438 ) ) ;
#24432 = DIRECTION ( 'NONE',  ( -1.000000000000000000, 0.000000000000000000, 0.000000000000000000 ) ) ;
#24433 = ORIENTED_EDGE ( 'NONE', *, *, #21429, .T. ) ;
#24434 = EDGE_CURVE ( 'NONE', #46422, #50318, #46808, .T. ) ;
#24435 = CARTESIAN_POINT ( 'NONE',  ( 0.000000000000000000, -165.1999999999999602, -359.8000000000002387 ) ) ;
#24436 = CARTESIAN_POINT ( 'NONE',  ( 0.000000000000000000, 169.0000000000000000, -344.0000000000001705 ) ) ;
#24437 = VERTEX_POINT ( 'NONE', #416 ) ;
#24438 = DIRECTION ( 'NONE',  ( 0.000000000000000000, 0.000000000000000000, 1.000000000000000000 ) ) ;
#24439 = CARTESIAN_POINT ( 'NONE',  ( -124.9459734468149463, 2.143131898507847836E-16, 159.0682875569279702 ) ) ;
#24440 = CARTESIAN_POINT ( 'NONE',  ( 1.114871695981101585, -0.4953159757246433093, 9.963925895596188909 ) ) ;
#24441 = CARTESIAN_POINT ( 'NONE',  ( 356.0000000000000000, 174.9999999999996589, -342.0000000000002842 ) ) ;
#24442 = ORIENTED_EDGE ( 'NONE', *, *, #1446, .T. ) ;
#24443 = ORIENTED_EDGE ( 'NONE', *, *, #42945, .F. ) ;
#24444 = CARTESIAN_POINT ( 'NONE',  ( 194.3291528190321742, 1.750000000000009548, -158.1565861772249377 ) ) ;
#24445 = ADVANCED_FACE ( 'NONE', ( #46308 ), #38659, .T. ) ;
#24446 = ORIENTED_EDGE ( 'NONE', *, *, #3326, .F. ) ;
#24447 = B_SPLINE_CURVE_WITH_KNOTS ( 'NONE', 3,
 ( #50175, #14828, #34862, #3271 ),
 .UNSPECIFIED., .F., .F.,
 ( 4, 4 ),
 ( 0.9811748202683091558, 0.9878904167554123372 ),
 .UNSPECIFIED. ) ;
#24448 = ADVANCED_FACE ( 'NONE', ( #34821 ), #11699, .F. ) ;
#24449 = DIRECTION ( 'NONE',  ( 0.000000000000000000, 0.000000000000000000, -1.000000000000000000 ) ) ;
#24450 = CARTESIAN_POINT ( 'NONE',  ( -88.44597344681497475, 0.000000000000000000, 42.56828755692799859 ) ) ;
#24451 = PLANE ( 'NONE',  #29729 ) ;
#24452 = VERTEX_POINT ( 'NONE', #19396 ) ;
#24453 = CARTESIAN_POINT ( 'NONE',  ( -126.6959734468149321, 1.749999999999997335, -119.1817124430720440 ) ) ;
#24454 = DIRECTION ( 'NONE',  ( 6.938893903907232322E-16, -1.000000000000000000, 0.000000000000000000 ) ) ;
#24455 = CARTESIAN_POINT ( 'NONE',  ( -10.00000000000000355, -34.54492135858216528, -5.000000000000000000 ) ) ;
#24456 = EDGE_CURVE ( 'NONE', #17311, #13126, #35809, .T. ) ;
#24457 = EDGE_CURVE ( 'NONE', #4784, #41616, #43192, .T. ) ;
#24458 = CARTESIAN_POINT ( 'NONE',  ( 7.499999999999944045, -224.9999999999999716, -224.9999999999999716 ) ) ;
#24459 = ORIENTED_EDGE ( 'NONE', *, *, #21843, .F. ) ;
#24460 = VECTOR ( 'NONE', #33684, 1000.000000000000000 ) ;
#24461 = ORIENTED_EDGE ( 'NONE', *, *, #38876, .F. ) ;
#24462 = ORIENTED_EDGE ( 'NONE', *, *, #44466, .T. ) ;
#24463 = CARTESIAN_POINT ( 'NONE',  ( 14.49999999999999822, 12.98684210526315930, 19.37312575500900280 ) ) ;
#24464 = EDGE_CURVE ( 'NONE', #9708, #10975, #30966, .T. ) ;
#24465 = CARTESIAN_POINT ( 'NONE',  ( 358.0000000000000568, 182.1715728752538439, -357.1715728752539576 ) ) ;
#24466 = CARTESIAN_POINT ( 'NONE',  ( -167.4999999999999432, 47.50000000000000000, -120.5992382549688955 ) ) ;
#24467 = ORIENTED_EDGE ( 'NONE', *, *, #20959, .F. ) ;
#24468 = ORIENTED_EDGE ( 'NONE', *, *, #49905, .T. ) ;
#24469 = LINE ( 'NONE', #5209, #30781 ) ;
#24470 = ORIENTED_EDGE ( 'NONE', *, *, #37323, .F. ) ;
#24471 = LINE ( 'NONE', #1122, #40104 ) ;
#24472 = CARTESIAN_POINT ( 'NONE',  ( 154.1026953830863420, 103.0380105690400683, -17.65743994998277699 ) ) ;
#24473 = FACE_OUTER_BOUND ( 'NONE', #36511, .T. ) ;
#24474 = CARTESIAN_POINT ( 'NONE',  ( -46.69597344681494633, 1.750000000000010658, 80.81828755692798438 ) ) ;
#24475 = CARTESIAN_POINT ( 'NONE',  ( -4.376737514451251698, 37.28021197136517628, 1.982731392810406668 ) ) ;
#24476 = CARTESIAN_POINT ( 'NONE',  ( 2.961022939495062900, -16.59676755884084187, 2.590526750877053086 ) ) ;
#24477 = ORIENTED_EDGE ( 'NONE', *, *, #43990, .T. ) ;
#24478 = PLANE ( 'NONE',  #34590 ) ;
#24479 = B_SPLINE_SURFACE_WITH_KNOTS ( 'NONE', 3, 3, ( 
 ( #37810, #17531, #10084, #13912 ),
 ( #29838, #29336, #9825, #25482 ),
 ( #5979, #17785, #33451, #11093 ),
 ( #22637, #31104, #39077, #42884 ) ),
 .UNSPECIFIED., .F., .F., .F.,
 ( 4, 4 ),
 ( 4, 4 ),
 ( 0.000000000000000000, 1.000000000000000000 ),
 ( 0.000000000000000000, 1.000000000000000000 ),
 .UNSPECIFIED. ) ;
#24480 = DIRECTION ( 'NONE',  ( 0.000000000000000000, 1.000000000000000000, 0.000000000000000000 ) ) ;
#24481 = CARTESIAN_POINT ( 'NONE',  ( -0.3862712429686895876, 1.188820645368940720, -3.333333333333333481 ) ) ;
#24482 = FACE_OUTER_BOUND ( 'NONE', #38583, .T. ) ;
#24483 = ORIENTED_EDGE ( 'NONE', *, *, #38529, .F. ) ;
#24484 = DIRECTION ( 'NONE',  ( 0.000000000000000000, -1.000000000000000000, -3.186989995019654210E-49 ) ) ;
#24485 = ORIENTED_EDGE ( 'NONE', *, *, #23803, .T. ) ;
#24486 = CARTESIAN_POINT ( 'NONE',  ( -14.99999999999876366, 17.00000000000000000, 5.000000000000004441 ) ) ;
#24487 = DIRECTION ( 'NONE',  ( -1.000000000000000000, -0.000000000000000000, -0.000000000000000000 ) ) ;
#24488 = EDGE_CURVE ( 'NONE', #38490, #8840, #27103, .T. ) ;
#24489 = CIRCLE ( 'NONE', #4122, 1.749999999999987566 ) ;
#24490 = ORIENTED_EDGE ( 'NONE', *, *, #39068, .T. ) ;
#24491 = VECTOR ( 'NONE', #6299, 1000.000000000000000 ) ;
#24492 = FACE_OUTER_BOUND ( 'NONE', #23417, .T. ) ;
#24493 = CARTESIAN_POINT ( 'NONE',  ( 7.929028631756658285, -0.8360402172235281704, 8.538092108323347418E-15 ) ) ;
#24494 = CARTESIAN_POINT ( 'NONE',  ( 194.9999999999999432, -173.0000000000000000, 352.0000000000000568 ) ) ;
#24495 = CARTESIAN_POINT ( 'NONE',  ( -120.0000000000000426, 16.00000000000000000, -90.00000000000000000 ) ) ;
#24496 = ORIENTED_EDGE ( 'NONE', *, *, #20011, .T. ) ;
#24497 = ORIENTED_EDGE ( 'NONE', *, *, #45029, .T. ) ;
#24498 = CARTESIAN_POINT ( 'NONE',  ( 0.4166666666666664631, -0.000000000000000000, -10.00000000000000000 ) ) ;
#24499 = CARTESIAN_POINT ( 'NONE',  ( 49.46074318306830975, -9.578883844006833570, 8.807470649214879543 ) ) ;
#24500 = ORIENTED_EDGE ( 'NONE', *, *, #813, .F. ) ;
#24501 = ORIENTED_EDGE ( 'NONE', *, *, #27760, .T. ) ;
#24502 = CARTESIAN_POINT ( 'NONE',  ( 181.0000000000000284, -9.999999999999953815, -99.00000000000014211 ) ) ;
#24503 = CARTESIAN_POINT ( 'NONE',  ( 8.277096487746778308, -45.55573069994827051, 7.455576670931136185 ) ) ;
#24504 = CARTESIAN_POINT ( 'NONE',  ( -65.00000000000002842, 16.00000000000000000, -114.9999999999999858 ) ) ;
#24505 = FACE_OUTER_BOUND ( 'NONE', #19646, .T. ) ;
#24506 = VERTEX_POINT ( 'NONE', #30704 ) ;
#24507 = VERTEX_POINT ( 'NONE', #15804 ) ;
#24508 = ORIENTED_EDGE ( 'NONE', *, *, #833, .T. ) ;
#24509 = CARTESIAN_POINT ( 'NONE',  ( -165.0000000000000284, 16.00000000000000000, 115.0000000000000142 ) ) ;
#24510 = DIRECTION ( 'NONE',  ( 1.000000000000000000, 0.000000000000000000, 0.000000000000000000 ) ) ;
#24511 = ORIENTED_EDGE ( 'NONE', *, *, #16749, .F. ) ;
#24512 = ORIENTED_EDGE ( 'NONE', *, *, #16433, .F. ) ;
#24513 = EDGE_CURVE ( 'NONE', #37518, #5763, #39392, .T. ) ;
#24514 = CARTESIAN_POINT ( 'NONE',  ( -8.445973446814964092, -1.025126265847097651, -77.43171244307197298 ) ) ;
#24515 = CARTESIAN_POINT ( 'NONE',  ( 111.5540265531850679, 0.000000000000000000, -40.93171244307202983 ) ) ;
#24516 = ORIENTED_EDGE ( 'NONE', *, *, #39731, .F. ) ;
#24517 = ORIENTED_EDGE ( 'NONE', *, *, #36920, .F. ) ;
#24518 = CARTESIAN_POINT ( 'NONE',  ( 35.05402655318504657, -1.025126265847089657, 79.06828755692797017 ) ) ;
#24519 = CARTESIAN_POINT ( 'NONE',  ( 15.00000000000000000, 12.98684210526315752, 19.87312575500900280 ) ) ;
#24521 = VERTEX_POINT ( 'NONE', #15043 ) ;
#24520 = VECTOR ( 'NONE', #5408, 1000.000000000000000 ) ;
#24522 =( BOUNDED_CURVE ( )  B_SPLINE_CURVE ( 3, ( #45970, #14182, #3139, #33960 ),
 .UNSPECIFIED., .F., .F. ) 
 B_SPLINE_CURVE_WITH_KNOTS ( ( 4, 4 ),
 ( 1.570796326794896558, 3.141592653589793116 ),
 .UNSPECIFIED. ) 
 CURVE ( )  GEOMETRIC_REPRESENTATION_ITEM ( )  RATIONAL_B_SPLINE_CURVE ( ( 1.000000000000000000, 0.8047378541243649375, 0.8047378541243649375, 1.000000000000000000 ) ) 
 REPRESENTATION_ITEM ( '' )  );
#24523 = FACE_OUTER_BOUND ( 'NONE', #13107, .T. ) ;
#24524 = DIRECTION ( 'NONE',  ( 1.000000000000000000, 0.000000000000000000, 0.000000000000000000 ) ) ;
#24525 = CARTESIAN_POINT ( 'NONE',  ( -69.99999999999847944, 17.00000000000000000, 60.00000000000000000 ) ) ;
#24526 = AXIS2_PLACEMENT_3D ( 'NONE', #10272, #5654, #37496 ) ;
#24527 = CARTESIAN_POINT ( 'NONE',  ( -86.69597344681494633, 1.750000000000010658, -119.1817124430720440 ) ) ;
#24528 = AXIS2_PLACEMENT_3D ( 'NONE', #11845, #31614, #47200 ) ;
#24529 = EDGE_LOOP ( 'NONE', ( #186, #28016, #9845, #34454 ) ) ;
#24530 = AXIS2_PLACEMENT_3D ( 'NONE', #32851, #48432, #13319 ) ;
#24531 = CARTESIAN_POINT ( 'NONE',  ( 177.5000000000000284, -112.5000000000000000, -10.00000000000000000 ) ) ;
#24532 =( BOUNDED_CURVE ( )  B_SPLINE_CURVE ( 3, ( #4166, #39577, #43398, #35744 ),
 .UNSPECIFIED., .F., .F. ) 
 B_SPLINE_CURVE_WITH_KNOTS ( ( 4, 4 ),
 ( 3.141592653589793116, 4.712388980384689674 ),
 .UNSPECIFIED. ) 
 CURVE ( )  GEOMETRIC_REPRESENTATION_ITEM ( )  RATIONAL_B_SPLINE_CURVE ( ( 1.000000000000000000, 0.8047378541243649375, 0.8047378541243649375, 1.000000000000000000 ) ) 
 REPRESENTATION_ITEM ( '' )  );
#24533 = CARTESIAN_POINT ( 'NONE',  ( 30.87089393895375267, -12.69923079256617449, -9.367992836599954742 ) ) ;
#24534 = CARTESIAN_POINT ( 'NONE',  ( -164.9459734468149463, 1.025126265847089879, -117.4317124430720156 ) ) ;
#24535 = CARTESIAN_POINT ( 'NONE',  ( -6.695973446814940111, 1.750000000000023315, 0.8182875569279768335 ) ) ;
#24536 = AXIS2_PLACEMENT_3D ( 'NONE', #29893, #50540, #26305 ) ;
#24537 = DIRECTION ( 'NONE',  ( -0.000000000000000000, -0.000000000000000000, -1.000000000000000000 ) ) ;
#24539 = DIRECTION ( 'NONE',  ( 0.000000000000000000, 1.000000000000000000, 0.000000000000000000 ) ) ;
#24538 =( BOUNDED_CURVE ( )  B_SPLINE_CURVE ( 3, ( #20656, #17060, #24514, #28866 ),
 .UNSPECIFIED., .F., .F. ) 
 B_SPLINE_CURVE_WITH_KNOTS ( ( 4, 4 ),
 ( 1.570796326794896558, 3.141592653589793116 ),
 .UNSPECIFIED. ) 
 CURVE ( )  GEOMETRIC_REPRESENTATION_ITEM ( )  RATIONAL_B_SPLINE_CURVE ( ( 1.000000000000000000, 0.8047378541243649375, 0.8047378541243649375, 1.000000000000000000 ) ) 
 REPRESENTATION_ITEM ( '' )  );
#24540 = DIRECTION ( 'NONE',  ( -0.000000000000000000, -0.000000000000000000, -1.000000000000000000 ) ) ;
#24541 = ORIENTED_EDGE ( 'NONE', *, *, #39646, .F. ) ;
#24542 = CARTESIAN_POINT ( 'NONE',  ( 71.55402655318506788, 2.143131898507880377E-16, -160.9317124430720298 ) ) ;
#24543 = FACE_OUTER_BOUND ( 'NONE', #2646, .T. ) ;
#24544 = EDGE_LOOP ( 'NONE', ( #15040, #37398, #13671, #18520, #7331 ) ) ;
#24545 = DIRECTION ( 'NONE',  ( 0.000000000000000000, 0.000000000000000000, 1.000000000000000000 ) ) ;
#24546 = CARTESIAN_POINT ( 'NONE',  ( -128.4459734468149179, 0.000000000000000000, -40.93171244307202983 ) ) ;
#24547 = CARTESIAN_POINT ( 'NONE',  ( -29.38926261462371770, 40.45084971874734237, 0.000000000000000000 ) ) ;
#24548 = ORIENTED_EDGE ( 'NONE', *, *, #48422, .T. ) ;
#24549 = CARTESIAN_POINT ( 'NONE',  ( 15.00000000000000000, -46.12433806312137108, 6.404467680894761372 ) ) ;
#24550 = ORIENTED_EDGE ( 'NONE', *, *, #41794, .F. ) ;
#24552 = ORIENTED_EDGE ( 'NONE', *, *, #19485, .F. ) ;
#24551 = VECTOR ( 'NONE', #40826, 1000.000000000000000 ) ;
#24553 = CARTESIAN_POINT ( 'NONE',  ( -194.9999999999999432, -173.0000000000000000, 352.0000000000000568 ) ) ;
#24554 = FACE_OUTER_BOUND ( 'NONE', #38099, .T. ) ;
#24555 = AXIS2_PLACEMENT_3D ( 'NONE', #36943, #1760, #37187 ) ;
#24556 = VECTOR ( 'NONE', #44320, 1000.000000000000000 ) ;
#24557 = ORIENTED_EDGE ( 'NONE', *, *, #46642, .F. ) ;
#24558 = CARTESIAN_POINT ( 'NONE',  ( 193.3040265531851105, 0.000000000000000000, -165.0000000000000000 ) ) ;
#24559 = CARTESIAN_POINT ( 'NONE',  ( -168.4459734468149747, -1.025126265847089213, -0.9317124430720324924 ) ) ;
#24560 = EDGE_LOOP ( 'NONE', ( #33276, #29752, #25514, #24315 ) ) ;
#24561 = ORIENTED_EDGE ( 'NONE', *, *, #24692, .T. ) ;
#24562 = VECTOR ( 'NONE', #34176, 1000.000000000000000 ) ;
#24563 = DIRECTION ( 'NONE',  ( -1.000000000000000000, 0.000000000000000000, 0.000000000000000000 ) ) ;
#24564 = VERTEX_POINT ( 'NONE', #3746 ) ;
#24565 = CARTESIAN_POINT ( 'NONE',  ( 192.2789002873380184, -1.750000000000010214, 121.8434138227750623 ) ) ;
#24566 = LINE ( 'NONE', #16872, #6176 ) ;
#24567 = DIRECTION ( 'NONE',  ( -0.000000000000000000, -0.000000000000000000, -1.000000000000000000 ) ) ;
#24568 = ORIENTED_EDGE ( 'NONE', *, *, #40872, .T. ) ;
#24569 = EDGE_CURVE ( 'NONE', #47251, #38939, #46552, .T. ) ;
#24570 = CARTESIAN_POINT ( 'NONE',  ( -1.249999999999999778, 0.000000000000000000, 10.00000000000000000 ) ) ;
#24571 = CARTESIAN_POINT ( 'NONE',  ( 0.3370904143228981575, -0.2449105217885261532, 10.00000000000000000 ) ) ;
#24572 = ORIENTED_EDGE ( 'NONE', *, *, #5895, .F. ) ;
#24573 = ORIENTED_EDGE ( 'NONE', *, *, #9132, .F. ) ;
#24574 = EDGE_LOOP ( 'NONE', ( #44027, #14819, #26272, #4753, #3978, #10714 ) ) ;
#24575 = DIRECTION ( 'NONE',  ( 0.000000000000000000, 0.000000000000000000, 1.000000000000000000 ) ) ;
#24576 = EDGE_CURVE ( 'NONE', #25177, #9422, #8114, .T. ) ;
#24577 = DIRECTION ( 'NONE',  ( -1.000000000000000000, 0.000000000000000000, 0.000000000000000000 ) ) ;
#24578 = ORIENTED_EDGE ( 'NONE', *, *, #592, .T. ) ;
#24579 = EDGE_CURVE ( 'NONE', #46782, #35640, #38917, .T. ) ;
#24580 = DIRECTION ( 'NONE',  ( -1.000000000000000000, -0.000000000000000000, -0.000000000000000000 ) ) ;
#24581 = CARTESIAN_POINT ( 'NONE',  ( 71.55402655318505367, 0.000000000000000000, 165.0000000000000000 ) ) ;
#24582 = LINE ( 'NONE', #25777, #15785 ) ;
#24583 = EDGE_CURVE ( 'NONE', #5629, #40397, #165, .T. ) ;
#24584 = CARTESIAN_POINT ( 'NONE',  ( -0.3896797354171960270, 1.262193838292709147, 9.943883492372847854 ) ) ;
#24585 = CARTESIAN_POINT ( 'NONE',  ( -84.94597344681497475, 0.000000000000000000, 162.5682875569279702 ) ) ;
#24586 = DIRECTION ( 'NONE',  ( 0.000000000000000000, 0.000000000000000000, -1.000000000000000000 ) ) ;
#24587 = CARTESIAN_POINT ( 'NONE',  ( -48.44597344681496054, -1.025126265847089213, -0.9317124430720324924 ) ) ;
#24588 = DIRECTION ( 'NONE',  ( 0.000000000000000000, 0.000000000000000000, -1.000000000000000000 ) ) ;
#24589 = CARTESIAN_POINT ( 'NONE',  ( -19.99999999999908695, 16.00000000000000000, -24.99999999999999289 ) ) ;
#24590 = DIRECTION ( 'NONE',  ( 0.000000000000000000, -1.000000000000000000, 0.000000000000000000 ) ) ;
#24591 = AXIS2_PLACEMENT_3D ( 'NONE', #37950, #10719, #38959 ) ;
#24592 = CIRCLE ( 'NONE', #22133, 2.000000000000001776 ) ;
#24593 = DIRECTION ( 'NONE',  ( -0.000000000000000000, -1.000000000000000000, -0.000000000000000000 ) ) ;
#24594 = UNCERTAINTY_MEASURE_WITH_UNIT (LENGTH_MEASURE( 1.000000000000000082E-05 ), #8368, 'distance_accuracy_value', 'NONE');
#24595 = AXIS2_PLACEMENT_3D ( 'NONE', #19362, #35045, #24237 ) ;
#24596 = LINE ( 'NONE', #24358, #34747 ) ;
#24597 = EDGE_LOOP ( 'NONE', ( #21173, #28657, #45630, #38257, #47623, #11616 ) ) ;
#24598 = VECTOR ( 'NONE', #5059, 1000.000000000000000 ) ;
#24599 = CARTESIAN_POINT ( 'NONE',  ( -543.5050241616419271, 53.53801056904005407, -176.2397770772458898 ) ) ;
#24600 = VECTOR ( 'NONE', #43566, 1000.000000000000000 ) ;
#24601 = DIRECTION ( 'NONE',  ( 0.000000000000000000, 1.000000000000000000, 0.000000000000000000 ) ) ;
#24602 = CARTESIAN_POINT ( 'NONE',  ( -310.0878471510133068, 232.7719218785459816, 296.3011729072028402 ) ) ;
#24603 = ADVANCED_FACE ( 'NONE', ( #31464 ), #47061, .T. ) ;
#24604 = EDGE_CURVE ( 'NONE', #8293, #43828, #27620, .T. ) ;
#24605 = CARTESIAN_POINT ( 'NONE',  ( 85.00000000000184741, 16.00000000000000000, 65.00000000000000000 ) ) ;
#24606 = AXIS2_PLACEMENT_3D ( 'NONE', #12554, #32586, #35934 ) ;
#24608 = VERTEX_POINT ( 'NONE', #924 ) ;
#24607 = ADVANCED_FACE ( 'NONE', ( #4261 ), #43500, .T. ) ;
#24609 = DIRECTION ( 'NONE',  ( -0.000000000000000000, -0.000000000000000000, -1.000000000000000000 ) ) ;
#24610 = ADVANCED_FACE ( 'NONE', ( #36082 ), #16311, .T. ) ;
#24611 = CARTESIAN_POINT ( 'NONE',  ( 344.0000000000000568, 165.0000000000000000, 339.9999999999998295 ) ) ;
#24612 = ORIENTED_EDGE ( 'NONE', *, *, #5533, .F. ) ;
#24613 = ADVANCED_FACE ( 'NONE', ( #32482 ), #5513, .T. ) ;
#24614 = DIRECTION ( 'NONE',  ( 0.000000000000000000, 0.000000000000000000, -1.000000000000000000 ) ) ;
#24615 = CYLINDRICAL_SURFACE ( 'NONE', #29776, 2.000000000000001776 ) ;
#24616 = CARTESIAN_POINT ( 'NONE',  ( -128.4459734468149463, 1.025126265847081442, 159.0682875569279418 ) ) ;
#24617 = EDGE_CURVE ( 'NONE', #37708, #38609, #5941, .T. ) ;
#24618 = VERTEX_POINT ( 'NONE', #48319 ) ;
#24619 = CARTESIAN_POINT ( 'NONE',  ( 350.0000000000000000, -182.9999999999999716, -344.0000000000001705 ) ) ;
#24620 = ORIENTED_EDGE ( 'NONE', *, *, #18086, .T. ) ;
#24621 = ORIENTED_EDGE ( 'NONE', *, *, #5599, .F. ) ;
#24622 = ORIENTED_EDGE ( 'NONE', *, *, #27365, .T. ) ;
#24623 = FACE_OUTER_BOUND ( 'NONE', #13038, .T. ) ;
#24624 = CARTESIAN_POINT ( 'NONE',  ( 74.32915281903215998, 1.750000000000010214, -80.20683870891910772 ) ) ;
#24625 = ORIENTED_EDGE ( 'NONE', *, *, #9375, .T. ) ;
#24626 = LINE ( 'NONE', #12305, #4135 ) ;
#24627 = CARTESIAN_POINT ( 'NONE',  ( -6.174150299305392053, 50.00000000000000711, 8.807470649214879543 ) ) ;
#24628 = PLANE ( 'NONE',  #16586 ) ;
#24629 = CARTESIAN_POINT ( 'NONE',  ( 0.3370904143228947158, 0.2449105217885311492, -10.00000000000000000 ) ) ;
#24630 = ADVANCED_FACE ( 'NONE', ( #40170 ), #8859, .T. ) ;
#24631 = ORIENTED_EDGE ( 'NONE', *, *, #8308, .T. ) ;
#24632 = EDGE_CURVE ( 'NONE', #14100, #3211, #13461, .T. ) ;
#24633 = DIRECTION ( 'NONE',  ( -1.000000000000000000, 0.000000000000000000, -7.793956916774525800E-48 ) ) ;
#24634 = VECTOR ( 'NONE', #47729, 1000.000000000000000 ) ;
#24635 = EDGE_CURVE ( 'NONE', #21159, #35861, #42952, .T. ) ;
#24636 = VERTEX_POINT ( 'NONE', #48571 ) ;
#24637 = ADVANCED_FACE ( 'NONE', ( #5005 ), #3510, .T. ) ;
#24638 = DIRECTION ( 'NONE',  ( 0.000000000000000000, -0.3846153846153844702, 0.9230769230769231282 ) ) ;
#24639 = DIRECTION ( 'NONE',  ( 0.000000000000000000, 0.000000000000000000, 1.000000000000000000 ) ) ;
#24640 = VERTEX_POINT ( 'NONE', #40425 ) ;
#24641 = CARTESIAN_POINT ( 'NONE',  ( -49.75871208702130133, -40.58472229863598102, 5.000000000000000000 ) ) ;
#24642 = VECTOR ( 'NONE', #45882, 1000.000000000000000 ) ;
#24643 = AXIS2_PLACEMENT_3D ( 'NONE', #11833, #46432, #34687 ) ;
#24644 = DIRECTION ( 'NONE',  ( 0.000000000000000000, -5.664403186863042467E-17, -1.000000000000000000 ) ) ;
#24645 = ORIENTED_EDGE ( 'NONE', *, *, #5314, .F. ) ;
#24647 = EDGE_CURVE ( 'NONE', #13851, #17745, #43748, .T. ) ;
#24646 = CARTESIAN_POINT ( 'NONE',  ( -16.69947034530963847, 2.312583065866374632, 2.590526750877053086 ) ) ;
#24648 = CARTESIAN_POINT ( 'NONE',  ( 0.000000000000000000, 0.000000000000000000, 10.00000000000000000 ) ) ;
#24649 = CARTESIAN_POINT ( 'NONE',  ( 153.3040265531850537, 1.750000000000009992, -159.1817124430720298 ) ) ;
#24650 = CARTESIAN_POINT ( 'NONE',  ( 151.5540265531850537, 0.000000000000000000, -165.0000000000000000 ) ) ;
#24651 = ORIENTED_EDGE ( 'NONE', *, *, #20390, .T. ) ;
#24652 = CARTESIAN_POINT ( 'NONE',  ( 7.499999999999996447, 194.9999999999999716, -224.9999999999999716 ) ) ;
#24653 = CARTESIAN_POINT ( 'NONE',  ( 30.00000000000217781, 17.00000000000000000, 95.00000000000000000 ) ) ;
#24654 = EDGE_CURVE ( 'NONE', #41260, #29654, #5260, .T. ) ;
#24655 = CARTESIAN_POINT ( 'NONE',  ( -36.08557433729205144, 35.58569447144795816, 7.455576670931136185 ) ) ;
#24656 = VERTEX_POINT ( 'NONE', #36599 ) ;
#24657 = EDGE_LOOP ( 'NONE', ( #45354, #6008, #24058, #2582 ) ) ;
#24658 = SHAPE_DEFINITION_REPRESENTATION ( #10572, #31369 ) ;
#24659 = CYLINDRICAL_SURFACE ( 'NONE', #2893, 1.750000000000008438 ) ;
#24660 = EDGE_CURVE ( 'NONE', #30282, #26345, #40677, .T. ) ;
#24661 = CARTESIAN_POINT ( 'NONE',  ( -88.44597344681494633, -1.025126265847089657, -80.93171244307201562 ) ) ;
#24662 = CARTESIAN_POINT ( 'NONE',  ( -5.000000000000000000, 165.2000000000000171, 359.7999999999997840 ) ) ;
#24663 = ORIENTED_EDGE ( 'NONE', *, *, #36311, .F. ) ;
#24664 = DIRECTION ( 'NONE',  ( 6.203854594147707562E-25, -2.067951531382569187E-25, 1.000000000000000000 ) ) ;
#24665 = CARTESIAN_POINT ( 'NONE',  ( 360.0000000000000000, -169.0000000000001137, -344.0000000000003411 ) ) ;
#24666 = CARTESIAN_POINT ( 'NONE',  ( -46.69597344681494633, 0.000000000000000000, -165.0000000000000000 ) ) ;
#24667 = CIRCLE ( 'NONE', #43514, 20.99999999999999289 ) ;
#24669 = VERTEX_POINT ( 'NONE', #6516 ) ;
#24668 = EDGE_CURVE ( 'NONE', #45714, #16313, #21161, .T. ) ;
#24670 = AXIS2_PLACEMENT_3D ( 'NONE', #10465, #34086, #26105 ) ;
#24671 = CARTESIAN_POINT ( 'NONE',  ( -46.69597344681494633, -1.750000000000009992, 0.8182875569279768335 ) ) ;
#24672 = EDGE_CURVE ( 'NONE', #25002, #22721, #29369, .T. ) ;
#24673 = VERTEX_POINT ( 'NONE', #49070 ) ;
#24674 = DIRECTION ( 'NONE',  ( -0.000000000000000000, 2.406552799042969348E-16, 1.000000000000000000 ) ) ;
#24675 = EDGE_LOOP ( 'NONE', ( #30163, #16665, #45460, #44654 ) ) ;
#24676 = CARTESIAN_POINT ( 'NONE',  ( 210.0000000000000568, 0.000000000000000000, -159.1817124430720298 ) ) ;
#24677 = CARTESIAN_POINT ( 'NONE',  ( -70.00000000000002842, 17.00000000000000000, -114.9999999999999858 ) ) ;
#24678 = EDGE_CURVE ( 'NONE', #38516, #47604, #41614, .T. ) ;
#24679 = VECTOR ( 'NONE', #11985, 1000.000000000000114 ) ;
#24680 = CARTESIAN_POINT ( 'NONE',  ( -206.6959734468149463, 1.750000000000009992, -159.1817124430720298 ) ) ;
#24681 = CARTESIAN_POINT ( 'NONE',  ( -4.945973446814903696, 2.143131898507912917E-16, -157.4317124430720014 ) ) ;
#24682 = ORIENTED_EDGE ( 'NONE', *, *, #25208, .T. ) ;
#24683 = EDGE_CURVE ( 'NONE', #23180, #18208, #44986, .T. ) ;
#24684 = EDGE_CURVE ( 'NONE', #11965, #34539, #6549, .T. ) ;
#24685 = PLANE ( 'NONE',  #9759 ) ;
#24686 = ORIENTED_EDGE ( 'NONE', *, *, #17858, .T. ) ;
#24687 = CARTESIAN_POINT ( 'NONE',  ( 151.5540265531850537, 2.143131898507880377E-16, -160.9317124430720298 ) ) ;
#24688 = CARTESIAN_POINT ( 'NONE',  ( -124.9459734468149321, 1.025126265847081664, 159.0682875569279418 ) ) ;
#24689 = CARTESIAN_POINT ( 'NONE',  ( -6.695973446814940111, -1.750000000000023315, -159.1817124430720298 ) ) ;
#24690 = CARTESIAN_POINT ( 'NONE',  ( -1.540571744149449751, 1.371626741452969034, 9.889206917020301191 ) ) ;
#24691 = CARTESIAN_POINT ( 'NONE',  ( -0.3862712429686977478, 1.188820645368937390, -10.00000000000000000 ) ) ;
#24692 = EDGE_CURVE ( 'NONE', #44183, #18077, #43262, .T. ) ;
#24693 =( BOUNDED_CURVE ( )  B_SPLINE_CURVE ( 3, ( #30215, #19684, #39201, #23268 ),
 .UNSPECIFIED., .F., .F. ) 
 B_SPLINE_CURVE_WITH_KNOTS ( ( 4, 4 ),
 ( 1.570796326794896558, 3.141592653589793116 ),
 .UNSPECIFIED. ) 
 CURVE ( )  GEOMETRIC_REPRESENTATION_ITEM ( )  RATIONAL_B_SPLINE_CURVE ( ( 1.000000000000000000, 0.8047378541243649375, 0.8047378541243649375, 1.000000000000000000 ) ) 
 REPRESENTATION_ITEM ( '' )  );
#24694 = VERTEX_POINT ( 'NONE', #41422 ) ;
#24695 = EDGE_LOOP ( 'NONE', ( #35086, #34720, #3, #10474 ) ) ;
#24696 = LINE ( 'NONE', #40591, #24304 ) ;
#24697 = B_SPLINE_CURVE_WITH_KNOTS ( 'NONE', 3,
 ( #5126, #30181, #22484, #29679 ),
 .UNSPECIFIED., .F., .F.,
 ( 4, 4 ),
 ( 0.9811748202683103770, 0.9878904167554123372 ),
 .UNSPECIFIED. ) ;
#24698 = ORIENTED_EDGE ( 'NONE', *, *, #1846, .F. ) ;
#24699 = EDGE_CURVE ( 'NONE', #6202, #22032, #26281, .T. ) ;
#24700 = CARTESIAN_POINT ( 'NONE',  ( 0.3910393408562611861, 3.877122853646846945, 9.741991644046958498 ) ) ;
#24701 = CARTESIAN_POINT ( 'NONE',  ( 169.0000000000000284, 165.0000000000000000, 357.9999999999998863 ) ) ;
#24702 = CARTESIAN_POINT ( 'NONE',  ( 34.32915281903212446, -1.750000000000010436, -120.2068387089191219 ) ) ;
#24703 = ORIENTED_EDGE ( 'NONE', *, *, #21424, .F. ) ;
#24704 = CARTESIAN_POINT ( 'NONE',  ( -124.9459734468149463, 2.143131898507847836E-16, -77.43171244307204404 ) ) ;
#24705 = CARTESIAN_POINT ( 'NONE',  ( 0.000000000000000000, -180.9999999999999716, -356.0000000000002274 ) ) ;
#24706 = CARTESIAN_POINT ( 'NONE',  ( 1.249999999999999778, -0.000000000000000000, -3.333333333333333481 ) ) ;
#24707 = CARTESIAN_POINT ( 'NONE',  ( 0.3862712429686810944, 1.188820645368943607, -3.333333333333333481 ) ) ;
#24708 = VECTOR ( 'NONE', #34222, 1000.000000000000114 ) ;
#24709 = CARTESIAN_POINT ( 'NONE',  ( -114.9999999999978542, 17.00000000000000000, 95.00000000000000000 ) ) ;
#24710 = DIRECTION ( 'NONE',  ( 6.203854594147707562E-25, -2.067951531382569187E-25, 1.000000000000000000 ) ) ;
#24711 = VERTEX_POINT ( 'NONE', #21664 ) ;
#24712 = VERTEX_POINT ( 'NONE', #2904 ) ;
#24713 = ORIENTED_EDGE ( 'NONE', *, *, #44379, .F. ) ;
#24714 = CARTESIAN_POINT ( 'NONE',  ( -4.207128120815918256E-14, 3.058192377181588826E-14, 10.00000000000000000 ) ) ;
#24715 = DIRECTION ( 'NONE',  ( -0.000000000000000000, -0.000000000000000000, -1.000000000000000000 ) ) ;
#24716 = VECTOR ( 'NONE', #25853, 1000.000000000000000 ) ;
#24717 = CARTESIAN_POINT ( 'NONE',  ( 0.000000000000000000, 23.48684210526316107, -3.750000000000000000 ) ) ;
#24718 = CYLINDRICAL_SURFACE ( 'NONE', #23965, 2.000000000000001776 ) ;
#24719 = VECTOR ( 'NONE', #2385, 1000.000000000000000 ) ;
#24720 = ORIENTED_EDGE ( 'NONE', *, *, #5582, .T. ) ;
#24721 = DIRECTION ( 'NONE',  ( 1.000000000000000000, 0.000000000000000000, 2.958228394578794708E-31 ) ) ;
#24722 = ORIENTED_EDGE ( 'NONE', *, *, #49891, .T. ) ;
#24723 = CARTESIAN_POINT ( 'NONE',  ( -6.875132362119187768, 50.00000000000000711, 8.356839323120299312 ) ) ;
#24724 = DIRECTION ( 'NONE',  ( 0.000000000000000000, 0.000000000000000000, -1.000000000000000000 ) ) ;
#24725 = CARTESIAN_POINT ( 'NONE',  ( 164.9999999999999716, -164.9999999999999432, 343.9999999999998863 ) ) ;
#24726 = DIRECTION ( 'NONE',  ( -1.000000000000000000, 0.000000000000000000, 0.000000000000000000 ) ) ;
#24727 = CARTESIAN_POINT ( 'NONE',  ( 166.9999999999999716, -168.9999999999999432, -340.0000000000001137 ) ) ;
#24728 = CARTESIAN_POINT ( 'NONE',  ( 340.0000000000000568, 167.0000000000000000, 355.9999999999997726 ) ) ;
#24729 = ORIENTED_EDGE ( 'NONE', *, *, #46847, .T. ) ;
#24730 = CARTESIAN_POINT ( 'NONE',  ( 135.0000000000000000, 16.00000000000000000, -90.00000000000000000 ) ) ;
#24731 = CARTESIAN_POINT ( 'NONE',  ( -9.281355226777547429, 3.722424633806451943, 0.000000000000000000 ) ) ;
#24732 = CARTESIAN_POINT ( 'NONE',  ( 181.0000000000000568, 165.0000000000000000, 355.9999999999998863 ) ) ;
#24733 = EDGE_CURVE ( 'NONE', #6508, #541, #11784, .T. ) ;
#24734 = FACE_OUTER_BOUND ( 'NONE', #48046, .T. ) ;
#24735 = EDGE_CURVE ( 'NONE', #7866, #40121, #40464, .T. ) ;
#24736 = ORIENTED_EDGE ( 'NONE', *, *, #22781, .T. ) ;
#24737 = CARTESIAN_POINT ( 'NONE',  ( -5.000000000000000000, -165.1999999999999602, -359.8000000000002387 ) ) ;
#24738 = EDGE_LOOP ( 'NONE', ( #8247, #23451, #10707, #28401 ) ) ;
#24739 = CARTESIAN_POINT ( 'NONE',  ( 1.780432407520001536, 1.041450996408479046, 9.894754715216729224 ) ) ;
#24740 = VECTOR ( 'NONE', #17601, 1000.000000000000000 ) ;
#24741 = CARTESIAN_POINT ( 'NONE',  ( 115.0540265531850395, 1.025126265847082108, 122.5682875569279702 ) ) ;
#24742 = EDGE_CURVE ( 'NONE', #9083, #20951, #14205, .T. ) ;
#24743 = B_SPLINE_CURVE_WITH_KNOTS ( 'NONE', 3,
 ( #32363, #47961, #32879, #33131 ),
 .UNSPECIFIED., .F., .F.,
 ( 4, 4 ),
 ( 0.000000000000000000, 0.2562577668812811016 ),
 .UNSPECIFIED. ) ;
#24744 = CARTESIAN_POINT ( 'NONE',  ( -5.873104089934114924, -0.6060605173725300832, 9.586754400234157814 ) ) ;
#24745 = VERTEX_POINT ( 'NONE', #33241 ) ;
#24746 = ADVANCED_FACE ( 'NONE', ( #21926 ), #38093, .F. ) ;
#24747 = EDGE_CURVE ( 'NONE', #12693, #16975, #2177, .T. ) ;
#24748 = ORIENTED_EDGE ( 'NONE', *, *, #2457, .T. ) ;
#24749 = AXIS2_PLACEMENT_3D ( 'NONE', #18826, #11154, #26801 ) ;
#24750 = LINE ( 'NONE', #20122, #14763 ) ;
#24751 = CARTESIAN_POINT ( 'NONE',  ( -208.4459734468149463, 0.000000000000000000, 42.56828755692798438 ) ) ;
#24752 = CARTESIAN_POINT ( 'NONE',  ( 168.9999999999999716, -174.9999999999999716, -340.0000000000001137 ) ) ;
#24753 = LINE ( 'NONE', #4235, #8675 ) ;
#24754 = EDGE_CURVE ( 'NONE', #17122, #46071, #2417, .T. ) ;
#24755 = VERTEX_POINT ( 'NONE', #37847 ) ;
#24756 = ORIENTED_EDGE ( 'NONE', *, *, #32958, .T. ) ;
#24757 = CARTESIAN_POINT ( 'NONE',  ( -0.3905129037392560676, 2.126717070043232738, 9.885585981620938156 ) ) ;
#24758 = CARTESIAN_POINT ( 'NONE',  ( 154.3291528190321458, -1.750000000000009548, -0.2068387089191121020 ) ) ;
#24759 = VERTEX_POINT ( 'NONE', #49818 ) ;
#24760 = VERTEX_POINT ( 'NONE', #45988 ) ;
#24761 = CARTESIAN_POINT ( 'NONE',  ( 29.18392875402930997, 17.44843138996603216, 7.906207997025717304 ) ) ;
#24762 = CARTESIAN_POINT ( 'NONE',  ( 0.6721397084974982672, 9.977385840602783773, 2.154851817814940063E-15 ) ) ;
#24763 = LINE ( 'NONE', #35560, #5429 ) ;
#24764 = CARTESIAN_POINT ( 'NONE',  ( 360.0000000000001137, 181.0000000000000568, 355.9999999999998863 ) ) ;
#24765 = ORIENTED_EDGE ( 'NONE', *, *, #34641, .T. ) ;
#24766 = EDGE_LOOP ( 'NONE', ( #46573, #2604, #32933, #21225 ) ) ;
#24767 = EDGE_LOOP ( 'NONE', ( #46817, #29021, #9406, #13871 ) ) ;
#24768 = CARTESIAN_POINT ( 'NONE',  ( -207.2103713177049258, 159.2880105690400399, 472.6625600500171345 ) ) ;
#24769 = CARTESIAN_POINT ( 'NONE',  ( 1.011271242968683648, 0.7347315653655930312, -10.00000000000000000 ) ) ;
#24770 = VERTEX_POINT ( 'NONE', #2665 ) ;
#24771 =( BOUNDED_CURVE ( )  B_SPLINE_CURVE ( 3, ( #21567, #25425, #5916, #37259 ),
 .UNSPECIFIED., .F., .F. ) 
 B_SPLINE_CURVE_WITH_KNOTS ( ( 4, 4 ),
 ( 8.635508522760760582E-16, 1.570796326794897002 ),
 .UNSPECIFIED. ) 
 CURVE ( )  GEOMETRIC_REPRESENTATION_ITEM ( )  RATIONAL_B_SPLINE_CURVE ( ( 1.000000000000000000, 0.8047378541243650485, 0.8047378541243650485, 1.000000000000000000 ) ) 
 REPRESENTATION_ITEM ( '' )  );
#24772 = VECTOR ( 'NONE', #13265, 1000.000000000000000 ) ;
#24773 = ORIENTED_EDGE ( 'NONE', *, *, #7349, .T. ) ;
#24774 = CARTESIAN_POINT ( 'NONE',  ( 359.9999999999999432, 166.6568542494923975, -341.6568542494925396 ) ) ;
#24775 = VECTOR ( 'NONE', #9552, 1000.000000000000000 ) ;
#24776 = CARTESIAN_POINT ( 'NONE',  ( 28.96803024440893992, 18.11533787072037072, 7.455576670931136185 ) ) ;
#24777 = EDGE_LOOP ( 'NONE', ( #33784, #43547, #18853, #42879, #17164, #42716 ) ) ;
#24778 = ORIENTED_EDGE ( 'NONE', *, *, #6602, .T. ) ;
#24780 = ADVANCED_FACE ( 'NONE', ( #18305 ), #39626, .T. ) ;
#24779 = AXIS2_PLACEMENT_3D ( 'NONE', #36040, #28069, #8578 ) ;
#24781 = CARTESIAN_POINT ( 'NONE',  ( -50.11058929355264979, 7.578863168071929834, 7.455576670931136185 ) ) ;
#24782 = CARTESIAN_POINT ( 'NONE',  ( -30.65355587399070814, 13.36566953343609043, -8.917361510505369182 ) ) ;
#24783 = ORIENTED_EDGE ( 'NONE', *, *, #13429, .T. ) ;
#24784 = DIRECTION ( 'NONE',  ( -1.000000000000000000, 0.000000000000000000, 0.000000000000000000 ) ) ;
#24785 = DIRECTION ( 'NONE',  ( -1.000000000000000000, 0.000000000000000000, -0.000000000000000000 ) ) ;
#24786 = DIRECTION ( 'NONE',  ( 0.000000000000000000, -3.186989995019654210E-49, -1.000000000000000000 ) ) ;
#24787 = AXIS2_PLACEMENT_3D ( 'NONE', #17679, #5112, #8978 ) ;
#24788 = DIRECTION ( 'NONE',  ( 1.000000000000000000, 0.000000000000000000, -0.000000000000000000 ) ) ;
#24789 = EDGE_LOOP ( 'NONE', ( #40621, #35161, #44984, #19423 ) ) ;
#24790 = LINE ( 'NONE', #44760, #18490 ) ;
#24791 = CARTESIAN_POINT ( 'NONE',  ( 31.94178169330218964, -9.256608784833820991, -3.760136334089591248 ) ) ;
#24792 = FACE_OUTER_BOUND ( 'NONE', #36449, .T. ) ;
#24793 = CARTESIAN_POINT ( 'NONE',  ( 359.9999999999998863, -183.3431457505077731, -358.3431457505079152 ) ) ;
#24794 = DIRECTION ( 'NONE',  ( -0.000000000000000000, -1.000000000000000000, 2.537652627714643577E-15 ) ) ;
#24795 = CARTESIAN_POINT ( 'NONE',  ( -1.401094519807299710, 0.7138523880601858052, 9.927288994922816912 ) ) ;
#24796 = DIRECTION ( 'NONE',  ( -0.6904757466825007794, -0.7233555441435719491, 0.000000000000000000 ) ) ;
#24797 = DIRECTION ( 'NONE',  ( 0.000000000000000000, 0.000000000000000000, 1.000000000000000000 ) ) ;
#24798 = ORIENTED_EDGE ( 'NONE', *, *, #37324, .T. ) ;
#24799 = CARTESIAN_POINT ( 'NONE',  ( -23.26005729352344176, -44.90397804740339183, 7.906207997025717304 ) ) ;
#24800 = ORIENTED_EDGE ( 'NONE', *, *, #45749, .F. ) ;
#24801 = CARTESIAN_POINT ( 'NONE',  ( -4.339432828817248122, -37.24807810779213213, -8.192531242611266862 ) ) ;
#24802 = EDGE_CURVE ( 'NONE', #46959, #29991, #1321, .T. ) ;
#24803 = CARTESIAN_POINT ( 'NONE',  ( 1.424818880982069880, -0.8247269902869861502, 9.936700280135882579 ) ) ;
#24804 = CARTESIAN_POINT ( 'NONE',  ( 33.30402655318503946, -1.750000000000009992, 0.8182875569279768335 ) ) ;
#24805 = AXIS2_PLACEMENT_3D ( 'NONE', #28249, #799, #24410 ) ;
#24806 = ORIENTED_EDGE ( 'NONE', *, *, #31640, .T. ) ;
#24807 = DIRECTION ( 'NONE',  ( 0.000000000000000000, 0.000000000000000000, -1.000000000000000000 ) ) ;
#24808 = ORIENTED_EDGE ( 'NONE', *, *, #16276, .F. ) ;
#24809 = LINE ( 'NONE', #2213, #39029 ) ;
#24810 = AXIS2_PLACEMENT_3D ( 'NONE', #49479, #14372, #30039 ) ;
#24811 = DIRECTION ( 'NONE',  ( 0.000000000000000000, -1.000000000000000000, -3.186989995019654210E-49 ) ) ;
#24812 = ORIENTED_EDGE ( 'NONE', *, *, #23017, .F. ) ;
#24813 = AXIS2_PLACEMENT_3D ( 'NONE', #11595, #46190, #22878 ) ;
#24814 = CARTESIAN_POINT ( 'NONE',  ( 2.053349722363697616, -0.3420258690444287208, 9.888808121373919846 ) ) ;
#24815 = CARTESIAN_POINT ( 'NONE',  ( 341.9999999999999432, -169.0000000000001137, -344.0000000000002842 ) ) ;
#24816 = ORIENTED_EDGE ( 'NONE', *, *, #18593, .T. ) ;
#24817 = ORIENTED_EDGE ( 'NONE', *, *, #17139, .F. ) ;
#24818 = CARTESIAN_POINT ( 'NONE',  ( 1.697332391510682159, 0.8495613812374117613, 9.900811091504543526 ) ) ;
#24819 = ORIENTED_EDGE ( 'NONE', *, *, #37750, .T. ) ;
#24820 = CARTESIAN_POINT ( 'NONE',  ( -2.961022939495062900, 16.59676755884084187, 2.590526750877053086 ) ) ;
#24821 = CARTESIAN_POINT ( 'NONE',  ( -114.9999999999987779, 17.00000000000000000, 30.00000000000000000 ) ) ;
#24822 = CARTESIAN_POINT ( 'NONE',  ( -22.69295089195507487, -45.31600496604688999, 7.455576670931136185 ) ) ;
#24823 =( BOUNDED_CURVE ( )  B_SPLINE_CURVE ( 3, ( #27766, #24181, #23912, #35745 ),
 .UNSPECIFIED., .F., .F. ) 
 B_SPLINE_CURVE_WITH_KNOTS ( ( 4, 4 ),
 ( 1.570796326794896558, 3.141592653589793116 ),
 .UNSPECIFIED. ) 
 CURVE ( )  GEOMETRIC_REPRESENTATION_ITEM ( )  RATIONAL_B_SPLINE_CURVE ( ( 1.000000000000000000, 0.8047378541243649375, 0.8047378541243649375, 1.000000000000000000 ) ) 
 REPRESENTATION_ITEM ( '' )  );
#24824 = ORIENTED_EDGE ( 'NONE', *, *, #28787, .T. ) ;
#24825 = DIRECTION ( 'NONE',  ( 0.000000000000000000, 1.580451535867971417E-48, -1.000000000000000000 ) ) ;
#24826 = CARTESIAN_POINT ( 'NONE',  ( 6.508636631827673824, 15.75743548351451295, 8.953103998512858652 ) ) ;
#24827 = ORIENTED_EDGE ( 'NONE', *, *, #32185, .T. ) ;
#24828 = ORIENTED_EDGE ( 'NONE', *, *, #24859, .T. ) ;
#24829 = ORIENTED_EDGE ( 'NONE', *, *, #8964, .F. ) ;
#24830 = FACE_OUTER_BOUND ( 'NONE', #49426, .T. ) ;
#24831 =( BOUNDED_CURVE ( )  B_SPLINE_CURVE ( 3, ( #39196, #29152, #48851, #44513 ),
 .UNSPECIFIED., .F., .F. ) 
 B_SPLINE_CURVE_WITH_KNOTS ( ( 4, 4 ),
 ( 3.141592653589793116, 4.712388980384689674 ),
 .UNSPECIFIED. ) 
 CURVE ( )  GEOMETRIC_REPRESENTATION_ITEM ( )  RATIONAL_B_SPLINE_CURVE ( ( 1.000000000000000000, 0.8047378541243649375, 0.8047378541243649375, 1.000000000000000000 ) ) 
 REPRESENTATION_ITEM ( '' )  );
#24832 = LINE ( 'NONE', #12771, #29119 ) ;
#24833 = EDGE_LOOP ( 'NONE', ( #43539, #50547, #50151, #37720 ) ) ;
#24834 = EDGE_CURVE ( 'NONE', #47416, #30683, #4200, .T. ) ;
#24835 = LINE ( 'NONE', #17377, #3661 ) ;
#24836 = DIRECTION ( 'NONE',  ( -1.000000000000000000, -0.000000000000000000, -0.000000000000000000 ) ) ;
#24837 = CARTESIAN_POINT ( 'NONE',  ( -10.25676241992221449, 8.638513918217338272, -18.89424093979656760 ) ) ;
#24838 = CARTESIAN_POINT ( 'NONE',  ( 350.0000000000001137, 175.0000000000000000, 349.9999999999998295 ) ) ;
#24839 = DIRECTION ( 'NONE',  ( -0.000000000000000000, -0.000000000000000000, -1.000000000000000000 ) ) ;
#24840 = CARTESIAN_POINT ( 'NONE',  ( 50.00000000000000000, 6.123233995736766085E-15, 900.0000000000000000 ) ) ;
#24841 = DIRECTION ( 'NONE',  ( 0.000000000000000000, 0.000000000000000000, 1.000000000000000000 ) ) ;
#24842 = B_SPLINE_CURVE_WITH_KNOTS ( 'NONE', 3,
 ( #26344, #38161, #21723, #18373 ),
 .UNSPECIFIED., .F., .F.,
 ( 4, 4 ),
 ( 0.8097120833243712790, 0.9322955464061803976 ),
 .UNSPECIFIED. ) ;
#24843 = CARTESIAN_POINT ( 'NONE',  ( -64.99999999999940314, 16.00000000000000000, -54.99999999999999289 ) ) ;
#24844 = CARTESIAN_POINT ( 'NONE',  ( 0.9987333403011454669, 1.123935354443737600, 9.936141075511214282 ) ) ;
#24845 = CARTESIAN_POINT ( 'NONE',  ( -8.445973446814976526, 0.000000000000000000, 165.0000000000000000 ) ) ;
#24846=STYLED_ITEM('',(#50747),#38969);
#24847 = FACE_OUTER_BOUND ( 'NONE', #5685, .T. ) ;
#24848 = FACE_BOUND ( 'NONE', #49054, .T. ) ;
#24849 = EDGE_LOOP ( 'NONE', ( #10435, #29522, #46723, #37567 ) ) ;
#24850 = CARTESIAN_POINT ( 'NONE',  ( 26.25702031264353664, -26.77347351953840615, 8.914903342594564961 ) ) ;
#24851 = CARTESIAN_POINT ( 'NONE',  ( 168.9999999999999716, -166.9999999999999432, -115.0000000000001847 ) ) ;
#24852 = CARTESIAN_POINT ( 'NONE',  ( -167.7210997126620384, -1.750000000000009548, 1.843413822775065825 ) ) ;
#24853 = LINE ( 'NONE', #12795, #13959 ) ;
#24854 = ORIENTED_EDGE ( 'NONE', *, *, #14286, .F. ) ;
#24855 = DIRECTION ( 'NONE',  ( 0.000000000000000000, -1.000000000000000000, 0.000000000000000000 ) ) ;
#24856 = LINE ( 'NONE', #32060, #36892 ) ;
#24857 = ORIENTED_EDGE ( 'NONE', *, *, #14289, .F. ) ;
#24858 = CARTESIAN_POINT ( 'NONE',  ( -165.0000000000000284, 17.00000000000000000, -90.00000000000000000 ) ) ;
#24859 = EDGE_CURVE ( 'NONE', #8676, #20584, #13440, .T. ) ;
#24860 = CARTESIAN_POINT ( 'NONE',  ( 3.087186397306452612, 2.514307945609885131, -2.642742795433417058E-16 ) ) ;
#24861 = CARTESIAN_POINT ( 'NONE',  ( -69.99999999999909051, 17.00000000000000000, -24.99999999999999289 ) ) ;
#24862 = ORIENTED_EDGE ( 'NONE', *, *, #38287, .T. ) ;
#24863 = CARTESIAN_POINT ( 'NONE',  ( 31.55402655318503236, -1.025126265847089879, -117.4317124430720156 ) ) ;
#24864 = VERTEX_POINT ( 'NONE', #26788 ) ;
#24865 = ORIENTED_EDGE ( 'NONE', *, *, #25889, .F. ) ;
#24866 = VERTEX_POINT ( 'NONE', #8059 ) ;
#24867 = FACE_OUTER_BOUND ( 'NONE', #8342, .T. ) ;
#24868 = LINE ( 'NONE', #40773, #39638 ) ;
#24869 = VECTOR ( 'NONE', #19233, 1000.000000000000000 ) ;
#24870 = VERTEX_POINT ( 'NONE', #50071 ) ;
#24871 = CARTESIAN_POINT ( 'NONE',  ( 350.0000000000001137, 175.0000000000000284, 349.9999999999998295 ) ) ;
#24872 = CARTESIAN_POINT ( 'NONE',  ( 210.0000000000000568, 2.143131898507881856E-16, 119.0682875569279560 ) ) ;
#24873 = VECTOR ( 'NONE', #13602, 1000.000000000000000 ) ;
#24874 = EDGE_CURVE ( 'NONE', #42829, #38545, #19070, .T. ) ;
#24875 = CARTESIAN_POINT ( 'NONE',  ( 355.9999999999999432, -183.0000000000001421, -349.9999999999998863 ) ) ;
#24876 = ADVANCED_FACE ( 'NONE', ( #47256 ), #50332, .T. ) ;
#24877 = FACE_BOUND ( 'NONE', #36984, .T. ) ;
#24878 = VERTEX_POINT ( 'NONE', #19834 ) ;
#24879 = MECHANICAL_DESIGN_GEOMETRIC_PRESENTATION_REPRESENTATION (  '', ( #24084 ), #9310 ) ;
#24880 = DIRECTION ( 'NONE',  ( -1.000000000000000000, 0.000000000000000000, 0.000000000000000000 ) ) ;
#24881 = EDGE_CURVE ( 'NONE', #50273, #43723, #24100, .T. ) ;
#24882 = EDGE_LOOP ( 'NONE', ( #10242, #10100, #984, #26658 ) ) ;
#24883 = PRESENTATION_LAYER_ASSIGNMENT (  '', '', ( #46960 ) ) ;
#24884 = DIRECTION ( 'NONE',  ( 1.000000000000000000, 0.000000000000000000, 0.000000000000000000 ) ) ;
#24885 = DIRECTION ( 'NONE',  ( -0.000000000000000000, -1.000000000000000000, -0.000000000000000000 ) ) ;
#24886 = ORIENTED_EDGE ( 'NONE', *, *, #45267, .T. ) ;
#24887 = ORIENTED_EDGE ( 'NONE', *, *, #34638, .T. ) ;
#24888 = EDGE_LOOP ( 'NONE', ( #15640, #42397, #32032, #13753 ) ) ;
#24889 = CARTESIAN_POINT ( 'NONE',  ( -1.365263087672800246, 0.5437404457009007430, 9.958264684458713489 ) ) ;
#24890 = FACE_OUTER_BOUND ( 'NONE', #32416, .T. ) ;
#24891 = PRODUCT_DEFINITION_SHAPE ( 'NONE', 'NONE',  #44709 ) ;
#24892 = EDGE_CURVE ( 'NONE', #1975, #17667, #3681, .T. ) ;
#24893 = EDGE_LOOP ( 'NONE', ( #7829, #4487, #44338, #47801 ) ) ;
#24894 = ADVANCED_FACE ( 'NONE', ( #34494 ), #39114, .T. ) ;
#24895 = CARTESIAN_POINT ( 'NONE',  ( 168.9999999999999716, 175.0000000000000284, -340.0000000000001137 ) ) ;
#24896 = LINE ( 'NONE', #48442, #18190 ) ;
#24897 = EDGE_CURVE ( 'NONE', #17906, #25205, #20458, .T. ) ;
#24898 = EDGE_CURVE ( 'NONE', #19313, #48360, #33392, .T. ) ;
#24899 = ORIENTED_EDGE ( 'NONE', *, *, #11182, .F. ) ;
#24900 = DIRECTION ( 'NONE',  ( -0.000000000000000000, -0.000000000000000000, -1.000000000000000000 ) ) ;
#24901 = DIRECTION ( 'NONE',  ( 1.000000000000000000, 0.000000000000000000, 0.000000000000000000 ) ) ;
#24902 = EDGE_CURVE ( 'NONE', #8001, #36506, #35020, .T. ) ;
#24904 = B_SPLINE_CURVE_WITH_KNOTS ( 'NONE', 3,
 ( #36938, #12536, #36683, #4600, #13282, #747 ),
 .UNSPECIFIED., .F., .F.,
 ( 4, 2, 4 ),
 ( 5.818439421673296370E-18, 0.009877169331704830149, 0.01975433866340965683 ),
 .UNSPECIFIED. ) ;
#24903 = CARTESIAN_POINT ( 'NONE',  ( 18.38319608353691947, -32.68498281710168385, -8.192531242611265085 ) ) ;
#24905 = ORIENTED_EDGE ( 'NONE', *, *, #49279, .T. ) ;
#24906 = VERTEX_POINT ( 'NONE', #46743 ) ;
#24907 = APPLICATION_PROTOCOL_DEFINITION ( 'draft international standard', 'automotive_design', 1998, #39776 ) ;
#24908 = CARTESIAN_POINT ( 'NONE',  ( -164.9999999999984936, 17.00000000000000000, 60.00000000000000000 ) ) ;
#24909 = LINE ( 'NONE', #20546, #5366 ) ;
#24910 = VECTOR ( 'NONE', #7648, 1000.000000000000000 ) ;
#24911 = CARTESIAN_POINT ( 'NONE',  ( -14.99999999999937472, 17.00000000000000000, -54.99999999999999289 ) ) ;
#24912 = CARTESIAN_POINT ( 'NONE',  ( 0.3862712429686810944, 1.188820645368943607, -10.00000000000000000 ) ) ;
#24913 = ORIENTED_EDGE ( 'NONE', *, *, #49509, .F. ) ;
#24914 = CARTESIAN_POINT ( 'NONE',  ( -165.0000000000000284, 15.00000000000000000, -114.9999999999999858 ) ) ;
#24915 = CIRCLE ( 'NONE', #37208, 10.00000000000000000 ) ;
#24916 = CARTESIAN_POINT ( 'NONE',  ( 0.3862712429686894766, -1.188820645368940276, -3.333333333333333481 ) ) ;
#24917 = CARTESIAN_POINT ( 'NONE',  ( 224.9999999999999432, -175.0000000000000000, 500.0000000000000000 ) ) ;
#24918 = EDGE_CURVE ( 'NONE', #24759, #26029, #11645, .T. ) ;
#24919 = VECTOR ( 'NONE', #4782, 1000.000000000000000 ) ;
#24920 = CARTESIAN_POINT ( 'NONE',  ( -9.643172164747307207, 0.000000000000000000, 0.000000000000000000 ) ) ;
#24921 = AXIS2_PLACEMENT_3D ( 'NONE', #13027, #43317, #40245 ) ;
#24922 = ORIENTED_EDGE ( 'NONE', *, *, #3172, .F. ) ;
#24923 = EDGE_CURVE ( 'NONE', #45889, #34658, #27838, .T. ) ;
#24924 = DIRECTION ( 'NONE',  ( 1.132880637372608740E-16, 4.718402560806925739E-50, 1.000000000000000000 ) ) ;
#24925 = ORIENTED_EDGE ( 'NONE', *, *, #4243, .F. ) ;
#24926 = EDGE_CURVE ( 'NONE', #43437, #46782, #7806, .T. ) ;
#24927 = CARTESIAN_POINT ( 'NONE',  ( -208.4459734468149463, 0.000000000000000000, -37.43171244307205825 ) ) ;
#24928 = ORIENTED_EDGE ( 'NONE', *, *, #5008, .T. ) ;
#24929 = CARTESIAN_POINT ( 'NONE',  ( 84.99999999999997158, 17.00000000000000000, -114.9999999999999858 ) ) ;
#24930 = ADVANCED_FACE ( 'NONE', ( #40116 ), #17260, .F. ) ;
#24931 = CARTESIAN_POINT ( 'NONE',  ( -206.6959734468149463, -1.750000000000009992, -159.1817124430720298 ) ) ;
#24932 = DIRECTION ( 'NONE',  ( -1.000000000000000000, 0.000000000000000000, -2.958228394578794270E-31 ) ) ;
#24933 = ORIENTED_EDGE ( 'NONE', *, *, #37119, .F. ) ;
#24934 = EDGE_CURVE ( 'NONE', #33254, #40248, #8811, .T. ) ;
#24935 = VECTOR ( 'NONE', #29061, 1000.000000000000000 ) ;
#24936 = CARTESIAN_POINT ( 'NONE',  ( -7.721099712662037540, 1.750000000000023315, 39.79316129108089228 ) ) ;
#24937 = ORIENTED_EDGE ( 'NONE', *, *, #2640, .F. ) ;
#24938 = LINE ( 'NONE', #44403, #27856 ) ;
#24939 = CARTESIAN_POINT ( 'NONE',  ( 185.0000000000000284, -81.49999999999988631, -115.0000000000001563 ) ) ;
#24940 = DIRECTION ( 'NONE',  ( -0.000000000000000000, -0.000000000000000000, -1.000000000000000000 ) ) ;
#24941 = DIRECTION ( 'NONE',  ( -0.000000000000000000, -0.000000000000000000, -1.000000000000000000 ) ) ;
#24942 = FACE_BOUND ( 'NONE', #45143, .T. ) ;
#24943 = ORIENTED_EDGE ( 'NONE', *, *, #39405, .T. ) ;
#24944 = VERTEX_POINT ( 'NONE', #24717 ) ;
#24945 = PLANE ( 'NONE',  #8737 ) ;
#24946 = ORIENTED_EDGE ( 'NONE', *, *, #36517, .T. ) ;
#24947 = CARTESIAN_POINT ( 'NONE',  ( -6.880036658038867436, 222.4999999999999716, -228.6347188485896140 ) ) ;
#24948 = VECTOR ( 'NONE', #3727, 1000.000000000000000 ) ;
#24949 = DIRECTION ( 'NONE',  ( -1.000000000000000000, -0.000000000000000000, -0.000000000000000000 ) ) ;
#24950 = ADVANCED_FACE ( 'NONE', ( #4942 ), #1370, .F. ) ;
#24951 = ORIENTED_EDGE ( 'NONE', *, *, #3692, .F. ) ;
#24952 = CYLINDRICAL_SURFACE ( 'NONE', #43410, 1.750000000000008438 ) ;
#24953 = VECTOR ( 'NONE', #34459, 1000.000000000000114 ) ;
#24954 = FACE_BOUND ( 'NONE', #9122, .T. ) ;
#24955 = VERTEX_POINT ( 'NONE', #20093 ) ;
#24956 = DIRECTION ( 'NONE',  ( 0.000000000000000000, -1.000000000000000000, 0.000000000000000000 ) ) ;
#24957 = CARTESIAN_POINT ( 'NONE',  ( -124.9459734468149321, 1.025126265847081886, -40.93171244307202272 ) ) ;
#24958 = CARTESIAN_POINT ( 'NONE',  ( 9.999999999999998224, 1.843143693225357538E-15, 8.340239149798797769 ) ) ;
#24959 = DIRECTION ( 'NONE',  ( 0.000000000000000000, -0.2223603367690689669, 0.9749645535258942841 ) ) ;
#24960 = EDGE_CURVE ( 'NONE', #22117, #21998, #24209, .T. ) ;
#24962 = ORIENTED_EDGE ( 'NONE', *, *, #42525, .T. ) ;
#24961 = EDGE_CURVE ( 'NONE', #43962, #7928, #24968, .T. ) ;
#24963 = VERTEX_POINT ( 'NONE', #12391 ) ;
#24964 = ORIENTED_EDGE ( 'NONE', *, *, #30859, .T. ) ;
#24965 = CARTESIAN_POINT ( 'NONE',  ( -166.6959734468149463, -1.750000000000010658, -119.1817124430720440 ) ) ;
#24966 = ADVANCED_FACE ( 'NONE', ( #4450 ), #8309, .T. ) ;
#24967 = CARTESIAN_POINT ( 'NONE',  ( -0.3862712429686729343, -1.188820645368946050, -3.333333333333333481 ) ) ;
#24968 = LINE ( 'NONE', #35783, #4418 ) ;
#24969 = ADVANCED_FACE ( 'NONE', ( #36531 ), #20598, .T. ) ;
#24970 = DIRECTION ( 'NONE',  ( 0.000000000000000000, -0.9230769230769231282, 0.3846153846153845812 ) ) ;
#24971 = ORIENTED_EDGE ( 'NONE', *, *, #18884, .F. ) ;
#24972 = EDGE_CURVE ( 'NONE', #36062, #23873, #2116, .T. ) ;
#24973 = DIRECTION ( 'NONE',  ( 1.000000000000000000, 0.000000000000000000, -1.860490536778032451E-50 ) ) ;
#24974 = ORIENTED_EDGE ( 'NONE', *, *, #1369, .T. ) ;
#24975 = CARTESIAN_POINT ( 'NONE',  ( -8.277096487746778308, 50.00000000000000711, 7.455576670931136185 ) ) ;
#24976 = CARTESIAN_POINT ( 'NONE',  ( -164.4973046169135102, 103.1142457376053727, -17.29493270523947501 ) ) ;
#24977 = DIRECTION ( 'NONE',  ( 0.000000000000000000, 0.000000000000000000, 1.000000000000000000 ) ) ;
#24978 = VECTOR ( 'NONE', #41875, 1000.000000000000000 ) ;
#24979 = LINE ( 'NONE', #44195, #45484 ) ;
#24980 = CARTESIAN_POINT ( 'NONE',  ( 341.9999999999999432, -181.0000000000001421, -356.0000000000003411 ) ) ;
#24981 = AXIS2_PLACEMENT_3D ( 'NONE', #44504, #28624, #10134 ) ;
#24982 = DIRECTION ( 'NONE',  ( -1.000000000000000000, -0.000000000000000000, -0.000000000000000000 ) ) ;
#24983 = VERTEX_POINT ( 'NONE', #24466 ) ;
#24984 = DIRECTION ( 'NONE',  ( -1.000000000000000000, 0.000000000000000000, 0.000000000000000000 ) ) ;
#24985 = CARTESIAN_POINT ( 'NONE',  ( -46.75893035013464072, -17.89420872045582200, 3.199614146704519602 ) ) ;
#24986 = CARTESIAN_POINT ( 'NONE',  ( -14.99999999999937472, 17.00000000000000000, -30.00000000000000000 ) ) ;
#24987 = EDGE_LOOP ( 'NONE', ( #29526, #9247, #20128, #11719, #37579, #33596 ) ) ;
#24988 = EDGE_CURVE ( 'NONE', #10222, #2212, #16251, .T. ) ;
#24989 = VECTOR ( 'NONE', #5745, 1000.000000000000000 ) ;
#24990 = FACE_BOUND ( 'NONE', #31776, .T. ) ;
#24991 = VERTEX_POINT ( 'NONE', #28049 ) ;
#24992 = CARTESIAN_POINT ( 'NONE',  ( 111.5540265531850679, 0.000000000000000000, 159.0682875569279702 ) ) ;
#24993 = CARTESIAN_POINT ( 'NONE',  ( -556.7900739183570522, -61.66198943095990614, -65.53102910462104091 ) ) ;
#24994 =( BOUNDED_CURVE ( )  B_SPLINE_CURVE ( 3, ( #50431, #43020, #23544, #38199 ),
 .UNSPECIFIED., .F., .F. ) 
 B_SPLINE_CURVE_WITH_KNOTS ( ( 4, 4 ),
 ( 4.712388980384689674, 6.283185307179586232 ),
 .UNSPECIFIED. ) 
 CURVE ( )  GEOMETRIC_REPRESENTATION_ITEM ( )  RATIONAL_B_SPLINE_CURVE ( ( 1.000000000000000000, 0.8047378541243649375, 0.8047378541243649375, 1.000000000000000000 ) ) 
 REPRESENTATION_ITEM ( '' )  );
#24995 = CARTESIAN_POINT ( 'NONE',  ( 191.5540265531851105, 0.000000000000000000, 2.568287556927978166 ) ) ;
#24996 = AXIS2_PLACEMENT_3D ( 'NONE', #30255, #33864, #49949 ) ;
#24997 = VERTEX_POINT ( 'NONE', #9061 ) ;
#24998 = LINE ( 'NONE', #36812, #43443 ) ;
#24999 = CARTESIAN_POINT ( 'NONE',  ( -15.57957361750255565, -5.755602074545403291, 3.266473740018926541 ) ) ;
#25000 = CARTESIAN_POINT ( 'NONE',  ( -208.4459734468149463, 0.000000000000000000, 165.0000000000000000 ) ) ;
#25001 = EDGE_CURVE ( 'NONE', #21151, #12850, #48463, .T. ) ;
#25002 = VERTEX_POINT ( 'NONE', #20850 ) ;
#25003 = ORIENTED_EDGE ( 'NONE', *, *, #242, .T. ) ;
#25004 = DIRECTION ( 'NONE',  ( 0.000000000000000000, 0.000000000000000000, -1.000000000000000000 ) ) ;
#25005 = CARTESIAN_POINT ( 'NONE',  ( 30.12518629743562926, 14.70074613238908157, 1.847720168420772691 ) ) ;
#25006 = AXIS2_PLACEMENT_3D ( 'NONE', #9705, #29975, #48909 ) ;
#25007 = VERTEX_POINT ( 'NONE', #44187 ) ;
#25008 = ORIENTED_EDGE ( 'NONE', *, *, #47216, .F. ) ;
#25009 = CARTESIAN_POINT ( 'NONE',  ( 14.52758583651987223, 8.922352469211173087, 8.953103998512858652 ) ) ;
#25010 = CARTESIAN_POINT ( 'NONE',  ( 1.455748852897596812, 0.01196569884528948975, 9.938560165450791573 ) ) ;
#25011 = CARTESIAN_POINT ( 'NONE',  ( 35.05402655318504657, -1.025126265847089435, -77.43171244307200141 ) ) ;
#25012 = CARTESIAN_POINT ( 'NONE',  ( -119.9999999999981668, 16.00000000000000000, 65.00000000000000000 ) ) ;
#25013 = ORIENTED_EDGE ( 'NONE', *, *, #46143, .T. ) ;
#25014 = AXIS2_PLACEMENT_3D ( 'NONE', #33941, #49530, #18523 ) ;
#25015 = ORIENTED_EDGE ( 'NONE', *, *, #7489, .T. ) ;
#25016 = ORIENTED_EDGE ( 'NONE', *, *, #31517, .F. ) ;
#25017 = CARTESIAN_POINT ( 'NONE',  ( 135.0000000000003411, 16.00000000000000000, -84.99999999999998579 ) ) ;
#25019=STYLED_ITEM('',(#50747),#22244);
#25018 = LINE ( 'NONE', #29365, #21641 ) ;
#25020 = EDGE_CURVE ( 'NONE', #11492, #26100, #20346, .T. ) ;
#25021 = EDGE_CURVE ( 'NONE', #48417, #20358, #36022, .T. ) ;
#25022 = VERTEX_POINT ( 'NONE', #12895 ) ;
#25023 = VECTOR ( 'NONE', #5320, 1000.000000000000000 ) ;
#25024 = EDGE_LOOP ( 'NONE', ( #48745, #22276, #20081, #50119, #12602 ) ) ;
#25025 = CARTESIAN_POINT ( 'NONE',  ( -164.9459734468149463, -1.025126265847089213, -0.9317124430720324924 ) ) ;
#25026 = CARTESIAN_POINT ( 'NONE',  ( 113.3040265531850537, 1.749999999999997113, -39.18171244307202983 ) ) ;
#25027 = EDGE_CURVE ( 'NONE', #27082, #35344, #28811, .T. ) ;
#25028 = ORIENTED_EDGE ( 'NONE', *, *, #27794, .F. ) ;
#25029 = VERTEX_POINT ( 'NONE', #9307 ) ;
#25030 = VECTOR ( 'NONE', #20603, 1000.000000000000000 ) ;
#25031 = ADVANCED_FACE ( 'NONE', ( #40615 ), #42308, .F. ) ;
#25032 = CARTESIAN_POINT ( 'NONE',  ( 34.32915281903212446, -1.750000000000010436, 79.79316129108087807 ) ) ;
#25033 = CARTESIAN_POINT ( 'NONE',  ( -15.15373036401909346, 7.214190911381058058, -9.233365092205394475 ) ) ;
#25034 = ORIENTED_EDGE ( 'NONE', *, *, #11131, .F. ) ;
#25035 = ADVANCED_FACE ( 'NONE', ( #1867 ), #50467, .F. ) ;
#25036 = CARTESIAN_POINT ( 'NONE',  ( 85.00000000000184741, 16.00000000000000000, 90.00000000000000000 ) ) ;
#25037 = DIRECTION ( 'NONE',  ( -1.000000000000000000, 0.000000000000000000, -0.000000000000000000 ) ) ;
#25038 = LINE ( 'NONE', #44994, #6349 ) ;
#25039 = FACE_OUTER_BOUND ( 'NONE', #1266, .T. ) ;
#25040 = LINE ( 'NONE', #17324, #371 ) ;
#25041 = ORIENTED_EDGE ( 'NONE', *, *, #19909, .F. ) ;
#25042 = LINE ( 'NONE', #40182, #10299 ) ;
#25043 = CARTESIAN_POINT ( 'NONE',  ( -46.69597344681494633, -1.750000000000009992, 160.8182875569279702 ) ) ;
#25044 = ADVANCED_FACE ( 'NONE', ( #21352 ), #13658, .T. ) ;
#25045 = CARTESIAN_POINT ( 'NONE',  ( -19.99999999999783995, 17.00000000000000000, 95.00000000000000000 ) ) ;
#25046 = VECTOR ( 'NONE', #30674, 1000.000000000000227 ) ;
#25047 = AXIS2_PLACEMENT_3D ( 'NONE', #22759, #38431, #3245 ) ;
#25048 = CARTESIAN_POINT ( 'NONE',  ( 8.277096487746778308, -50.00000000000000711, 7.455576670931136185 ) ) ;
#25049 = CARTESIAN_POINT ( 'NONE',  ( -206.6959734468149463, -1.750000000000010658, 120.8182875569279702 ) ) ;
#25050 = VECTOR ( 'NONE', #12403, 1000.000000000000114 ) ;
#25051 = CARTESIAN_POINT ( 'NONE',  ( 155.0540265531850537, 1.025126265847089213, -160.9317124430720014 ) ) ;
#25052 = ORIENTED_EDGE ( 'NONE', *, *, #14680, .F. ) ;
#25053 = FACE_OUTER_BOUND ( 'NONE', #8624, .T. ) ;
#25054 = AXIS2_PLACEMENT_3D ( 'NONE', #11501, #46362, #34867 ) ;
#25055 = CARTESIAN_POINT ( 'NONE',  ( -165.3973046169136012, 54.43801056904003133, -17.65743994998275213 ) ) ;
#25056 = AXIS2_PLACEMENT_3D ( 'NONE', #46106, #10999, #26900 ) ;
#25057 = CYLINDRICAL_SURFACE ( 'NONE', #23728, 1.750000000000015543 ) ;
#25058 = DIRECTION ( 'NONE',  ( 0.000000000000000000, 0.000000000000000000, 1.000000000000000000 ) ) ;
#25059 = DIRECTION ( 'NONE',  ( -0.000000000000000000, -0.000000000000000000, -1.000000000000000000 ) ) ;
#25060 = EDGE_LOOP ( 'NONE', ( #44688, #39951, #4926, #28341, #11224, #42514, #44741, #17547 ) ) ;
#25061 = EDGE_LOOP ( 'NONE', ( #12858, #32605, #48054, #18702 ) ) ;
#25062 = CARTESIAN_POINT ( 'NONE',  ( 210.0000000000000568, 2.143131898507880377E-16, 159.0682875569279702 ) ) ;
#25063 = ORIENTED_EDGE ( 'NONE', *, *, #19259, .F. ) ;
#25064 = VECTOR ( 'NONE', #14540, 1000.000000000000000 ) ;
#25065 = ADVANCED_FACE ( 'NONE', ( #37538 ), #3299, .T. ) ;
#25066 = CARTESIAN_POINT ( 'NONE',  ( 33.30402655318503946, -1.750000000000010658, -119.1817124430720440 ) ) ;
#25067 = ORIENTED_EDGE ( 'NONE', *, *, #21310, .T. ) ;
#25068 = CARTESIAN_POINT ( 'NONE',  ( 342.0000000000000568, 181.0000000000000284, 349.9999999999998863 ) ) ;
#25069 = DIRECTION ( 'NONE',  ( 0.000000000000000000, 0.000000000000000000, 1.000000000000000000 ) ) ;
#25070 =( BOUNDED_CURVE ( )  B_SPLINE_CURVE ( 3, ( #2016, #17658, #1517, #48908 ),
 .UNSPECIFIED., .F., .F. ) 
 B_SPLINE_CURVE_WITH_KNOTS ( ( 4, 4 ),
 ( 3.141592653589793116, 4.712388980384689674 ),
 .UNSPECIFIED. ) 
 CURVE ( )  GEOMETRIC_REPRESENTATION_ITEM ( )  RATIONAL_B_SPLINE_CURVE ( ( 1.000000000000000000, 0.8047378541243649375, 0.8047378541243649375, 1.000000000000000000 ) ) 
 REPRESENTATION_ITEM ( '' )  );
#25071 = ORIENTED_EDGE ( 'NONE', *, *, #38479, .F. ) ;
#25072 = ORIENTED_EDGE ( 'NONE', *, *, #31825, .T. ) ;
#25073 = CARTESIAN_POINT ( 'NONE',  ( 0.4611230188129936125, -1.144552435864506279, 9.969907203203808521 ) ) ;
#25074 = CARTESIAN_POINT ( 'NONE',  ( 33.64889274059390090, -3.704246042440748621, 8.356839323120299312 ) ) ;
#25075 = FACE_OUTER_BOUND ( 'NONE', #4988, .T. ) ;
#25076 = CIRCLE ( 'NONE', #29179, 4.000000000000003553 ) ;
#25077 = EDGE_LOOP ( 'NONE', ( #50603, #29978, #603 ) ) ;
#25078 = DIRECTION ( 'NONE',  ( -1.000000000000000000, 0.000000000000000000, -1.612977847700450206E-50 ) ) ;
#25079 = EDGE_CURVE ( 'NONE', #12918, #23110, #2933, .T. ) ;
#25080 = CARTESIAN_POINT ( 'NONE',  ( -84.94597344681494633, 2.143131898507880377E-16, 2.568287556927978166 ) ) ;
#25081 = ORIENTED_EDGE ( 'NONE', *, *, #8276, .T. ) ;
#25082 = VECTOR ( 'NONE', #18859, 1000.000000000000000 ) ;
#25083 = ORIENTED_EDGE ( 'NONE', *, *, #45211, .F. ) ;
#25084 = VERTEX_POINT ( 'NONE', #9560 ) ;
#25085 = CARTESIAN_POINT ( 'NONE',  ( 183.0000000000000284, -174.9999999999999716, -111.0000000000001563 ) ) ;
#25086 = CARTESIAN_POINT ( 'NONE',  ( -114.9999999999994031, 17.00000000000000000, -30.00000000000000000 ) ) ;
#25087 = ORIENTED_EDGE ( 'NONE', *, *, #16112, .T. ) ;
#25088 = B_SPLINE_CURVE_WITH_KNOTS ( 'NONE', 3,
 ( #45949, #11340, #26987, #2861 ),
 .UNSPECIFIED., .F., .F.,
 ( 4, 4 ),
 ( 0.000000000000000000, 0.001249001861321276038 ),
 .UNSPECIFIED. ) ;
#25089 = EDGE_CURVE ( 'NONE', #43884, #41782, #49795, .T. ) ;
#25090 = CARTESIAN_POINT ( 'NONE',  ( 35.05402655318504657, 2.143131898507880377E-16, 159.0682875569279702 ) ) ;
#25091 = CARTESIAN_POINT ( 'NONE',  ( 74.32915281903215998, 1.750000000000009326, 161.8434138227750907 ) ) ;
#25092 = EDGE_CURVE ( 'NONE', #27259, #15078, #9798, .T. ) ;
#25093 = VECTOR ( 'NONE', #6329, 1000.000000000000000 ) ;
#25094 = FACE_OUTER_BOUND ( 'NONE', #42780, .T. ) ;
#25095 = CARTESIAN_POINT ( 'NONE',  ( 194.9999999999999432, 0.000000000000000000, 0.000000000000000000 ) ) ;
#25096 = AXIS2_PLACEMENT_3D ( 'NONE', #5202, #39871, #17004 ) ;
#25097 = DIRECTION ( 'NONE',  ( -0.000000000000000000, 1.000000000000000000, 0.000000000000000000 ) ) ;
#25099 = ADVANCED_FACE ( 'NONE', ( #50201 ), #34621, .T. ) ;
#25098 = CARTESIAN_POINT ( 'NONE',  ( -204.9459734468149463, 2.143131898507880377E-16, -80.93171244307201562 ) ) ;
#25100 = DIRECTION ( 'NONE',  ( 0.000000000000000000, 0.000000000000000000, -1.000000000000000000 ) ) ;
#25101 = PLANE ( 'NONE',  #2279 ) ;
#25102 = AXIS2_PLACEMENT_3D ( 'NONE', #41846, #21581, #14394 ) ;
#25103 = CARTESIAN_POINT ( 'NONE',  ( 1.011271242968688311, -0.7347315653655855927, 10.00000000000000000 ) ) ;
#25104 = DIRECTION ( 'NONE',  ( -0.000000000000000000, -0.000000000000000000, -1.000000000000000000 ) ) ;
#25105 = ORIENTED_EDGE ( 'NONE', *, *, #45940, .F. ) ;
#25106 = CARTESIAN_POINT ( 'NONE',  ( 194.9999999999999432, -173.0000000000000000, 372.0000000000000568 ) ) ;
#25107 = CARTESIAN_POINT ( 'NONE',  ( -0.5113015165352315927, -1.175527691268679398, 9.948547179989621014 ) ) ;
#25108 = DIRECTION ( 'NONE',  ( -0.000000000000000000, -1.000000000000000000, -0.000000000000000000 ) ) ;
#25109 = CARTESIAN_POINT ( 'NONE',  ( -165.6708471809677974, -1.750000000000009326, 159.7931612910809065 ) ) ;
#25110 = VERTEX_POINT ( 'NONE', #15113 ) ;
#25111 = CARTESIAN_POINT ( 'NONE',  ( -114.9999999999987779, 17.00000000000000000, 5.000000000000004441 ) ) ;
#25112 = VECTOR ( 'NONE', #26712, 1000.000000000000000 ) ;
#25113 = PLANE ( 'NONE',  #42591 ) ;
#25114 = VECTOR ( 'NONE', #32150, 1000.000000000000000 ) ;
#25115 = EDGE_LOOP ( 'NONE', ( #34240, #37594 ) ) ;
#25116 = CARTESIAN_POINT ( 'NONE',  ( 31.94178169330218964, -9.256608784833820991, -3.760136334089591248 ) ) ;
#25117 = CARTESIAN_POINT ( 'NONE',  ( 23.13346437080453555, -39.73622551878964515, -8.016098858316205167 ) ) ;
#25118 = CARTESIAN_POINT ( 'NONE',  ( 1.962558162476984114, -3.366505435497487042, 9.741991644047251597 ) ) ;
#25119 = EDGE_LOOP ( 'NONE', ( #17299, #24419, #30827, #20649 ) ) ;
#25120 = FILL_AREA_STYLE ('',( #28958 ) ) ;
#25121 = ORIENTED_EDGE ( 'NONE', *, *, #7437, .T. ) ;
#25122 = ORIENTED_EDGE ( 'NONE', *, *, #39750, .F. ) ;
#25123 = ADVANCED_FACE ( 'NONE', ( #33182 ), #46383, .T. ) ;
#25124 =( BOUNDED_CURVE ( )  B_SPLINE_CURVE ( 3, ( #17845, #49356, #45525, #18839 ),
 .UNSPECIFIED., .F., .F. ) 
 B_SPLINE_CURVE_WITH_KNOTS ( ( 4, 4 ),
 ( 1.570796326794896558, 3.141592653589793116 ),
 .UNSPECIFIED. ) 
 CURVE ( )  GEOMETRIC_REPRESENTATION_ITEM ( )  RATIONAL_B_SPLINE_CURVE ( ( 1.000000000000000000, 0.8047378541243649375, 0.8047378541243649375, 1.000000000000000000 ) ) 
 REPRESENTATION_ITEM ( '' )  );
#25125 = AXIS2_PLACEMENT_3D ( 'NONE', #27226, #23370, #39036 ) ;
#25126 = ORIENTED_EDGE ( 'NONE', *, *, #26632, .T. ) ;
#25127 = DIRECTION ( 'NONE',  ( 0.000000000000000000, 0.000000000000000000, 1.000000000000000000 ) ) ;
#25128 = CARTESIAN_POINT ( 'NONE',  ( -88.44597344681497475, 0.000000000000000000, 122.5682875569279986 ) ) ;
#25129 = VECTOR ( 'NONE', #14797, 1000.000000000000000 ) ;
#25130 = VECTOR ( 'NONE', #33994, 1000.000000000000000 ) ;
#25131 = ORIENTED_EDGE ( 'NONE', *, *, #10352, .T. ) ;
#25132 = CARTESIAN_POINT ( 'NONE',  ( 29.18392875402930997, 17.44843138996603216, 7.906207997025717304 ) ) ;
#25133 = DIRECTION ( 'NONE',  ( 1.000000000000000000, -0.000000000000000000, -0.000000000000000000 ) ) ;
#25134 = DIRECTION ( 'NONE',  ( 0.5038710255240862468, 0.000000000000000000, 0.8637789008984334549 ) ) ;
#25135 =( BOUNDED_CURVE ( )  B_SPLINE_CURVE ( 3, ( #32183, #23975, #8580, #20624 ),
 .UNSPECIFIED., .F., .F. ) 
 B_SPLINE_CURVE_WITH_KNOTS ( ( 4, 4 ),
 ( 1.586958686267286008E-16, 1.570796326794896780 ),
 .UNSPECIFIED. ) 
 CURVE ( )  GEOMETRIC_REPRESENTATION_ITEM ( )  RATIONAL_B_SPLINE_CURVE ( ( 1.000000000000000000, 0.8047378541243649375, 0.8047378541243649375, 1.000000000000000000 ) ) 
 REPRESENTATION_ITEM ( '' )  );
#25136 = LINE ( 'NONE', #48173, #5492 ) ;
#25137 = ORIENTED_EDGE ( 'NONE', *, *, #10239, .F. ) ;
#25138 = VECTOR ( 'NONE', #32842, 1000.000000000000000 ) ;
#25139 = DIRECTION ( 'NONE',  ( -1.000000000000000000, 0.000000000000000000, -2.958228394578794708E-31 ) ) ;
#25140 = ORIENTED_EDGE ( 'NONE', *, *, #7478, .F. ) ;
#25141 = CARTESIAN_POINT ( 'NONE',  ( -8.445973446814976526, 0.000000000000000000, 2.568287556928034121 ) ) ;
#25142 = CARTESIAN_POINT ( 'NONE',  ( -14.49999999999999822, -46.01315789473684248, 5.916985404131813731 ) ) ;
#25143 = EDGE_LOOP ( 'NONE', ( #28574, #42154, #35649, #21669 ) ) ;
#25144 = ORIENTED_EDGE ( 'NONE', *, *, #42546, .T. ) ;
#25145 = ORIENTED_EDGE ( 'NONE', *, *, #37116, .F. ) ;
#25146 = CARTESIAN_POINT ( 'NONE',  ( -166.6959734468149463, 0.000000000000000000, 165.0000000000000000 ) ) ;
#25147 = FACE_OUTER_BOUND ( 'NONE', #10632, .T. ) ;
#25148 = ORIENTED_EDGE ( 'NONE', *, *, #48841, .F. ) ;
#25149 = DIRECTION ( 'NONE',  ( 0.000000000000000000, -1.000000000000000000, 0.000000000000000000 ) ) ;
#25150 = DIRECTION ( 'NONE',  ( 1.000000000000000000, 0.000000000000000000, 0.000000000000000000 ) ) ;
#25151 = LINE ( 'NONE', #37473, #9190 ) ;
#25152 = VECTOR ( 'NONE', #10731, 1000.000000000000000 ) ;
#25153 = VERTEX_POINT ( 'NONE', #44680 ) ;
#25154 = CARTESIAN_POINT ( 'NONE',  ( 2.500000000000001776, 214.9999999999999716, -230.2499999999999716 ) ) ;
#25155 = EDGE_CURVE ( 'NONE', #9119, #19888, #23936, .T. ) ;
#25156 = CARTESIAN_POINT ( 'NONE',  ( 19.00512336303704686, -32.33518880947659113, -8.600750091277033604 ) ) ;
#25157 = VERTEX_POINT ( 'NONE', #29557 ) ;
#25158 = ORIENTED_EDGE ( 'NONE', *, *, #38112, .T. ) ;
#25159 = APPLICATION_PROTOCOL_DEFINITION ( 'draft international standard', 'automotive_design', 1998, #6639 ) ;
#25160 = DIRECTION ( 'NONE',  ( 0.9928768384869219865, 0.000000000000000000, 0.1191452206184307749 ) ) ;
#25161 = DIRECTION ( 'NONE',  ( 0.4740998230350171871, 0.3386427307392981256, -0.8127425537743158124 ) ) ;
#25162 = CARTESIAN_POINT ( 'NONE',  ( -44.99506233596265048, -23.32283626942287569, 7.455576670931136185 ) ) ;
#25163 = DIRECTION ( 'NONE',  ( -1.000000000000000000, -0.000000000000000000, -0.000000000000000000 ) ) ;
#25164 = VERTEX_POINT ( 'NONE', #14145 ) ;
#25165 = PLANE ( 'NONE',  #23068 ) ;
#25166 = FACE_OUTER_BOUND ( 'NONE', #223, .T. ) ;
#25167 = CARTESIAN_POINT ( 'NONE',  ( -208.4459734468149463, 0.000000000000000000, 165.0000000000000000 ) ) ;
#25168 = VECTOR ( 'NONE', #31902, 1000.000000000000000 ) ;
#25169 = VERTEX_POINT ( 'NONE', #19198 ) ;
#25170 = ORIENTED_EDGE ( 'NONE', *, *, #22507, .F. ) ;
#25171 = CARTESIAN_POINT ( 'NONE',  ( 214.9999999999999432, 164.9999999999999716, 500.0000000000000000 ) ) ;
#25172 = ORIENTED_EDGE ( 'NONE', *, *, #21102, .T. ) ;
#25173 = CARTESIAN_POINT ( 'NONE',  ( 341.9999999999999432, -181.0000000000001421, -356.0000000000003411 ) ) ;
#25174 = ADVANCED_FACE ( 'NONE', ( #34887 ), #2360, .F. ) ;
#25176 = CARTESIAN_POINT ( 'NONE',  ( 55.00000000000002132, -52.50000000000000711, 5.000000000000000000 ) ) ;
#25175 = B_SPLINE_CURVE_WITH_KNOTS ( 'NONE', 3,
 ( #11273, #6650, #22552, #26404 ),
 .UNSPECIFIED., .F., .F.,
 ( 4, 4 ),
 ( 0.000000000000000000, 0.0001252128669263292060 ),
 .UNSPECIFIED. ) ;
#25177 = VERTEX_POINT ( 'NONE', #21873 ) ;
#25178 = CYLINDRICAL_SURFACE ( 'NONE', #765, 1.750000000000015543 ) ;
#25179 = AXIS2_PLACEMENT_3D ( 'NONE', #35922, #47404, #28956 ) ;
#25180 = ORIENTED_EDGE ( 'NONE', *, *, #50337, .T. ) ;
#25181 = CARTESIAN_POINT ( 'NONE',  ( 214.9999999999999432, -175.0000000000000000, 474.0000000000000000 ) ) ;
#25182 = CARTESIAN_POINT ( 'NONE',  ( -9.907356528110963012, 1.358045148327947427, 0.000000000000000000 ) ) ;
#25183 = CARTESIAN_POINT ( 'NONE',  ( 73.30402655318508209, 0.000000000000000000, 165.0000000000000000 ) ) ;
#25184 = LINE ( 'NONE', #44160, #3713 ) ;
#25185 = FACE_OUTER_BOUND ( 'NONE', #23678, .T. ) ;
#25186 = VERTEX_POINT ( 'NONE', #17998 ) ;
#25187 = ORIENTED_EDGE ( 'NONE', *, *, #30567, .T. ) ;
#25188 = DIRECTION ( 'NONE',  ( 1.000000000000000000, 0.000000000000000000, 0.000000000000000000 ) ) ;
#25189 = EDGE_LOOP ( 'NONE', ( #6121, #39432, #1274, #12104 ) ) ;
#25190 = DIRECTION ( 'NONE',  ( -1.000000000000000000, -0.000000000000000000, -0.000000000000000000 ) ) ;
#25191 = CARTESIAN_POINT ( 'NONE',  ( 0.000000000000000000, -180.9999999999999716, -356.0000000000002274 ) ) ;
#25192 = ORIENTED_EDGE ( 'NONE', *, *, #46532, .F. ) ;
#25193 = CARTESIAN_POINT ( 'NONE',  ( 181.0000000000000000, 10.00000000000006395, 339.9999999999998295 ) ) ;
#25194 = CARTESIAN_POINT ( 'NONE',  ( 151.5540265531850537, -1.025126265847089657, 79.06828755692797017 ) ) ;
#25195 = B_SPLINE_SURFACE_WITH_KNOTS ( 'NONE', 3, 3, ( 
 ( #31699, #388, #16787, #8338 ),
 ( #896, #16034, #40398, #23729 ),
 ( #32448, #12180, #27835, #35814 ),
 ( #12920, #4474, #636, #43468 ) ),
 .UNSPECIFIED., .F., .F., .F.,
 ( 4, 4 ),
 ( 4, 4 ),
 ( 0.000000000000000000, 1.000000000000000000 ),
 ( 0.000000000000000000, 1.000000000000000000 ),
 .UNSPECIFIED. ) ;
#25196 = ORIENTED_EDGE ( 'NONE', *, *, #48677, .F. ) ;
#25197 = DIRECTION ( 'NONE',  ( -1.000000000000000000, 0.000000000000000000, 0.000000000000000000 ) ) ;
#25198 = CARTESIAN_POINT ( 'NONE',  ( -125.6708471809678542, 1.749999999999996669, -40.20683870891911482 ) ) ;
#25199 = CARTESIAN_POINT ( 'NONE',  ( -165.3973046169136012, -98.56198943095992604, 22.84256005001721945 ) ) ;
#25200 = DIRECTION ( 'NONE',  ( 1.000000000000000000, -0.000000000000000000, -0.000000000000000000 ) ) ;
#25201 = EDGE_CURVE ( 'NONE', #15011, #40834, #33674, .T. ) ;
#25202 = VERTEX_POINT ( 'NONE', #29817 ) ;
#25203 = EDGE_CURVE ( 'NONE', #50033, #41657, #48160, .T. ) ;
#25204 = ORIENTED_EDGE ( 'NONE', *, *, #35539, .F. ) ;
#25205 = VERTEX_POINT ( 'NONE', #4814 ) ;
#25206 = CARTESIAN_POINT ( 'NONE',  ( 356.0000000000001137, 167.0000000000000000, 349.9999999999998863 ) ) ;
#25208 = EDGE_CURVE ( 'NONE', #19221, #5824, #4458, .T. ) ;
#25207 = LINE ( 'NONE', #5953, #6233 ) ;
#25209 = CARTESIAN_POINT ( 'NONE',  ( -10.00000000000003375, 8.486842105263161073, -18.38522261288946780 ) ) ;
#25210 = CARTESIAN_POINT ( 'NONE',  ( -1.066995270233474624, 50.00000000000000711, -3.760136334089591248 ) ) ;
#25211 = ORIENTED_EDGE ( 'NONE', *, *, #28650, .T. ) ;
#25212 = EDGE_CURVE ( 'NONE', #7227, #27797, #15921, .T. ) ;
#25213 = CARTESIAN_POINT ( 'NONE',  ( -84.94597344681494633, 2.143131898507880377E-16, 39.06828755692798438 ) ) ;
#25214 = EDGE_LOOP ( 'NONE', ( #3151, #1651, #743, #42600, #42172, #40545 ) ) ;
#25215 = EDGE_CURVE ( 'NONE', #11044, #14334, #28189, .T. ) ;
#25216 = CARTESIAN_POINT ( 'NONE',  ( -207.2473046169136808, -154.8119894309599260, 470.5025600500171095 ) ) ;
#25217 = CARTESIAN_POINT ( 'NONE',  ( -207.2473046169136808, -154.8119894309599260, 472.8425600500171981 ) ) ;
#25218 = CARTESIAN_POINT ( 'NONE',  ( -5.670847180967843570, -1.750000000000023981, 119.7931612910808781 ) ) ;
#25219 = VECTOR ( 'NONE', #14481, 1000.000000000000000 ) ;
#25220 = CARTESIAN_POINT ( 'NONE',  ( -1.057156451998854996, 0.7920882637787067804, 9.943883492372851407 ) ) ;
#25221 = DIRECTION ( 'NONE',  ( -0.000000000000000000, -1.000000000000000000, -0.000000000000000000 ) ) ;
#25222 = ORIENTED_EDGE ( 'NONE', *, *, #18044, .F. ) ;
#25223 = CYLINDRICAL_SURFACE ( 'NONE', #1812, 1.880036658038868103 ) ;
#25224 = DIRECTION ( 'NONE',  ( 0.000000000000000000, -1.000000000000000000, 0.000000000000000000 ) ) ;
#25225 = CARTESIAN_POINT ( 'NONE',  ( -210.0000000000000568, 0.000000000000000000, 80.81828755692798438 ) ) ;
#25226 = DIRECTION ( 'NONE',  ( -0.9928768384869219865, 0.000000000000000000, -0.1191452206184307888 ) ) ;
#25227 = VERTEX_POINT ( 'NONE', #3817 ) ;
#25228 = DIRECTION ( 'NONE',  ( 0.000000000000000000, -1.000000000000000000, -3.186989995019654210E-49 ) ) ;
#25229 = VERTEX_POINT ( 'NONE', #35657 ) ;
#25230 = CARTESIAN_POINT ( 'NONE',  ( -44.94597344681493922, 1.025126265847089879, 82.56828755692798438 ) ) ;
#25231 = CARTESIAN_POINT ( 'NONE',  ( 75.05402655318509630, -1.025126265847088991, 2.568287556927986159 ) ) ;
#25232 = AXIS2_PLACEMENT_3D ( 'NONE', #19843, #38613, #23956 ) ;
#25233 = EDGE_CURVE ( 'NONE', #16307, #16010, #23311, .T. ) ;
#25234 = CARTESIAN_POINT ( 'NONE',  ( 17.51065725283127250, -28.41934970907778890, -9.367992836599951190 ) ) ;
#25235 = EDGE_CURVE ( 'NONE', #1878, #25941, #31795, .T. ) ;
#25236 = ORIENTED_EDGE ( 'NONE', *, *, #42017, .T. ) ;
#25237 = EDGE_CURVE ( 'NONE', #15030, #39856, #16205, .T. ) ;
#25238 = EDGE_CURVE ( 'NONE', #1115, #14362, #35146, .T. ) ;
#25239 = CARTESIAN_POINT ( 'NONE',  ( -0.3862712429686729343, -1.188820645368946050, -10.00000000000000000 ) ) ;
#25240 = LINE ( 'NONE', #5732, #20433 ) ;
#25241 = LINE ( 'NONE', #9092, #41739 ) ;
#25242 = ADVANCED_FACE ( 'NONE', ( #27175 ), #15618, .F. ) ;
#25243 = LINE ( 'NONE', #48545, #18466 ) ;
#25244 = EDGE_CURVE ( 'NONE', #26079, #7763, #27933, .T. ) ;
#25245 = VERTEX_POINT ( 'NONE', #20470 ) ;
#25246 = ORIENTED_EDGE ( 'NONE', *, *, #36140, .F. ) ;
#25247 = DIRECTION ( 'NONE',  ( -1.000000000000000000, 0.000000000000000000, 0.000000000000000000 ) ) ;
#25248 = DIRECTION ( 'NONE',  ( -0.000000000000000000, -0.000000000000000000, -1.000000000000000000 ) ) ;
#25249 = ORIENTED_EDGE ( 'NONE', *, *, #26127, .F. ) ;
#25250 = VERTEX_POINT ( 'NONE', #35400 ) ;
#25251 = CARTESIAN_POINT ( 'NONE',  ( 183.0000000000000284, -174.9999999999999716, -111.0000000000001563 ) ) ;
#25252 = DIRECTION ( 'NONE',  ( -0.000000000000000000, -0.000000000000000000, -1.000000000000000000 ) ) ;
#25253 = CARTESIAN_POINT ( 'NONE',  ( 34.32915281903212446, 1.750000000000009548, 159.7931612910809065 ) ) ;
#25254 = CARTESIAN_POINT ( 'NONE',  ( 113.3040265531850537, -1.749999999999997335, 80.81828755692798438 ) ) ;
#25255 = ORIENTED_EDGE ( 'NONE', *, *, #29840, .T. ) ;
#25256 = VERTEX_POINT ( 'NONE', #36148 ) ;
#25257 = ORIENTED_EDGE ( 'NONE', *, *, #11177, .T. ) ;
#25258 = EDGE_CURVE ( 'NONE', #30782, #9269, #11206, .T. ) ;
#25259 = CARTESIAN_POINT ( 'NONE',  ( 31.55402655318506788, 2.143131898507880377E-16, -160.9317124430720298 ) ) ;
#25260 =( BOUNDED_CURVE ( )  B_SPLINE_CURVE ( 3, ( #4170, #24184, #35486, #333 ),
 .UNSPECIFIED., .F., .F. ) 
 B_SPLINE_CURVE_WITH_KNOTS ( ( 4, 4 ),
 ( 1.570796326794896780, 3.141592653589793116 ),
 .UNSPECIFIED. ) 
 CURVE ( )  GEOMETRIC_REPRESENTATION_ITEM ( )  RATIONAL_B_SPLINE_CURVE ( ( 1.000000000000000000, 0.8047378541243650485, 0.8047378541243650485, 1.000000000000000000 ) ) 
 REPRESENTATION_ITEM ( '' )  );
#25261 = DIRECTION ( 'NONE',  ( -4.485344387572531843E-16, -0.7071067811865476838, -0.7071067811865473507 ) ) ;
#25262 = EDGE_CURVE ( 'NONE', #9366, #25957, #41017, .T. ) ;
#25263 = EDGE_CURVE ( 'NONE', #41151, #28572, #16376, .T. ) ;
#25264 = ORIENTED_EDGE ( 'NONE', *, *, #12214, .F. ) ;
#25265 = EDGE_LOOP ( 'NONE', ( #29979, #14259, #1018, #19133, #31911, #32021, #4746, #26943 ) ) ;
#25266 =( BOUNDED_CURVE ( )  B_SPLINE_CURVE ( 3, ( #13892, #10064, #41111, #25719 ),
 .UNSPECIFIED., .F., .F. ) 
 B_SPLINE_CURVE_WITH_KNOTS ( ( 4, 4 ),
 ( 0.000000000000000000, 1.570796326794896558 ),
 .UNSPECIFIED. ) 
 CURVE ( )  GEOMETRIC_REPRESENTATION_ITEM ( )  RATIONAL_B_SPLINE_CURVE ( ( 1.000000000000000000, 0.8047378541243649375, 0.8047378541243649375, 1.000000000000000000 ) ) 
 REPRESENTATION_ITEM ( '' )  );
#25267 = CARTESIAN_POINT ( 'NONE',  ( 29.18392875402930997, 17.44843138996603216, 7.906207997025717304 ) ) ;
#25268 = ORIENTED_EDGE ( 'NONE', *, *, #42860, .T. ) ;
#25269 = ORIENTED_EDGE ( 'NONE', *, *, #43112, .F. ) ;
#25270 = FACE_OUTER_BOUND ( 'NONE', #37406, .T. ) ;
#25271 = DIRECTION ( 'NONE',  ( -1.000000000000000000, 0.000000000000000000, 0.000000000000000000 ) ) ;
#25272 = VERTEX_POINT ( 'NONE', #32045 ) ;
#25273 = CARTESIAN_POINT ( 'NONE',  ( 6.875132362119187768, -33.14667368551891258, 8.356839323120299312 ) ) ;
#25274 = LINE ( 'NONE', #40431, #28693 ) ;
#25275 = CARTESIAN_POINT ( 'NONE',  ( -0.8965959638259611841, -1.582931917743307215, 9.903764339332084887 ) ) ;
#25276 = CARTESIAN_POINT ( 'NONE',  ( 155.0540265531850537, 2.143131898507880377E-16, -157.4317124430720582 ) ) ;
#25277 = CARTESIAN_POINT ( 'NONE',  ( 151.5540265531850537, 0.000000000000000000, 2.568287556927978166 ) ) ;
#25278 = ORIENTED_EDGE ( 'NONE', *, *, #18125, .T. ) ;
#25279 = EDGE_CURVE ( 'NONE', #16425, #13764, #32743, .T. ) ;
#25280 = DIRECTION ( 'NONE',  ( -1.000000000000000000, -0.000000000000000000, -0.000000000000000000 ) ) ;
#25281 = CARTESIAN_POINT ( 'NONE',  ( 210.0000000000000568, 0.000000000000000000, 40.81828755692798438 ) ) ;
#25282 =( BOUNDED_CURVE ( )  B_SPLINE_CURVE ( 3, ( #35890, #19712, #35391, #4574 ),
 .UNSPECIFIED., .F., .F. ) 
 B_SPLINE_CURVE_WITH_KNOTS ( ( 4, 4 ),
 ( 4.712388980384689674, 6.283185307179586232 ),
 .UNSPECIFIED. ) 
 CURVE ( )  GEOMETRIC_REPRESENTATION_ITEM ( )  RATIONAL_B_SPLINE_CURVE ( ( 1.000000000000000000, 0.8047378541243649375, 0.8047378541243649375, 1.000000000000000000 ) ) 
 REPRESENTATION_ITEM ( '' )  );
#25283 = CARTESIAN_POINT ( 'NONE',  ( -34.38425513258695077, 36.82177522737848108, 8.807470649214879543 ) ) ;
#25284 = CARTESIAN_POINT ( 'NONE',  ( 35.00000000000028422, 17.00000000000000000, -84.99999999999998579 ) ) ;
#25285 = VECTOR ( 'NONE', #32179, 1000.000000000000000 ) ;
#25286 = CARTESIAN_POINT ( 'NONE',  ( -1.589327968330880969, -0.05051906867692697312, 9.933337059263775970 ) ) ;
#25287 = CARTESIAN_POINT ( 'NONE',  ( -4.945973446814903696, 2.143131898507912917E-16, 165.0000000000000000 ) ) ;
#25288 = EDGE_CURVE ( 'NONE', #50205, #5524, #11934, .T. ) ;
#25289 = FACE_OUTER_BOUND ( 'NONE', #1489, .T. ) ;
#25290 = CARTESIAN_POINT ( 'NONE',  ( -10.49999999999999467, -46.01315789473684248, 5.916985404131813731 ) ) ;
#25291 = CLOSED_SHELL ( 'NONE', ( #2234, #35285, #28707, #22374 ) ) ;
#25292 = CARTESIAN_POINT ( 'NONE',  ( 1.540662627795932105, -1.371465786296032441, 9.894754715216729224 ) ) ;
#25293 = ORIENTED_EDGE ( 'NONE', *, *, #42556, .T. ) ;
#25294 = CARTESIAN_POINT ( 'NONE',  ( -1.011271242968688533, 0.7347315653655859258, 10.00000000000000000 ) ) ;
#25295 = EDGE_CURVE ( 'NONE', #9096, #11140, #21098, .T. ) ;
#25296 = ADVANCED_FACE ( 'NONE', ( #4075 ), #9431, .T. ) ;
#25297 = CARTESIAN_POINT ( 'NONE',  ( -47.22310614333779455, -16.46562252335923660, -3.760136334089591248 ) ) ;
#25298 = FACE_OUTER_BOUND ( 'NONE', #26278, .T. ) ;
#25299 = CARTESIAN_POINT ( 'NONE',  ( -1.011271242968677875, -0.7347315653656004697, 10.00000000000000000 ) ) ;
#25300 = FACE_OUTER_BOUND ( 'NONE', #19701, .T. ) ;
#25301 = EDGE_CURVE ( 'NONE', #14400, #169, #5330, .T. ) ;
#25302 = EDGE_LOOP ( 'NONE', ( #11915, #46858, #50187, #13386, #29919, #4569, #6402, #19807, #37860, #8426, #38089, #49371, #34185, #28297 ) ) ;
#25303 = PLANE ( 'NONE',  #22448 ) ;
#25304 = B_SPLINE_SURFACE_WITH_KNOTS ( 'NONE', 3, 3, ( 
 ( #5795, #44267, #12735, #25294 ),
 ( #9139, #40951, #37123, #13486 ),
 ( #24799, #40451, #20943, #32750 ),
 ( #48344, #13232, #28894, #29393 ) ),
 .UNSPECIFIED., .F., .F., .F.,
 ( 4, 4 ),
 ( 4, 4 ),
 ( 0.000000000000000000, 1.000000000000000000 ),
 ( 0.000000000000000000, 1.000000000000000000 ),
 .UNSPECIFIED. ) ;
#25305 = VERTEX_POINT ( 'NONE', #44065 ) ;
#25306 = CARTESIAN_POINT ( 'NONE',  ( 357.9999999999999432, -181.0000000000001421, -356.0000000000003979 ) ) ;
#25307 = EDGE_CURVE ( 'NONE', #5304, #9422, #40237, .T. ) ;
#25308 = DIRECTION ( 'NONE',  ( 0.000000000000000000, -2.537652627714643577E-15, -1.000000000000000000 ) ) ;
#25309 = EDGE_CURVE ( 'NONE', #2518, #29162, #18372, .T. ) ;
#25310 = EDGE_LOOP ( 'NONE', ( #25579, #38470, #4651, #42961 ) ) ;
#25311 = CARTESIAN_POINT ( 'NONE',  ( -0.4166666666666669072, 0.000000000000000000, 10.00000000000000000 ) ) ;
#25312 = DIRECTION ( 'NONE',  ( -1.000000000000000000, -0.000000000000000000, -0.000000000000000000 ) ) ;
#25313 = ORIENTED_EDGE ( 'NONE', *, *, #32601, .T. ) ;
#25314 = VERTEX_POINT ( 'NONE', #20990 ) ;
#25315 = EDGE_CURVE ( 'NONE', #40327, #38568, #29188, .T. ) ;
#25316 = CARTESIAN_POINT ( 'NONE',  ( 191.5540265531850537, -1.025126265847089879, 122.5682875569280128 ) ) ;
#25317 = CARTESIAN_POINT ( 'NONE',  ( -207.2473046169136808, 159.2880105690400399, 472.8425600500171981 ) ) ;
#25318 = VECTOR ( 'NONE', #27879, 1000.000000000000000 ) ;
#25319 = CARTESIAN_POINT ( 'NONE',  ( 0.2834763335391893846, -1.876787935832544107, 9.900811091504525763 ) ) ;
#25320 = VERTEX_POINT ( 'NONE', #16893 ) ;
#25321 = AXIS2_PLACEMENT_3D ( 'NONE', #39758, #24601, #40250 ) ;
#25322 = FACE_OUTER_BOUND ( 'NONE', #2968, .T. ) ;
#25323 = DIRECTION ( 'NONE',  ( 0.000000000000000000, 0.000000000000000000, -1.000000000000000000 ) ) ;
#25324 = SURFACE_STYLE_USAGE ( .BOTH. , #37152 ) ;
#25325 = EDGE_LOOP ( 'NONE', ( #27512, #3934, #32590, #24072 ) ) ;
#25326 = ORIENTED_EDGE ( 'NONE', *, *, #17326, .T. ) ;
#25327 = VERTEX_POINT ( 'NONE', #25592 ) ;
#25328 = CARTESIAN_POINT ( 'NONE',  ( -6.695973446814940111, 0.000000000000000000, 165.0000000000000000 ) ) ;
#25329 = AXIS2_PLACEMENT_3D ( 'NONE', #9004, #48455, #29000 ) ;
#25330 = VECTOR ( 'NONE', #30758, 1000.000000000000000 ) ;
#25331 = CARTESIAN_POINT ( 'NONE',  ( -1.275994128725546739, 0.1230186051320636409, 9.948547179989615685 ) ) ;
#25332 = ORIENTED_EDGE ( 'NONE', *, *, #1054, .F. ) ;
#25333 = AXIS2_PLACEMENT_3D ( 'NONE', #50520, #7488, #46174 ) ;
#25334 = CARTESIAN_POINT ( 'NONE',  ( -45.64490844644706158, -21.32281559348763977, 8.807470649214879543 ) ) ;
#25335 = CARTESIAN_POINT ( 'NONE',  ( -0.4266413953668892756, -1.250184266969579294, 9.943883492372849631 ) ) ;
#25336 = VECTOR ( 'NONE', #47727, 1000.000000000000000 ) ;
#25337 = CARTESIAN_POINT ( 'NONE',  ( -1.275994128725546739, 0.1230186051320636409, 9.948547179989615685 ) ) ;
#25338 = LINE ( 'NONE', #10191, #30446 ) ;
#25339 = CARTESIAN_POINT ( 'NONE',  ( 343.9999999999999432, -185.0000000000001421, -360.0000000000003979 ) ) ;
#25340 = CARTESIAN_POINT ( 'NONE',  ( 31.46770792452135268, -38.94077080897339727, 3.199614146704519602 ) ) ;
#25341 = DIRECTION ( 'NONE',  ( -1.000000000000000000, 0.000000000000000000, -0.000000000000000000 ) ) ;
#25342 = CARTESIAN_POINT ( 'NONE',  ( -164.9459734468149463, 2.143131898507880377E-16, 165.0000000000000000 ) ) ;
#25343 = DIRECTION ( 'NONE',  ( 0.000000000000000000, 0.000000000000000000, 1.000000000000000000 ) ) ;
#25344 = ADVANCED_FACE ( 'NONE', ( #13774 ), #33309, .T. ) ;
#25345 = FACE_OUTER_BOUND ( 'NONE', #9556, .T. ) ;
#25346 = CARTESIAN_POINT ( 'NONE',  ( -5.647304616913629616, 2.688010569040066411, 22.84256005001721945 ) ) ;
#25347 = EDGE_LOOP ( 'NONE', ( #4707, #8323, #42085, #49812, #44270, #47014 ) ) ;
#25348 = CARTESIAN_POINT ( 'NONE',  ( -204.9459734468148895, -1.025126265847089435, 82.56828755692798438 ) ) ;
#25349 = CARTESIAN_POINT ( 'NONE',  ( 210.0000000000000568, 0.000000000000000000, -159.1817124430720298 ) ) ;
#25350 = CARTESIAN_POINT ( 'NONE',  ( 181.0000000000000000, -272.4999999999999432, -359.9999999999999432 ) ) ;
#25351 = AXIS2_PLACEMENT_3D ( 'NONE', #21242, #2247, #9695 ) ;
#25352 = ORIENTED_EDGE ( 'NONE', *, *, #28077, .F. ) ;
#25353 = EDGE_CURVE ( 'NONE', #16301, #7708, #41232, .T. ) ;
#25354 = VECTOR ( 'NONE', #49834, 1000.000000000000000 ) ;
#25355 = EDGE_CURVE ( 'NONE', #23532, #7894, #48886, .T. ) ;
#25356 = CARTESIAN_POINT ( 'NONE',  ( -25.79500241909648395, -7.388441598285492518, 229.0000000000000000 ) ) ;
#25357 =( BOUNDED_CURVE ( )  B_SPLINE_CURVE ( 3, ( #10290, #44896, #29790, #48734 ),
 .UNSPECIFIED., .F., .F. ) 
 B_SPLINE_CURVE_WITH_KNOTS ( ( 4, 4 ),
 ( 3.141592653589793116, 4.712388980384693227 ),
 .UNSPECIFIED. ) 
 CURVE ( )  GEOMETRIC_REPRESENTATION_ITEM ( )  RATIONAL_B_SPLINE_CURVE ( ( 1.000000000000000000, 0.8047378541243641603, 0.8047378541243641603, 1.000000000000000000 ) ) 
 REPRESENTATION_ITEM ( '' )  );
#25358 = EDGE_LOOP ( 'NONE', ( #41970, #27995, #14308, #7735 ) ) ;
#25359 = AXIS2_PLACEMENT_3D ( 'NONE', #10677, #42471, #14267 ) ;
#25360 = CARTESIAN_POINT ( 'NONE',  ( 0.000000000000000000, 13.98684210526316107, -3.750000000000000000 ) ) ;
#25361 = DIRECTION ( 'NONE',  ( -1.000000000000000000, -0.000000000000000000, -0.000000000000000000 ) ) ;
#25362 = VECTOR ( 'NONE', #44557, 1000.000000000000000 ) ;
#25363 = EDGE_CURVE ( 'NONE', #41350, #1434, #13021, .T. ) ;
#25364 = ORIENTED_EDGE ( 'NONE', *, *, #36811, .F. ) ;
#25365 = DIRECTION ( 'NONE',  ( -1.000000000000000000, -0.000000000000000000, -0.000000000000000000 ) ) ;
#25366 = ORIENTED_EDGE ( 'NONE', *, *, #19923, .T. ) ;
#25367 = VERTEX_POINT ( 'NONE', #44309 ) ;
#25368 = ADVANCED_FACE ( 'NONE', ( #40493 ), #44813, .F. ) ;
#25369 = CARTESIAN_POINT ( 'NONE',  ( -14.99999999999937472, 16.00000000000000000, -30.00000000000000000 ) ) ;
#25370 = EDGE_CURVE ( 'NONE', #30782, #43794, #4308, .T. ) ;
#25371 = VECTOR ( 'NONE', #39639, 1000.000000000000000 ) ;
#25372 = ORIENTED_EDGE ( 'NONE', *, *, #17201, .F. ) ;
#25373 = PLANE ( 'NONE',  #23749 ) ;
#25374 = DIRECTION ( 'NONE',  ( -1.000000000000000000, -0.000000000000000000, -0.000000000000000000 ) ) ;
#25375 = ORIENTED_EDGE ( 'NONE', *, *, #37108, .T. ) ;
#25376 = LINE ( 'NONE', #29475, #28703 ) ;
#25377 = CARTESIAN_POINT ( 'NONE',  ( 31.55402655318503236, 0.000000000000000000, -0.9317124430720247208 ) ) ;
#25378 = EDGE_CURVE ( 'NONE', #20650, #15814, #28933, .T. ) ;
#25379 = CARTESIAN_POINT ( 'NONE',  ( 29.99999999999998579, 17.00000000000000000, -114.9999999999999858 ) ) ;
#25380 = FACE_OUTER_BOUND ( 'NONE', #29220, .T. ) ;
#25381 = ORIENTED_EDGE ( 'NONE', *, *, #10829, .F. ) ;
#25382 = B_SPLINE_CURVE_WITH_KNOTS ( 'NONE', 3,
 ( #6503, #22160, #2403, #17804 ),
 .UNSPECIFIED., .F., .F.,
 ( 4, 4 ),
 ( 0.01012863361515542113, 0.01015667504234211808 ),
 .UNSPECIFIED. ) ;
#25383 = CARTESIAN_POINT ( 'NONE',  ( 350.0000000000000000, 169.0000000000000000, -360.0000000000002274 ) ) ;
#25384 = VERTEX_POINT ( 'NONE', #9685 ) ;
#25385 = DIRECTION ( 'NONE',  ( 0.000000000000000000, 3.186989995019654210E-49, 1.000000000000000000 ) ) ;
#25386 = DIRECTION ( 'NONE',  ( -0.000000000000000000, -0.000000000000000000, -1.000000000000000000 ) ) ;
#25387 = ORIENTED_EDGE ( 'NONE', *, *, #28836, .T. ) ;
#25388 = VERTEX_POINT ( 'NONE', #25339 ) ;
#25389 = ORIENTED_EDGE ( 'NONE', *, *, #38703, .T. ) ;
#25390 = DIRECTION ( 'NONE',  ( -0.000000000000000000, -1.000000000000000000, 2.537652627714643577E-15 ) ) ;
#25391 = LINE ( 'NONE', #13075, #23408 ) ;
#25392 = VERTEX_POINT ( 'NONE', #40989 ) ;
#25393 = AXIS2_PLACEMENT_3D ( 'NONE', #29283, #24438, #21574 ) ;
#25394 = VECTOR ( 'NONE', #41251, 1000.000000000000000 ) ;
#25395 = CARTESIAN_POINT ( 'NONE',  ( 35.05402655318504657, 2.143131898507880377E-16, -77.43171244307198720 ) ) ;
#25396 = PLANE ( 'NONE',  #8234 ) ;
#25397 = FACE_OUTER_BOUND ( 'NONE', #12149, .T. ) ;
#25398 = AXIS2_PLACEMENT_3D ( 'NONE', #50096, #22949, #49596 ) ;
#25399 = CARTESIAN_POINT ( 'NONE',  ( 4.999999999999999112, -175.0000000000000284, 350.0000000000002274 ) ) ;
#25400 = VERTEX_POINT ( 'NONE', #5836 ) ;
#25401 = CARTESIAN_POINT ( 'NONE',  ( 0.9602803029231544718, -0.8490247040095941777, 9.976582533991681601 ) ) ;
#25402 = CARTESIAN_POINT ( 'NONE',  ( 1.151763129092702398, -0.4096856258255446304, 9.987567862361071747 ) ) ;
#25403 = AXIS2_PLACEMENT_3D ( 'NONE', #8488, #24143, #3349 ) ;
#25404 = ADVANCED_FACE ( 'NONE', ( #21478 ), #37167, .F. ) ;
#25405 = CARTESIAN_POINT ( 'NONE',  ( 0.3862712429686894766, -1.188820645368940276, -3.333333333333333481 ) ) ;
#25406 = EDGE_CURVE ( 'NONE', #28419, #3854, #31495, .T. ) ;
#25407 = VERTEX_POINT ( 'NONE', #50142 ) ;
#25409 = CARTESIAN_POINT ( 'NONE',  ( 194.9999999999999432, -173.0000000000000000, 132.0000000000000853 ) ) ;
#25408 = CIRCLE ( 'NONE', #3265, 3.749999999999975575 ) ;
#25410 = DIRECTION ( 'NONE',  ( 0.000000000000000000, -1.000000000000000000, -3.186989995019654210E-49 ) ) ;
#25411 = CARTESIAN_POINT ( 'NONE',  ( -28.96803024440907137, -18.11533787072017176, 7.455576670931136185 ) ) ;
#25412 = CARTESIAN_POINT ( 'NONE',  ( 210.0000000000000568, 0.000000000000000000, -39.18171244307202983 ) ) ;
#25413 = ORIENTED_EDGE ( 'NONE', *, *, #15348, .F. ) ;
#25414 = DIRECTION ( 'NONE',  ( -1.000000000000000000, 0.000000000000000000, 0.000000000000000000 ) ) ;
#25415 = CYLINDRICAL_SURFACE ( 'NONE', #9785, 1.750000000000008438 ) ;
#25416 = CARTESIAN_POINT ( 'NONE',  ( -44.99506233596265048, -23.32283626942287569, 7.455576670931136185 ) ) ;
#25417 = CARTESIAN_POINT ( 'NONE',  ( -0.3862712429686895876, 1.188820645368940720, 10.00000000000000000 ) ) ;
#25418 = LINE ( 'NONE', #9013, #25442 ) ;
#25419 =( BOUNDED_CURVE ( )  B_SPLINE_CURVE ( 3, ( #23570, #8926, #28184, #43813 ),
 .UNSPECIFIED., .F., .F. ) 
 B_SPLINE_CURVE_WITH_KNOTS ( ( 4, 4 ),
 ( 0.000000000000000000, 1.570796326794896558 ),
 .UNSPECIFIED. ) 
 CURVE ( )  GEOMETRIC_REPRESENTATION_ITEM ( )  RATIONAL_B_SPLINE_CURVE ( ( 1.000000000000000000, 0.8047378541243649375, 0.8047378541243649375, 1.000000000000000000 ) ) 
 REPRESENTATION_ITEM ( '' )  );
#25420 = ORIENTED_EDGE ( 'NONE', *, *, #41182, .F. ) ;
#25421 = EDGE_LOOP ( 'NONE', ( #35104, #21322, #4120, #44853 ) ) ;
#25422 = FACE_OUTER_BOUND ( 'NONE', #40779, .T. ) ;
#25423 = ORIENTED_EDGE ( 'NONE', *, *, #13890, .T. ) ;
#25424 = DIRECTION ( 'NONE',  ( -1.000000000000000000, 0.000000000000000000, 0.000000000000000000 ) ) ;
#25425 = CARTESIAN_POINT ( 'NONE',  ( 358.3431457505076310, 165.0000000000000284, 339.9999999999997726 ) ) ;
#25426 =( BOUNDED_CURVE ( )  B_SPLINE_CURVE ( 3, ( #6870, #17894, #29215, #45079 ),
 .UNSPECIFIED., .F., .F. ) 
 B_SPLINE_CURVE_WITH_KNOTS ( ( 4, 4 ),
 ( 0.000000000000000000, 1.570796326794896558 ),
 .UNSPECIFIED. ) 
 CURVE ( )  GEOMETRIC_REPRESENTATION_ITEM ( )  RATIONAL_B_SPLINE_CURVE ( ( 1.000000000000000000, 0.8047378541243649375, 0.8047378541243649375, 1.000000000000000000 ) ) 
 REPRESENTATION_ITEM ( '' )  );
#25427 = AXIS2_PLACEMENT_3D ( 'NONE', #31767, #7912, #42520 ) ;
#25428 = ORIENTED_EDGE ( 'NONE', *, *, #49978, .T. ) ;
#25429 = AXIS2_PLACEMENT_3D ( 'NONE', #17414, #28276, #585 ) ;
#25430 = VECTOR ( 'NONE', #44890, 1000.000000000000000 ) ;
#25431 = DIRECTION ( 'NONE',  ( -0.000000000000000000, -0.000000000000000000, -1.000000000000000000 ) ) ;
#25432 = ORIENTED_EDGE ( 'NONE', *, *, #29025, .F. ) ;
#25433 = DIRECTION ( 'NONE',  ( -1.000000000000000000, 3.172065799423185948E-16, -1.587271980518778491E-16 ) ) ;
#25434 = CARTESIAN_POINT ( 'NONE',  ( 0.9390173899407876501, 1.130417317737878458, 9.958264684458711713 ) ) ;
#25435 = CARTESIAN_POINT ( 'NONE',  ( -166.6959734468149463, 1.750000000000010658, -119.1817124430720440 ) ) ;
#25436 = CARTESIAN_POINT ( 'NONE',  ( -0.4384710792283267322, -1.388197036929783357, 9.938560165450807560 ) ) ;
#25437 = EDGE_CURVE ( 'NONE', #9119, #2781, #7106, .T. ) ;
#25438 = VECTOR ( 'NONE', #6389, 1000.000000000000000 ) ;
#25439 = CYLINDRICAL_SURFACE ( 'NONE', #14847, 1.749999999999987566 ) ;
#25440 = VECTOR ( 'NONE', #39488, 1000.000000000000000 ) ;
#25441 = ORIENTED_EDGE ( 'NONE', *, *, #25495, .F. ) ;
#25442 = VECTOR ( 'NONE', #32618, 1000.000000000000000 ) ;
#25443 = EDGE_LOOP ( 'NONE', ( #35175, #11656, #929, #11830 ) ) ;
#25444 = DIRECTION ( 'NONE',  ( 0.000000000000000000, 0.000000000000000000, 1.000000000000000000 ) ) ;
#25445 = ORIENTED_EDGE ( 'NONE', *, *, #25570, .F. ) ;
#25446 = B_SPLINE_CURVE_WITH_KNOTS ( 'NONE', 3,
 ( #26007, #22899, #27005, #14958 ),
 .UNSPECIFIED., .F., .F.,
 ( 4, 4 ),
 ( 1.734723475976807094E-18, 8.326314924664821488E-06 ),
 .UNSPECIFIED. ) ;
#25447 = CARTESIAN_POINT ( 'NONE',  ( -22.90865447854277193, -29.73489050103202302, -2.490396854064185650 ) ) ;
#25448 = CARTESIAN_POINT ( 'NONE',  ( 40.76831105797779031, 21.94948152812829889, 7.455576670931137073 ) ) ;
#25449 = ORIENTED_EDGE ( 'NONE', *, *, #49405, .T. ) ;
#25450 = LINE ( 'NONE', #2105, #4088 ) ;
#25451 = LINE ( 'NONE', #29302, #50450 ) ;
#25452 = ORIENTED_EDGE ( 'NONE', *, *, #10948, .F. ) ;
#25453 = CARTESIAN_POINT ( 'NONE',  ( 195.0540265531851105, 2.143131898507880377E-16, -77.43171244307204404 ) ) ;
#25454 = CARTESIAN_POINT ( 'NONE',  ( -7.372990760266265653, 0.000000000000000000, 0.000000000000000000 ) ) ;
#25455 = DIRECTION ( 'NONE',  ( -1.000000000000000000, -0.000000000000000000, -0.000000000000000000 ) ) ;
#25456 = CARTESIAN_POINT ( 'NONE',  ( 114.3291528190321173, -1.749999999999996891, 39.79316129108089228 ) ) ;
#25457 = ORIENTED_EDGE ( 'NONE', *, *, #36929, .F. ) ;
#25458 = VERTEX_POINT ( 'NONE', #18878 ) ;
#25459 = FACE_OUTER_BOUND ( 'NONE', #41908, .T. ) ;
#25460 = CARTESIAN_POINT ( 'NONE',  ( -3.694521163055078272, -0.7694713829383514891, 9.865049507598754985 ) ) ;
#25461 = DIRECTION ( 'NONE',  ( 1.000000000000000000, 0.000000000000000000, 0.000000000000000000 ) ) ;
#25462 = DIRECTION ( 'NONE',  ( -0.000000000000000000, -0.000000000000000000, -1.000000000000000000 ) ) ;
#25463 = CARTESIAN_POINT ( 'NONE',  ( -1.158497635116737312, 16.61944452314319420, -3.546734833711462365 ) ) ;
#25464 = EDGE_LOOP ( 'NONE', ( #47345, #29607, #16756, #18480, #30521, #7873 ) ) ;
#25465 = DIRECTION ( 'NONE',  ( -1.000000000000000000, -0.000000000000000000, -0.000000000000000000 ) ) ;
#25466 = EDGE_CURVE ( 'NONE', #19947, #23987, #18630, .T. ) ;
#25468 = ORIENTED_EDGE ( 'NONE', *, *, #44448, .T. ) ;
#25467 = VECTOR ( 'NONE', #37884, 1000.000000000000000 ) ;
#25469 = DIRECTION ( 'NONE',  ( 0.000000000000000000, -0.000000000000000000, 1.000000000000000000 ) ) ;
#25470 = CARTESIAN_POINT ( 'NONE',  ( 1.377509002708426689, -0.6027468487254984408, 9.927319414211227766 ) ) ;
#25471 = AXIS2_PLACEMENT_3D ( 'NONE', #49419, #14305, #3505 ) ;
#25472 = CARTESIAN_POINT ( 'NONE',  ( 210.0000000000000568, 0.000000000000000000, -119.1817124430720440 ) ) ;
#25473 = FACE_OUTER_BOUND ( 'NONE', #21524, .T. ) ;
#25474 = DIRECTION ( 'NONE',  ( -1.000000000000000000, -0.000000000000000000, -0.000000000000000000 ) ) ;
#25475 = ORIENTED_EDGE ( 'NONE', *, *, #41238, .T. ) ;
#25476 = CARTESIAN_POINT ( 'NONE',  ( 72.27890028733797578, -1.750000000000009548, 39.79316129108089228 ) ) ;
#25478 = VECTOR ( 'NONE', #2448, 1000.000000000000000 ) ;
#25477 = CARTESIAN_POINT ( 'NONE',  ( 194.9999999999999432, -172.9999999999999716, 232.0000000000000284 ) ) ;
#25479 = CARTESIAN_POINT ( 'NONE',  ( 181.0000000000000284, -272.5000000000000000, -114.9999999999999147 ) ) ;
#25480 = CARTESIAN_POINT ( 'NONE',  ( 34.08355720199905647, -2.371364769369109116, 7.455576670931136185 ) ) ;
#25481 = ORIENTED_EDGE ( 'NONE', *, *, #50220, .T. ) ;
#25482 = CARTESIAN_POINT ( 'NONE',  ( -1.011271242968688533, 0.7347315653655859258, -3.333333333333333481 ) ) ;
#25483 = ORIENTED_EDGE ( 'NONE', *, *, #42791, .T. ) ;
#25484 = PLANE ( 'NONE',  #36072 ) ;
#25485 = DIRECTION ( 'NONE',  ( 0.000000000000000000, 0.000000000000000000, 1.000000000000000000 ) ) ;
#25486 = CARTESIAN_POINT ( 'NONE',  ( 10.50000000000000178, -46.01315789473684248, -5.916985404131818171 ) ) ;
#25487 = CARTESIAN_POINT ( 'NONE',  ( 46.55190821232867648, -18.53135734581217164, -8.917361510505369182 ) ) ;
#25488 = CARTESIAN_POINT ( 'NONE',  ( -119.9999999999994174, 17.00000000000000000, -54.99999999999999289 ) ) ;
#25489 = CARTESIAN_POINT ( 'NONE',  ( 166.9999999999999716, -268.5000000000000000, -339.9999999999998863 ) ) ;
#25490 = CARTESIAN_POINT ( 'NONE',  ( 0.000000000000000000, 0.000000000000000000, 0.000000000000000000 ) ) ;
#25491 = ADVANCED_FACE ( 'NONE', ( #14282 ), #29947, .F. ) ;
#25492 = ORIENTED_EDGE ( 'NONE', *, *, #15569, .T. ) ;
#25493 = ORIENTED_EDGE ( 'NONE', *, *, #47145, .T. ) ;
#25494 = CYLINDRICAL_SURFACE ( 'NONE', #26709, 1.750000000000008438 ) ;
#25495 = EDGE_CURVE ( 'NONE', #48161, #13105, #29687, .T. ) ;
#25496 = CARTESIAN_POINT ( 'NONE',  ( 28.96803024440893992, 18.11533787072037072, 7.455576670931136185 ) ) ;
#25497 = AXIS2_PLACEMENT_3D ( 'NONE', #17295, #13692, #1903 ) ;
#25498 = EDGE_CURVE ( 'NONE', #25957, #8816, #34437, .T. ) ;
#25499 = ORIENTED_EDGE ( 'NONE', *, *, #6040, .F. ) ;
#25500 = ORIENTED_EDGE ( 'NONE', *, *, #11533, .F. ) ;
#25501 = DIRECTION ( 'NONE',  ( 1.000000000000000000, 0.000000000000000000, 2.958228394578794270E-31 ) ) ;
#25502 = DIRECTION ( 'NONE',  ( -0.000000000000000000, -0.000000000000000000, -1.000000000000000000 ) ) ;
#25503 = DIRECTION ( 'NONE',  ( 0.000000000000000000, 0.000000000000000000, -1.000000000000000000 ) ) ;
#25504 = CARTESIAN_POINT ( 'NONE',  ( -10.50000000000003375, 8.875661936878630698, 18.94832733001756253 ) ) ;
#25505 = ORIENTED_EDGE ( 'NONE', *, *, #26298, .F. ) ;
#25506 = ORIENTED_EDGE ( 'NONE', *, *, #41494, .F. ) ;
#25507 = VECTOR ( 'NONE', #9942, 1000.000000000000000 ) ;
#25508 = EDGE_CURVE ( 'NONE', #13625, #33144, #14025, .T. ) ;
#25509 = EDGE_CURVE ( 'NONE', #38550, #325, #49143, .T. ) ;
#25510 = AXIS2_PLACEMENT_3D ( 'NONE', #47721, #8784, #20568 ) ;
#25511 = EDGE_CURVE ( 'NONE', #36401, #45850, #2641, .T. ) ;
#25512 = CARTESIAN_POINT ( 'NONE',  ( 195.0540265531851105, 2.143131898507880377E-16, 79.06828755692797017 ) ) ;
#25513 = EDGE_LOOP ( 'NONE', ( #24698, #13136, #45275, #4318, #12647, #9473 ) ) ;
#25514 = ORIENTED_EDGE ( 'NONE', *, *, #38085, .F. ) ;
#25515 = DIRECTION ( 'NONE',  ( -1.000000000000000000, -0.000000000000000000, -0.000000000000000000 ) ) ;
#25516 = CARTESIAN_POINT ( 'NONE',  ( 153.3040265531850537, 1.750000000000009992, 0.8182875569279768335 ) ) ;
#25517 = VERTEX_POINT ( 'NONE', #15050 ) ;
#25518 = ADVANCED_FACE ( 'NONE', ( #37662 ), #3954, .T. ) ;
#25519 = EDGE_CURVE ( 'NONE', #29900, #15646, #26352, .T. ) ;
#25520 = ORIENTED_EDGE ( 'NONE', *, *, #49096, .F. ) ;
#25521 = CARTESIAN_POINT ( 'NONE',  ( -4.353119224255007857, -9.002796955359011477, 0.000000000000000000 ) ) ;
#25522 = DIRECTION ( 'NONE',  ( 1.000000000000000000, -0.000000000000000000, 0.000000000000000000 ) ) ;
#25523 = VERTEX_POINT ( 'NONE', #42489 ) ;
#25524 = CARTESIAN_POINT ( 'NONE',  ( -7.574282714737721633, 6.549555713337947616, 3.092310436554648767 ) ) ;
#25525 = EDGE_CURVE ( 'NONE', #37470, #8001, #22494, .T. ) ;
#25526 = DIRECTION ( 'NONE',  ( -1.000000000000000000, -0.000000000000000000, -0.000000000000000000 ) ) ;
#25527 = DIRECTION ( 'NONE',  ( 1.000000000000000000, 0.000000000000000000, 0.000000000000000000 ) ) ;
#25528 = DIRECTION ( 'NONE',  ( 0.000000000000000000, -0.000000000000000000, -1.000000000000000000 ) ) ;
#25529 = EDGE_CURVE ( 'NONE', #12618, #41724, #38170, .T. ) ;
#25530 = LINE ( 'NONE', #26543, #35654 ) ;
#25531 = EDGE_LOOP ( 'NONE', ( #22220, #36721, #39087, #32585 ) ) ;
#25532 = ADVANCED_FACE ( 'NONE', ( #16322 ), #8893, .T. ) ;
#25533 = DIRECTION ( 'NONE',  ( 0.000000000000000000, 0.000000000000000000, 1.000000000000000000 ) ) ;
#25534 = CIRCLE ( 'NONE', #48409, 2.000000000000001776 ) ;
#25535 = EDGE_CURVE ( 'NONE', #25772, #11761, #13138, .T. ) ;
#25536 = CARTESIAN_POINT ( 'NONE',  ( 33.30402655318503946, -1.750000000000010658, -119.1817124430720440 ) ) ;
#25537 = CARTESIAN_POINT ( 'NONE',  ( 73.30402655318508209, 1.750000000000010658, -119.1817124430720440 ) ) ;
#25538 = DIRECTION ( 'NONE',  ( 0.000000000000000000, 0.000000000000000000, -1.000000000000000000 ) ) ;
#25539 = CARTESIAN_POINT ( 'NONE',  ( 5.551115123125782702E-14, -168.9999999999999432, 343.9999999999997726 ) ) ;
#25540 = CARTESIAN_POINT ( 'NONE',  ( -177.4999999999999716, -72.50000000000001421, -9.999999999999973355 ) ) ;
#25541 = CIRCLE ( 'NONE', #28032, 5.000000000000000000 ) ;
#25542 = CARTESIAN_POINT ( 'NONE',  ( 7.576114424932982594, -33.14742743729794938, 7.906207997025717304 ) ) ;
#25543 = CARTESIAN_POINT ( 'NONE',  ( -208.4459734468149463, 0.000000000000000000, 119.0682875569279702 ) ) ;
#25544 = AXIS2_PLACEMENT_3D ( 'NONE', #14949, #50296, #15207 ) ;
#25545 = EDGE_CURVE ( 'NONE', #14624, #40520, #47582, .T. ) ;
#25546 = DIRECTION ( 'NONE',  ( -1.000000000000000000, 0.000000000000000000, -0.000000000000000000 ) ) ;
#25547 = ORIENTED_EDGE ( 'NONE', *, *, #32103, .T. ) ;
#25548 = CARTESIAN_POINT ( 'NONE',  ( 350.0000000000001137, 165.0000000000000000, 355.9999999999997726 ) ) ;
#25549 = EDGE_CURVE ( 'NONE', #47191, #45593, #31477, .T. ) ;
#25550 = ADVANCED_FACE ( 'NONE', ( #12215 ), #3483, .T. ) ;
#25551 = FACE_OUTER_BOUND ( 'NONE', #6517, .T. ) ;
#25552 = DIRECTION ( 'NONE',  ( -1.000000000000000000, -0.000000000000000000, -0.000000000000000000 ) ) ;
#25553 = CARTESIAN_POINT ( 'NONE',  ( -126.6959734468149321, -1.749999999999997113, 40.81828755692798438 ) ) ;
#25554 = CARTESIAN_POINT ( 'NONE',  ( -164.9459734468149463, 2.143131898507880377E-16, 165.0000000000000000 ) ) ;
#25555 = EDGE_CURVE ( 'NONE', #8813, #33254, #16072, .T. ) ;
#25556 = ORIENTED_EDGE ( 'NONE', *, *, #2087, .F. ) ;
#25557 = VERTEX_POINT ( 'NONE', #46816 ) ;
#25558 = CARTESIAN_POINT ( 'NONE',  ( -168.4459734468149463, 0.000000000000000000, -37.43171244307205825 ) ) ;
#25559 = EDGE_CURVE ( 'NONE', #16843, #18731, #39683, .T. ) ;
#25560 = DIRECTION ( 'NONE',  ( -1.000000000000000000, -0.000000000000000000, -0.000000000000000000 ) ) ;
#25561 =( BOUNDED_CURVE ( )  B_SPLINE_CURVE ( 3, ( #47351, #32760, #16603, #9149 ),
 .UNSPECIFIED., .F., .F. ) 
 B_SPLINE_CURVE_WITH_KNOTS ( ( 4, 4 ),
 ( 0.000000000000000000, 1.570796326794931197 ),
 .UNSPECIFIED. ) 
 CURVE ( )  GEOMETRIC_REPRESENTATION_ITEM ( )  RATIONAL_B_SPLINE_CURVE ( ( 1.000000000000000000, 0.8047378541243568328, 0.8047378541243568328, 1.000000000000000000 ) ) 
 REPRESENTATION_ITEM ( '' )  );
#25562 = ORIENTED_EDGE ( 'NONE', *, *, #27738, .T. ) ;
#25563 = CARTESIAN_POINT ( 'NONE',  ( -166.6959734468149463, 1.750000000000010658, 120.8182875569279702 ) ) ;
#25564 = DIRECTION ( 'NONE',  ( -1.000000000000000000, -0.000000000000000000, -0.000000000000000000 ) ) ;
#25565 = ORIENTED_EDGE ( 'NONE', *, *, #32741, .T. ) ;
#25566 = VERTEX_POINT ( 'NONE', #42999 ) ;
#25567 =( BOUNDED_CURVE ( )  B_SPLINE_CURVE ( 3, ( #17878, #49399, #25849, #10950 ),
 .UNSPECIFIED., .F., .F. ) 
 B_SPLINE_CURVE_WITH_KNOTS ( ( 4, 4 ),
 ( 3.141592653589793116, 4.712388980384689674 ),
 .UNSPECIFIED. ) 
 CURVE ( )  GEOMETRIC_REPRESENTATION_ITEM ( )  RATIONAL_B_SPLINE_CURVE ( ( 1.000000000000000000, 0.8047378541243649375, 0.8047378541243649375, 1.000000000000000000 ) ) 
 REPRESENTATION_ITEM ( '' )  );
#25568 = AXIS2_PLACEMENT_3D ( 'NONE', #19456, #35895, #27421 ) ;
#25569 = VERTEX_POINT ( 'NONE', #50409 ) ;
#25570 = EDGE_CURVE ( 'NONE', #30113, #17360, #31227, .T. ) ;
#25571 = CYLINDRICAL_SURFACE ( 'NONE', #6954, 0.5000000000000004441 ) ;
#25572 = CARTESIAN_POINT ( 'NONE',  ( 33.30402655318503946, -1.750000000000010658, 120.8182875569279702 ) ) ;
#25573 = CARTESIAN_POINT ( 'NONE',  ( 5.888214538810389698, 16.20866436362417673, 8.727788335465566760 ) ) ;
#25574 = VERTEX_POINT ( 'NONE', #7878 ) ;
#25575 = FACE_OUTER_BOUND ( 'NONE', #24314, .T. ) ;
#25576 = CIRCLE ( 'NONE', #42769, 4.000000000000003553 ) ;
#25577 = FACE_OUTER_BOUND ( 'NONE', #50223, .T. ) ;
#25578 = CARTESIAN_POINT ( 'NONE',  ( 7.749480817862238524, 14.85497772329518895, 9.403735324607438884 ) ) ;
#25579 = ORIENTED_EDGE ( 'NONE', *, *, #27130, .T. ) ;
#25580 = EDGE_CURVE ( 'NONE', #16448, #20559, #9546, .T. ) ;
#25581 = ORIENTED_EDGE ( 'NONE', *, *, #36530, .T. ) ;
#25582 = CARTESIAN_POINT ( 'NONE',  ( 33.30402655318503946, 0.000000000000000000, 165.0000000000000000 ) ) ;
#25583 = CARTESIAN_POINT ( 'NONE',  ( 112.2789002873379758, -1.749999999999996891, 121.8434138227750481 ) ) ;
#25584 =( BOUNDED_CURVE ( )  B_SPLINE_CURVE ( 3, ( #9936, #9433, #44066, #25098 ),
 .UNSPECIFIED., .F., .F. ) 
 B_SPLINE_CURVE_WITH_KNOTS ( ( 4, 4 ),
 ( 4.712388980384689674, 6.283185307179586232 ),
 .UNSPECIFIED. ) 
 CURVE ( )  GEOMETRIC_REPRESENTATION_ITEM ( )  RATIONAL_B_SPLINE_CURVE ( ( 1.000000000000000000, 0.8047378541243649375, 0.8047378541243649375, 1.000000000000000000 ) ) 
 REPRESENTATION_ITEM ( '' )  );
#25585 = CARTESIAN_POINT ( 'NONE',  ( 113.3040265531850537, 1.749999999999997113, -39.18171244307202983 ) ) ;
#25586 = EDGE_LOOP ( 'NONE', ( #42825, #35048 ) ) ;
#25587 = DIRECTION ( 'NONE',  ( -2.958228394578793832E-31, 0.000000000000000000, -1.000000000000000000 ) ) ;
#25588 = CARTESIAN_POINT ( 'NONE',  ( -85.67084718096784002, -1.750000000000009548, 161.8434138227750907 ) ) ;
#25589 = EDGE_CURVE ( 'NONE', #47273, #30921, #35343, .T. ) ;
#25590 = CARTESIAN_POINT ( 'NONE',  ( 85.00000000000090949, 17.00000000000000000, -24.99999999999999289 ) ) ;
#25591 = EDGE_CURVE ( 'NONE', #37300, #2701, #41812, .T. ) ;
#25592 = CARTESIAN_POINT ( 'NONE',  ( -49.75871208702130133, 40.58472229863599523, 5.000000000000000000 ) ) ;
#25593 = LINE ( 'NONE', #13270, #39868 ) ;
#25594 = ADVANCED_FACE ( 'NONE', ( #43258 ), #425, .T. ) ;
#25595 = CARTESIAN_POINT ( 'NONE',  ( 20.37409433807990666, 26.28007012093483397, -2.408242355805840784 ) ) ;
#25596 = AXIS2_PLACEMENT_3D ( 'NONE', #20080, #35766, #36514 ) ;
#25597 = EDGE_CURVE ( 'NONE', #18727, #10108, #40689, .T. ) ;
#25598 = CARTESIAN_POINT ( 'NONE',  ( -46.69597344681494633, 0.000000000000000000, 165.0000000000000000 ) ) ;
#25599 = LINE ( 'NONE', #21740, #8845 ) ;
#25600 = EDGE_CURVE ( 'NONE', #3985, #37708, #25040, .T. ) ;
#25601 = DIRECTION ( 'NONE',  ( -0.8090169943749507819, 0.5877852522924685852, 0.000000000000000000 ) ) ;
#25602 = DIRECTION ( 'NONE',  ( 0.000000000000000000, 0.000000000000000000, 1.000000000000000000 ) ) ;
#25603 = AXIS2_PLACEMENT_3D ( 'NONE', #36916, #32794, #21228 ) ;
#25604 = ORIENTED_EDGE ( 'NONE', *, *, #6325, .F. ) ;
#25605 = LINE ( 'NONE', #14036, #34384 ) ;
#25606 = AXIS2_PLACEMENT_3D ( 'NONE', #32795, #12775, #40490 ) ;
#25607 = DIRECTION ( 'NONE',  ( -1.000000000000000000, -0.000000000000000000, -0.000000000000000000 ) ) ;
#25608 = CARTESIAN_POINT ( 'NONE',  ( 153.3040265531850537, 1.750000000000010214, 40.81828755692798438 ) ) ;
#25609 = VECTOR ( 'NONE', #50218, 1000.000000000000000 ) ;
#25610 = EDGE_LOOP ( 'NONE', ( #33350, #19190, #21747, #25505 ) ) ;
#25611 = CARTESIAN_POINT ( 'NONE',  ( 154.1026953830863420, 103.0380105690400683, -17.46817021067766973 ) ) ;
#25612 = EDGE_CURVE ( 'NONE', #47251, #34400, #47011, .T. ) ;
#25613 = VECTOR ( 'NONE', #39622, 1000.000000000000000 ) ;
#25614 = CYLINDRICAL_SURFACE ( 'NONE', #830, 1.750000000000015543 ) ;
#25615 = ORIENTED_EDGE ( 'NONE', *, *, #29922, .T. ) ;
#25616 = DIRECTION ( 'NONE',  ( -1.000000000000000000, 0.000000000000000000, -2.958228394578794270E-31 ) ) ;
#25617 = DIRECTION ( 'NONE',  ( 0.000000000000000000, 0.000000000000000000, 1.000000000000000000 ) ) ;
#25618 = CARTESIAN_POINT ( 'NONE',  ( -124.9459734468149463, 2.143131898507847836E-16, 2.568287556927950632 ) ) ;
#25619 = DIRECTION ( 'NONE',  ( 0.000000000000000000, 0.000000000000000000, 1.000000000000000000 ) ) ;
#25620 = ORIENTED_EDGE ( 'NONE', *, *, #8595, .T. ) ;
#25621 = LINE ( 'NONE', #5862, #1154 ) ;
#25622 = B_SPLINE_SURFACE_WITH_KNOTS ( 'NONE', 3, 3, ( 
 ( #46662, #23605, #26947, #19236 ),
 ( #3333, #34927, #4110, #18 ),
 ( #19491, #11815, #47170, #11561 ),
 ( #50501, #30811, #18983, #46415 ) ),
 .UNSPECIFIED., .F., .F., .F.,
 ( 4, 4 ),
 ( 4, 4 ),
 ( 0.000000000000000000, 1.000000000000000000 ),
 ( 0.000000000000000000, 1.000000000000000000 ),
 .UNSPECIFIED. ) ;
#25623 = ORIENTED_EDGE ( 'NONE', *, *, #8632, .T. ) ;
#25624 = ORIENTED_EDGE ( 'NONE', *, *, #45469, .T. ) ;
#25625 = CARTESIAN_POINT ( 'NONE',  ( -4.632259510536085756, 3.749670975867693379, -2.642742795433417058E-16 ) ) ;
#25626 = ORIENTED_EDGE ( 'NONE', *, *, #24264, .F. ) ;
#25627 = LINE ( 'NONE', #42281, #10620 ) ;
#25628 = LINE ( 'NONE', #17169, #47788 ) ;
#25629 =( BOUNDED_CURVE ( )  B_SPLINE_CURVE ( 3, ( #24283, #31737, #31471, #43506 ),
 .UNSPECIFIED., .F., .F. ) 
 B_SPLINE_CURVE_WITH_KNOTS ( ( 4, 4 ),
 ( 3.141592653589793116, 4.712388980384689674 ),
 .UNSPECIFIED. ) 
 CURVE ( )  GEOMETRIC_REPRESENTATION_ITEM ( )  RATIONAL_B_SPLINE_CURVE ( ( 1.000000000000000000, 0.8047378541243649375, 0.8047378541243649375, 1.000000000000000000 ) ) 
 REPRESENTATION_ITEM ( '' )  );
#25630 = ORIENTED_EDGE ( 'NONE', *, *, #43141, .T. ) ;
#25631 = PLANE ( 'NONE',  #32819 ) ;
#25632 = EDGE_CURVE ( 'NONE', #50040, #50273, #36093, .T. ) ;
#25633 = CARTESIAN_POINT ( 'NONE',  ( -4.945973446814916130, -1.025126265847097207, -77.43171244307197298 ) ) ;
#25634 = CIRCLE ( 'NONE', #20720, 4.000000000000003553 ) ;
#25635 = CARTESIAN_POINT ( 'NONE',  ( 169.0000000000000284, 165.0000000000000000, 359.9999999999997726 ) ) ;
#25636 = VERTEX_POINT ( 'NONE', #935 ) ;
#25637 = CARTESIAN_POINT ( 'NONE',  ( -210.0000000000000568, 2.143131898507890731E-16, -160.9317124430720298 ) ) ;
#25638 = DIRECTION ( 'NONE',  ( 1.000000000000000000, 0.000000000000000000, 2.958228394578794270E-31 ) ) ;
#25639 = FACE_OUTER_BOUND ( 'NONE', #21154, .T. ) ;
#25640 = ORIENTED_EDGE ( 'NONE', *, *, #31719, .T. ) ;
#25641 = DIRECTION ( 'NONE',  ( -7.793956916774525800E-48, 0.000000000000000000, -1.000000000000000000 ) ) ;
#25642 = DIRECTION ( 'NONE',  ( 1.000000000000000000, 0.000000000000000000, 0.000000000000000000 ) ) ;
#25643 = ORIENTED_EDGE ( 'NONE', *, *, #29415, .F. ) ;
#25644 = ORIENTED_EDGE ( 'NONE', *, *, #40091, .F. ) ;
#25645 = EDGE_LOOP ( 'NONE', ( #270, #32615, #12598, #44602 ) ) ;
#25646 = DIRECTION ( 'NONE',  ( 0.000000000000000000, 0.000000000000000000, -1.000000000000000000 ) ) ;
#25647 = AXIS2_PLACEMENT_3D ( 'NONE', #12093, #8245, #4650 ) ;
#25648 = DIRECTION ( 'NONE',  ( 0.000000000000000000, 0.000000000000000000, 1.000000000000000000 ) ) ;
#25649 = ORIENTED_EDGE ( 'NONE', *, *, #25237, .F. ) ;
#25650 = VECTOR ( 'NONE', #1701, 1000.000000000000000 ) ;
#25651 = CARTESIAN_POINT ( 'NONE',  ( 210.0000000000000568, 0.000000000000000000, 160.8182875569279702 ) ) ;
#25652 = CARTESIAN_POINT ( 'NONE',  ( 85.00000000000152056, 17.00000000000000000, 35.00000000000000000 ) ) ;
#25653 = CARTESIAN_POINT ( 'NONE',  ( 25.60949810002064098, 43.19700938445193827, 1.847720168420772691 ) ) ;
#25654 = ADVANCED_FACE ( 'NONE', ( #32730 ), #16576, .T. ) ;
#25655 = CARTESIAN_POINT ( 'NONE',  ( 113.3040265531850537, 1.749999999999997113, 40.81828755692798438 ) ) ;
#25656 = ADVANCED_FACE ( 'NONE', ( #12717 ), #44254, .T. ) ;
#25657 = VECTOR ( 'NONE', #29327, 1000.000000000000000 ) ;
#25658 = ORIENTED_EDGE ( 'NONE', *, *, #14350, .T. ) ;
#25659 = LINE ( 'NONE', #13335, #1569 ) ;
#25660 = CARTESIAN_POINT ( 'NONE',  ( -0.8285222815141961572, -1.889008401827320771, 9.886433018048073507 ) ) ;
#25661 = EDGE_CURVE ( 'NONE', #38870, #31478, #33253, .T. ) ;
#25662 = CARTESIAN_POINT ( 'NONE',  ( 0.3862712429686894766, -1.188820645368940276, 3.333333333333333481 ) ) ;
#25663 = ORIENTED_EDGE ( 'NONE', *, *, #39322, .F. ) ;
#25664 = EDGE_CURVE ( 'NONE', #36853, #27926, #32187, .T. ) ;
#25665 = EDGE_CURVE ( 'NONE', #11965, #34244, #28381, .T. ) ;
#25666 = LINE ( 'NONE', #22305, #7709 ) ;
#25667 = CARTESIAN_POINT ( 'NONE',  ( -1.011271242968677875, -0.7347315653656004697, 10.00000000000000000 ) ) ;
#25668 =( BOUNDED_CURVE ( )  B_SPLINE_CURVE ( 3, ( #22756, #38428, #18891, #34570 ),
 .UNSPECIFIED., .F., .F. ) 
 B_SPLINE_CURVE_WITH_KNOTS ( ( 4, 4 ),
 ( 3.141592653589793560, 4.712388980384731418 ),
 .UNSPECIFIED. ) 
 CURVE ( )  GEOMETRIC_REPRESENTATION_ITEM ( )  RATIONAL_B_SPLINE_CURVE ( ( 1.000000000000000000, 0.8047378541243551675, 0.8047378541243551675, 1.000000000000000000 ) ) 
 REPRESENTATION_ITEM ( '' )  );
#25669 = CARTESIAN_POINT ( 'NONE',  ( -1.962558162477761714, 3.366505435501197407, 9.741991644046970933 ) ) ;
#25670 = DIRECTION ( 'NONE',  ( 0.000000000000000000, 0.000000000000000000, 1.000000000000000000 ) ) ;
#25671 = ORIENTED_EDGE ( 'NONE', *, *, #23201, .F. ) ;
#25672 = DIRECTION ( 'NONE',  ( -1.000000000000000000, 0.000000000000000000, 0.000000000000000000 ) ) ;
#25673 = CARTESIAN_POINT ( 'NONE',  ( 12.78770032058947237, 31.68259716188277864, 7.455576670931136185 ) ) ;
#25674 = ADVANCED_FACE ( 'NONE', ( #16829 ), #29135, .T. ) ;
#25675 = CARTESIAN_POINT ( 'NONE',  ( -46.10908423965022251, -19.89422939639105437, 1.847720168420772691 ) ) ;
#25676 = CARTESIAN_POINT ( 'NONE',  ( 0.000000000000000000, 165.0000000000000000, -344.0000000000001705 ) ) ;
#25677 = ORIENTED_EDGE ( 'NONE', *, *, #20285, .T. ) ;
#25678 = CARTESIAN_POINT ( 'NONE',  ( 168.9999999999999716, -184.9999999999999716, -358.0000000000001705 ) ) ;
#25679 = ORIENTED_EDGE ( 'NONE', *, *, #1141, .T. ) ;
#25680 = CARTESIAN_POINT ( 'NONE',  ( -1.249999999999999778, 0.000000000000000000, 10.00000000000000000 ) ) ;
#25681 = VECTOR ( 'NONE', #30214, 1000.000000000000000 ) ;
#25682 = B_SPLINE_CURVE_WITH_KNOTS ( 'NONE', 3,
 ( #18487, #18953, #42559, #34635, #3561, #50209 ),
 .UNSPECIFIED., .F., .F.,
 ( 4, 2, 4 ),
 ( 5.818439421673296370E-18, 0.009877169331704830149, 0.01975433866340965683 ),
 .UNSPECIFIED. ) ;
#25683 = EDGE_LOOP ( 'NONE', ( #30108, #23260, #43676, #6060, #3747, #30934 ) ) ;
#25684 = CARTESIAN_POINT ( 'NONE',  ( -164.9459734468149463, 2.143131898507880377E-16, 165.0000000000000000 ) ) ;
#25685 = CARTESIAN_POINT ( 'NONE',  ( -204.9459734468149463, 2.143131898507880377E-16, -120.9317124430720156 ) ) ;
#25686 = DIRECTION ( 'NONE',  ( 0.000000000000000000, 0.000000000000000000, 1.000000000000000000 ) ) ;
#25687 = EDGE_LOOP ( 'NONE', ( #23809, #36383, #17663, #41971 ) ) ;
#25688 = LINE ( 'NONE', #37509, #33281 ) ;
#25689 = VECTOR ( 'NONE', #30786, 1000.000000000000000 ) ;
#25690 = ORIENTED_EDGE ( 'NONE', *, *, #4635, .T. ) ;
#25691 = CARTESIAN_POINT ( 'NONE',  ( 168.9999999999999716, 10.00000000000006395, -340.0000000000001137 ) ) ;
#25692 = CARTESIAN_POINT ( 'NONE',  ( -0.4402948852767746279, 2.015117899693936732, 9.894754715216722118 ) ) ;
#25693 = DIRECTION ( 'NONE',  ( 1.000000000000000000, 0.000000000000000000, -0.000000000000000000 ) ) ;
#25694 = CARTESIAN_POINT ( 'NONE',  ( 210.0000000000000568, 0.000000000000000000, -39.18171244307202983 ) ) ;
#25695 = CARTESIAN_POINT ( 'NONE',  ( 71.55402655318505367, 0.000000000000000000, -40.93171244307205825 ) ) ;
#25696 = ORIENTED_EDGE ( 'NONE', *, *, #44301, .F. ) ;
#25697 = ORIENTED_EDGE ( 'NONE', *, *, #8762, .T. ) ;
#25698 = CARTESIAN_POINT ( 'NONE',  ( 35.05402655318504657, 2.143131898507880377E-16, -80.93171244307204404 ) ) ;
#25699 = EDGE_CURVE ( 'NONE', #46387, #19943, #40424, .T. ) ;
#25700 = ORIENTED_EDGE ( 'NONE', *, *, #43066, .F. ) ;
#25701 = CARTESIAN_POINT ( 'NONE',  ( -5.000000000000000000, 184.8000000000000114, 340.1999999999997044 ) ) ;
#25702 = CARTESIAN_POINT ( 'NONE',  ( 85.00000000000213163, 17.00000000000000000, 115.0000000000000142 ) ) ;
#25703 = ORIENTED_EDGE ( 'NONE', *, *, #28449, .T. ) ;
#25704 = CARTESIAN_POINT ( 'NONE',  ( 153.3040265531850537, -1.750000000000010658, -119.1817124430720440 ) ) ;
#25705 = CYLINDRICAL_SURFACE ( 'NONE', #42291, 1.750000000000015543 ) ;
#25706 = ORIENTED_EDGE ( 'NONE', *, *, #11712, .F. ) ;
#25707 = CARTESIAN_POINT ( 'NONE',  ( -4.945973446814917018, -1.025126265847096985, -160.9317124430720014 ) ) ;
#25708 = DIRECTION ( 'NONE',  ( 0.000000000000000000, 0.000000000000000000, 1.000000000000000000 ) ) ;
#25709 = CARTESIAN_POINT ( 'NONE',  ( -46.69597344681494633, -1.750000000000009992, -159.1817124430720298 ) ) ;
#25710 = CARTESIAN_POINT ( 'NONE',  ( 341.6568542494922553, 185.0000000000002558, -360.0000000000003411 ) ) ;
#25711 = CARTESIAN_POINT ( 'NONE',  ( -9.643172164747307207, 0.000000000000000000, -5.000000000000000000 ) ) ;
#25712 = ORIENTED_EDGE ( 'NONE', *, *, #30270, .T. ) ;
#25713 = VERTEX_POINT ( 'NONE', #24527 ) ;
#25714 = AXIS2_PLACEMENT_3D ( 'NONE', #23666, #43656, #43407 ) ;
#25715 = ORIENTED_EDGE ( 'NONE', *, *, #3891, .F. ) ;
#25716 = CARTESIAN_POINT ( 'NONE',  ( 85.00000000000123634, 17.00000000000000000, 5.000000000000004441 ) ) ;
#25717 = AXIS2_PLACEMENT_3D ( 'NONE', #17810, #1918, #33477 ) ;
#25718 = CARTESIAN_POINT ( 'NONE',  ( -128.4459734468149179, 0.000000000000000000, -0.9317124430719969652 ) ) ;
#25719 = CARTESIAN_POINT ( 'NONE',  ( 360.0000000000000000, -168.9999999999999432, 343.9999999999998295 ) ) ;
#25720 = EDGE_LOOP ( 'NONE', ( #32202, #38795, #37707 ) ) ;
#25721 = VECTOR ( 'NONE', #39518, 1000.000000000000227 ) ;
#25722 = CARTESIAN_POINT ( 'NONE',  ( -194.9999999999999432, 173.0000000000000000, 231.9999999999999716 ) ) ;
#25723 = EDGE_LOOP ( 'NONE', ( #40924, #32757, #7527, #11038 ) ) ;
#25724 =( NAMED_UNIT ( * ) PLANE_ANGLE_UNIT ( ) SI_UNIT ( $, .RADIAN. ) );
#25725 = VECTOR ( 'NONE', #3306, 1000.000000000000000 ) ;
#25726 = EDGE_CURVE ( 'NONE', #13539, #23942, #37440, .T. ) ;
#25727 = CARTESIAN_POINT ( 'NONE',  ( 74.32915281903215998, 1.750000000000010214, -120.2068387089191219 ) ) ;
#25728 =( BOUNDED_CURVE ( )  B_SPLINE_CURVE ( 3, ( #2543, #32862, #5631, #13331 ),
 .UNSPECIFIED., .F., .F. ) 
 B_SPLINE_CURVE_WITH_KNOTS ( ( 4, 4 ),
 ( 4.712388980384689674, 6.283185307179586232 ),
 .UNSPECIFIED. ) 
 CURVE ( )  GEOMETRIC_REPRESENTATION_ITEM ( )  RATIONAL_B_SPLINE_CURVE ( ( 1.000000000000000000, 0.8047378541243649375, 0.8047378541243649375, 1.000000000000000000 ) ) 
 REPRESENTATION_ITEM ( '' )  );
#25729 = DIRECTION ( 'NONE',  ( 0.000000000000000000, 0.000000000000000000, -1.000000000000000000 ) ) ;
#25730 = CYLINDRICAL_SURFACE ( 'NONE', #20100, 2.000000000000001776 ) ;
#25731 = CARTESIAN_POINT ( 'NONE',  ( 151.5540265531850537, 0.000000000000000000, 165.0000000000000000 ) ) ;
#25732 = CARTESIAN_POINT ( 'NONE',  ( -8.445973446814976526, 0.000000000000000000, 159.0682875569279418 ) ) ;
#25733 = ORIENTED_EDGE ( 'NONE', *, *, #12567, .T. ) ;
#25734 = EDGE_CURVE ( 'NONE', #12204, #4741, #5776, .T. ) ;
#25735 = DIRECTION ( 'NONE',  ( 1.156482317317870492E-16, -1.000000000000000000, -0.000000000000000000 ) ) ;
#25736 =( BOUNDED_CURVE ( )  B_SPLINE_CURVE ( 3, ( #16920, #48159, #43844, #28213 ),
 .UNSPECIFIED., .F., .F. ) 
 B_SPLINE_CURVE_WITH_KNOTS ( ( 4, 4 ),
 ( 0.000000000000000000, 1.570796326794896780 ),
 .UNSPECIFIED. ) 
 CURVE ( )  GEOMETRIC_REPRESENTATION_ITEM ( )  RATIONAL_B_SPLINE_CURVE ( ( 1.000000000000000000, 0.8047378541243649375, 0.8047378541243649375, 1.000000000000000000 ) ) 
 REPRESENTATION_ITEM ( '' )  );
#25737 = B_SPLINE_SURFACE_WITH_KNOTS ( 'NONE', 3, 3, ( 
 ( #1137, #20622, #16773, #32438 ),
 ( #2618, #17529, #5976, #6478 ),
 ( #29836, #9579, #21890, #32949 ),
 ( #37057, #25480, #33943, #49531 ) ),
 .UNSPECIFIED., .F., .F., .F.,
 ( 4, 4 ),
 ( 4, 4 ),
 ( 0.000000000000000000, 1.000000000000000000 ),
 ( 0.000000000000000000, 1.000000000000000000 ),
 .UNSPECIFIED. ) ;
#25738 = LINE ( 'NONE', #37803, #17082 ) ;
#25739 = CARTESIAN_POINT ( 'NONE',  ( -167.7210997126620384, -1.750000000000010214, -78.15658617722490931 ) ) ;
#25740 = CYLINDRICAL_SURFACE ( 'NONE', #7674, 1.750000000000008438 ) ;
#25741 = ORIENTED_EDGE ( 'NONE', *, *, #27562, .T. ) ;
#25742 = CARTESIAN_POINT ( 'NONE',  ( -46.76852358249001895, 17.86468378716740801, -9.367992836599951190 ) ) ;
#25743 = ORIENTED_EDGE ( 'NONE', *, *, #42446, .F. ) ;
#25744 = CARTESIAN_POINT ( 'NONE',  ( -119.9999999999994174, 17.00000000000000000, -54.99999999999999289 ) ) ;
#25745 = DIRECTION ( 'NONE',  ( 1.000000000000000000, 0.000000000000000000, -0.000000000000000000 ) ) ;
#25746 = PLANE ( 'NONE',  #20601 ) ;
#25747 = CARTESIAN_POINT ( 'NONE',  ( 15.15373036401913787, -7.214190911380954141, -9.233365092205394475 ) ) ;
#25748 = ORIENTED_EDGE ( 'NONE', *, *, #1117, .F. ) ;
#25749 = AXIS2_PLACEMENT_3D ( 'NONE', #41337, #29534, #9773 ) ;
#25750 = CARTESIAN_POINT ( 'NONE',  ( 33.14391172085757375, 37.72293746533119929, -8.016098858316199838 ) ) ;
#25751 = CIRCLE ( 'NONE', #42947, 2.000000000000001776 ) ;
#25752 = FACE_OUTER_BOUND ( 'NONE', #43804, .T. ) ;
#25753 = CARTESIAN_POINT ( 'NONE',  ( -166.6959734468149463, -1.750000000000010658, 80.81828755692798438 ) ) ;
#25754 = ORIENTED_EDGE ( 'NONE', *, *, #30354, .F. ) ;
#25755 = VERTEX_POINT ( 'NONE', #48074 ) ;
#25756 = CARTESIAN_POINT ( 'NONE',  ( -30.64276258327282321, -34.28040101195678346, -8.016098858316205167 ) ) ;
#25757 = VECTOR ( 'NONE', #40293, 1000.000000000000000 ) ;
#25758 = CARTESIAN_POINT ( 'NONE',  ( 14.86945752723346637, 7.944783388879009145, 2.590526750877053086 ) ) ;
#25759 = EDGE_CURVE ( 'NONE', #23523, #13148, #21009, .T. ) ;
#25760 = VERTEX_POINT ( 'NONE', #1935 ) ;
#25761 = ORIENTED_EDGE ( 'NONE', *, *, #21424, .T. ) ;
#25762 = CARTESIAN_POINT ( 'NONE',  ( 73.30402655318508209, -1.750000000000009992, 160.8182875569279702 ) ) ;
#25763 = CARTESIAN_POINT ( 'NONE',  ( -210.0000000000000568, 0.000000000000000000, -77.43171244307200141 ) ) ;
#25764 = DIRECTION ( 'NONE',  ( -0.000000000000000000, -0.000000000000000000, -1.000000000000000000 ) ) ;
#25765 = ORIENTED_EDGE ( 'NONE', *, *, #13352, .F. ) ;
#25766 = CARTESIAN_POINT ( 'NONE',  ( -206.6959734468149463, 0.000000000000000000, 165.0000000000000000 ) ) ;
#25767 = VERTEX_POINT ( 'NONE', #48833 ) ;
#25768 = CARTESIAN_POINT ( 'NONE',  ( 15.00000000000000000, -46.12433806312137108, 6.404467680894761372 ) ) ;
#25769 = DIRECTION ( 'NONE',  ( 0.000000000000000000, -0.000000000000000000, -1.000000000000000000 ) ) ;
#25770 = VECTOR ( 'NONE', #14221, 1000.000000000000000 ) ;
#25771 = VERTEX_POINT ( 'NONE', #29380 ) ;
#25772 = VERTEX_POINT ( 'NONE', #8630 ) ;
#25773 = AXIS2_PLACEMENT_3D ( 'NONE', #35534, #124, #8327 ) ;
#25774 = CARTESIAN_POINT ( 'NONE',  ( -164.9459734468149463, 2.143131898507880377E-16, -0.9317124430720247208 ) ) ;
#25775 = DIRECTION ( 'NONE',  ( 1.000000000000000000, 0.000000000000000000, -0.000000000000000000 ) ) ;
#25776 = VERTEX_POINT ( 'NONE', #24287 ) ;
#25777 = CARTESIAN_POINT ( 'NONE',  ( 341.9999999999999432, -169.0000000000001137, -349.9999999999998863 ) ) ;
#25778 = VERTEX_POINT ( 'NONE', #20410 ) ;
#25779 = CARTESIAN_POINT ( 'NONE',  ( 340.0000000000000568, 185.0000000000000284, 349.9999999999998295 ) ) ;
#25780 = DIRECTION ( 'NONE',  ( 0.000000000000000000, 0.000000000000000000, -1.000000000000000000 ) ) ;
#25781 = ORIENTED_EDGE ( 'NONE', *, *, #45534, .F. ) ;
#25782 = CYLINDRICAL_SURFACE ( 'NONE', #8652, 1.750000000000036193 ) ;
#25783 = CARTESIAN_POINT ( 'NONE',  ( -214.9999999999999432, 173.0000000000000000, 132.0000000000000000 ) ) ;
#25784 = CARTESIAN_POINT ( 'NONE',  ( 183.0000000000000000, -174.9999999999999716, -356.0000000000001705 ) ) ;
#25785 = CARTESIAN_POINT ( 'NONE',  ( 10.00000000000000000, -250.0000000000000000, -224.9999999999999716 ) ) ;
#25786 = VECTOR ( 'NONE', #6889, 1000.000000000000000 ) ;
#25787 = CARTESIAN_POINT ( 'NONE',  ( 72.27890028733797578, 1.750000000000009548, -0.2068387089191121020 ) ) ;
#25788 = ORIENTED_EDGE ( 'NONE', *, *, #6863, .F. ) ;
#25789 = EDGE_CURVE ( 'NONE', #20648, #16490, #25530, .T. ) ;
#25790 = CARTESIAN_POINT ( 'NONE',  ( -208.4459734468148611, 1.025126265847089213, 42.56828755692799149 ) ) ;
#25791 = DIRECTION ( 'NONE',  ( -1.000000000000000000, 0.000000000000000000, 0.000000000000000000 ) ) ;
#25792 = CARTESIAN_POINT ( 'NONE',  ( -24.47767542868268364, 23.18653802921800278, 8.807470649214879543 ) ) ;
#25793 = PLANE ( 'NONE',  #1206 ) ;
#25794 = AXIS2_PLACEMENT_3D ( 'NONE', #35583, #15808, #30969 ) ;
#25795 = CARTESIAN_POINT ( 'NONE',  ( 36.08557433729230013, -35.58569447144767395, 7.455576670931136185 ) ) ;
#25796 = DIRECTION ( 'NONE',  ( 0.000000000000000000, 0.000000000000000000, 1.000000000000000000 ) ) ;
#25797 = CARTESIAN_POINT ( 'NONE',  ( -1.249999999999999778, 0.000000000000000000, 10.00000000000000000 ) ) ;
#25798 = EDGE_CURVE ( 'NONE', #12438, #16264, #49332, .T. ) ;
#25799 = FACE_OUTER_BOUND ( 'NONE', #38226, .T. ) ;
#25800 = CARTESIAN_POINT ( 'NONE',  ( -168.4459734468149747, 1.025126265847089435, 122.5682875569280128 ) ) ;
#25801 = EDGE_CURVE ( 'NONE', #25772, #44745, #49505, .T. ) ;
#25802 = EDGE_CURVE ( 'NONE', #34395, #43947, #45249, .T. ) ;
#25803 = ORIENTED_EDGE ( 'NONE', *, *, #5184, .F. ) ;
#25804 = CARTESIAN_POINT ( 'NONE',  ( 21.61731705588930552, 25.43568671410602278, -9.367992836599951190 ) ) ;
#25805 = VECTOR ( 'NONE', #9960, 1000.000000000000000 ) ;
#25806 = CARTESIAN_POINT ( 'NONE',  ( -28.96803024440907137, -18.11533787072017176, 7.455576670931136185 ) ) ;
#25807 = AXIS2_PLACEMENT_3D ( 'NONE', #29332, #17780, #5716 ) ;
#25808 = CYLINDRICAL_SURFACE ( 'NONE', #5694, 1.750000000000001554 ) ;
#25809 = CARTESIAN_POINT ( 'NONE',  ( -204.9459734468148895, -1.025126265847089213, -160.9317124430720014 ) ) ;
#25810 = CARTESIAN_POINT ( 'NONE',  ( -45.67084718096785423, -1.750000000000009548, -38.15658617722494483 ) ) ;
#25811 = VERTEX_POINT ( 'NONE', #6022 ) ;
#25812 = EDGE_CURVE ( 'NONE', #2324, #27056, #21937, .T. ) ;
#25814 = ORIENTED_EDGE ( 'NONE', *, *, #9185, .T. ) ;
#25813 = EDGE_CURVE ( 'NONE', #5419, #7227, #22687, .T. ) ;
#25815 = LINE ( 'NONE', #22461, #7040 ) ;
#25816 = CARTESIAN_POINT ( 'NONE',  ( 210.0000000000000568, 0.000000000000000000, 82.56828755692799859 ) ) ;
#25817 = EDGE_CURVE ( 'NONE', #42182, #3066, #29884, .T. ) ;
#25818 = EDGE_CURVE ( 'NONE', #31470, #27168, #11856, .T. ) ;
#25819 = ORIENTED_EDGE ( 'NONE', *, *, #15761, .F. ) ;
#25820 = CARTESIAN_POINT ( 'NONE',  ( 3.229232847726260403, -16.57333684275945629, 9.178419661560148768 ) ) ;
#25821 = DIRECTION ( 'NONE',  ( 0.000000000000000000, 0.000000000000000000, -1.000000000000000000 ) ) ;
#25822 = VECTOR ( 'NONE', #23575, 1000.000000000000000 ) ;
#25823 = ORIENTED_EDGE ( 'NONE', *, *, #49816, .T. ) ;
#25824 = ORIENTED_EDGE ( 'NONE', *, *, #39649, .F. ) ;
#25825 = ORIENTED_EDGE ( 'NONE', *, *, #27233, .T. ) ;
#25826 = VECTOR ( 'NONE', #11526, 1000.000000000000000 ) ;
#25827 = DIRECTION ( 'NONE',  ( -0.000000000000000000, -0.000000000000000000, -1.000000000000000000 ) ) ;
#25828 = LINE ( 'NONE', #25317, #7879 ) ;
#25829 = CARTESIAN_POINT ( 'NONE',  ( 357.9999999999999432, -181.0000000000001421, -349.9999999999999432 ) ) ;
#25830 = ORIENTED_EDGE ( 'NONE', *, *, #49351, .T. ) ;
#25831 = CARTESIAN_POINT ( 'NONE',  ( -10.00000000000000000, 0.000000000000000000, 10.00000000000000000 ) ) ;
#25832 = CARTESIAN_POINT ( 'NONE',  ( 210.0000000000000568, 0.000000000000000000, 120.8182875569279702 ) ) ;
#25833 = FACE_OUTER_BOUND ( 'NONE', #46266, .T. ) ;
#25834 = EDGE_LOOP ( 'NONE', ( #33926, #32596, #42145, #33739 ) ) ;
#25835 = ORIENTED_EDGE ( 'NONE', *, *, #45038, .F. ) ;
#25836 = LINE ( 'NONE', #45552, #29533 ) ;
#25837 = CARTESIAN_POINT ( 'NONE',  ( -0.3862712429686809279, -1.188820645368943163, 10.00000000000000000 ) ) ;
#25838 = VERTEX_POINT ( 'NONE', #41939 ) ;
#25839 = EDGE_CURVE ( 'NONE', #30626, #40517, #33496, .T. ) ;
#25840 = CARTESIAN_POINT ( 'NONE',  ( -15.00000000000001421, 17.00000000000000000, -90.00000000000000000 ) ) ;
#25841 = EDGE_CURVE ( 'NONE', #42641, #23796, #49206, .T. ) ;
#25842 = DIRECTION ( 'NONE',  ( 0.000000000000000000, 0.000000000000000000, -1.000000000000000000 ) ) ;
#25843 = DIRECTION ( 'NONE',  ( 0.000000000000000000, -0.000000000000000000, 1.000000000000000000 ) ) ;
#25844 = EDGE_CURVE ( 'NONE', #20358, #18930, #41433, .T. ) ;
#25845 = DIRECTION ( 'NONE',  ( 0.000000000000000000, 1.000000000000000000, 7.004339610132985974E-48 ) ) ;
#25846 = AXIS2_PLACEMENT_3D ( 'NONE', #24821, #5310, #35879 ) ;
#25847 = LINE ( 'NONE', #42491, #40580 ) ;
#25848 = EDGE_CURVE ( 'NONE', #18366, #9801, #5342, .T. ) ;
#25849 = CARTESIAN_POINT ( 'NONE',  ( 114.3291528190321173, -1.749999999999996225, 1.843413822775058497 ) ) ;
#25850 = DIRECTION ( 'NONE',  ( -0.000000000000000000, -0.000000000000000000, -1.000000000000000000 ) ) ;
#25851 = CARTESIAN_POINT ( 'NONE',  ( 168.9999999999999716, 175.0000000000000284, -342.0000000000001137 ) ) ;
#25852 = EDGE_CURVE ( 'NONE', #18024, #49373, #18076, .T. ) ;
#25853 = DIRECTION ( 'NONE',  ( -0.000000000000000000, -1.000000000000000000, -0.000000000000000000 ) ) ;
#25854 = CIRCLE ( 'NONE', #15197, 1.750000000000015543 ) ;
#25855 =( GEOMETRIC_REPRESENTATION_CONTEXT ( 3 ) GLOBAL_UNCERTAINTY_ASSIGNED_CONTEXT ( ( #35235 ) ) GLOBAL_UNIT_ASSIGNED_CONTEXT ( ( #32936, #16760, #40861 ) ) REPRESENTATION_CONTEXT ( 'NONE', 'WORKASPACE' ) );
#25856 = ORIENTED_EDGE ( 'NONE', *, *, #3888, .T. ) ;
#25857 = FACE_BOUND ( 'NONE', #10003, .T. ) ;
#25858 = CARTESIAN_POINT ( 'NONE',  ( 0.9989200098981507736, 1.123829893718967687, 9.927319414211233095 ) ) ;
#25859 = VECTOR ( 'NONE', #46321, 1000.000000000000000 ) ;
#25860 = CARTESIAN_POINT ( 'NONE',  ( 154.3291528190321458, 1.750000000000010214, -120.2068387089191219 ) ) ;
#25861 =( BOUNDED_CURVE ( )  B_SPLINE_CURVE ( 3, ( #22851, #2837, #42351, #18235 ),
 .UNSPECIFIED., .F., .F. ) 
 B_SPLINE_CURVE_WITH_KNOTS ( ( 4, 4 ),
 ( 3.141592653589793116, 4.712388980384689674 ),
 .UNSPECIFIED. ) 
 CURVE ( )  GEOMETRIC_REPRESENTATION_ITEM ( )  RATIONAL_B_SPLINE_CURVE ( ( 1.000000000000000000, 0.8047378541243649375, 0.8047378541243649375, 1.000000000000000000 ) ) 
 REPRESENTATION_ITEM ( '' )  );
#25862 = ORIENTED_EDGE ( 'NONE', *, *, #5504, .F. ) ;
#25863 = SURFACE_SIDE_STYLE ('',( #34845 ) ) ;
#25864 = CARTESIAN_POINT ( 'NONE',  ( 153.3040265531850537, 1.750000000000010214, -39.18171244307202983 ) ) ;
#25865 = ADVANCED_FACE ( 'NONE', ( #10392 ), #6532, .F. ) ;
#25866 = EDGE_LOOP ( 'NONE', ( #1361, #9455, #274, #7961 ) ) ;
#25867 = FACE_OUTER_BOUND ( 'NONE', #35709, .T. ) ;
#25868 = FACE_OUTER_BOUND ( 'NONE', #9794, .T. ) ;
#25869 = CARTESIAN_POINT ( 'NONE',  ( 7.726417830024686850, -6.396462539501553302, 9.390253821402620105 ) ) ;
#25870 = CARTESIAN_POINT ( 'NONE',  ( -7.822422304254325276, 7.611558401714507482, 229.0000000000000000 ) ) ;
#25871 =( BOUNDED_CURVE ( )  B_SPLINE_CURVE ( 3, ( #22563, #38248, #3059, #49967 ),
 .UNSPECIFIED., .F., .F. ) 
 B_SPLINE_CURVE_WITH_KNOTS ( ( 4, 4 ),
 ( 0.000000000000000000, 1.570796326794896558 ),
 .UNSPECIFIED. ) 
 CURVE ( )  GEOMETRIC_REPRESENTATION_ITEM ( )  RATIONAL_B_SPLINE_CURVE ( ( 1.000000000000000000, 0.8047378541243649375, 0.8047378541243649375, 1.000000000000000000 ) ) 
 REPRESENTATION_ITEM ( '' )  );
#25872 = ORIENTED_EDGE ( 'NONE', *, *, #46859, .T. ) ;
#25873 = CARTESIAN_POINT ( 'NONE',  ( -0.4401267517937272333, 2.015194695084603360, 9.889206916986893248 ) ) ;
#25874 = EDGE_CURVE ( 'NONE', #7258, #6011, #26295, .T. ) ;
#25876 = ORIENTED_EDGE ( 'NONE', *, *, #35600, .F. ) ;
#25875 = EDGE_CURVE ( 'NONE', #35538, #6064, #36844, .T. ) ;
#25877 = EDGE_LOOP ( 'NONE', ( #15334, #32870, #18486, #17119 ) ) ;
#25878 = CYLINDRICAL_SURFACE ( 'NONE', #31192, 2.000000000000001776 ) ;
#25879 = EDGE_CURVE ( 'NONE', #12765, #8645, #14996, .T. ) ;
#25880 = AXIS2_PLACEMENT_3D ( 'NONE', #32331, #36708, #47924 ) ;
#25881 = EDGE_CURVE ( 'NONE', #7107, #7456, #30396, .T. ) ;
#25882 = ORIENTED_EDGE ( 'NONE', *, *, #23703, .T. ) ;
#25883 = DIRECTION ( 'NONE',  ( 1.000000000000000000, 0.000000000000000000, -1.586032892321652482E-16 ) ) ;
#25884 = CARTESIAN_POINT ( 'NONE',  ( 210.0000000000000568, 0.000000000000000000, -119.1817124430720440 ) ) ;
#25885 = VECTOR ( 'NONE', #40672, 1000.000000000000000 ) ;
#25886 = CYLINDRICAL_SURFACE ( 'NONE', #30239, 5.000000000000000000 ) ;
#25887 = EDGE_CURVE ( 'NONE', #9233, #43863, #15496, .T. ) ;
#25888 = CARTESIAN_POINT ( 'NONE',  ( -48.44597344681495343, 0.000000000000000000, 119.0682875569279702 ) ) ;
#25889 = EDGE_CURVE ( 'NONE', #39539, #32832, #42682, .T. ) ;
#25890 = VECTOR ( 'NONE', #1384, 1000.000000000000000 ) ;
#25891 =( BOUNDED_CURVE ( )  B_SPLINE_CURVE ( 3, ( #30171, #11435, #31204, #38150 ),
 .UNSPECIFIED., .F., .F. ) 
 B_SPLINE_CURVE_WITH_KNOTS ( ( 4, 4 ),
 ( 1.570796326794896558, 3.141592653589793116 ),
 .UNSPECIFIED. ) 
 CURVE ( )  GEOMETRIC_REPRESENTATION_ITEM ( )  RATIONAL_B_SPLINE_CURVE ( ( 1.000000000000000000, 0.8047378541243649375, 0.8047378541243649375, 1.000000000000000000 ) ) 
 REPRESENTATION_ITEM ( '' )  );
#25892 = DIRECTION ( 'NONE',  ( 0.000000000000000000, 0.000000000000000000, 1.000000000000000000 ) ) ;
#25893 = VERTEX_POINT ( 'NONE', #30655 ) ;
#25894 = DIRECTION ( 'NONE',  ( -0.000000000000000000, 0.000000000000000000, -1.000000000000000000 ) ) ;
#25895 = DIRECTION ( 'NONE',  ( -0.000000000000000000, -0.000000000000000000, -1.000000000000000000 ) ) ;
#25896 = PLANE ( 'NONE',  #26696 ) ;
#25897 = ORIENTED_EDGE ( 'NONE', *, *, #50101, .T. ) ;
#25898 = B_SPLINE_CURVE_WITH_KNOTS ( 'NONE', 3,
 ( #43114, #47425, #8738, #12074 ),
 .UNSPECIFIED., .F., .F.,
 ( 4, 4 ),
 ( 1.580408300606902237E-17, 0.009404495247862305896 ),
 .UNSPECIFIED. ) ;
#25899 = CARTESIAN_POINT ( 'NONE',  ( -168.4459734468149463, 0.000000000000000000, 42.56828755692798438 ) ) ;
#25900 = FACE_OUTER_BOUND ( 'NONE', #40481, .T. ) ;
#25901 = ORIENTED_EDGE ( 'NONE', *, *, #5333, .F. ) ;
#25902 = VECTOR ( 'NONE', #25461, 1000.000000000000000 ) ;
#25903 = ORIENTED_EDGE ( 'NONE', *, *, #47261, .F. ) ;
#25904 = VERTEX_POINT ( 'NONE', #50601 ) ;
#25905 = DIRECTION ( 'NONE',  ( 0.000000000000000000, 1.000000000000000000, 7.004339610132985974E-48 ) ) ;
#25906 = CARTESIAN_POINT ( 'NONE',  ( -124.9459734468149463, 2.143131898507847836E-16, 165.0000000000000000 ) ) ;
#25907 = ORIENTED_EDGE ( 'NONE', *, *, #14690, .T. ) ;
#25908 = VECTOR ( 'NONE', #8406, 1000.000000000000000 ) ;
#25909 = CARTESIAN_POINT ( 'NONE',  ( -4.672045878990125800, 50.00000000000000711, 1.847720168420772691 ) ) ;
#25910 = CARTESIAN_POINT ( 'NONE',  ( 1.275949648750062337, -0.1226307170719979495, 9.967237415621765351 ) ) ;
#25911 = FACE_BOUND ( 'NONE', #10296, .T. ) ;
#25912 = ADVANCED_FACE ( 'NONE', ( #4460 ), #28152, .T. ) ;
#25913 = CARTESIAN_POINT ( 'NONE',  ( 195.0540265531851105, 2.143131898507880377E-16, 2.568287556927978166 ) ) ;
#25914 = ADVANCED_FACE ( 'NONE', ( #35795 ), #19846, .F. ) ;
#25915 = VERTEX_POINT ( 'NONE', #8321 ) ;
#25916 = LINE ( 'NONE', #41299, #12221 ) ;
#25917 =( LENGTH_UNIT ( ) NAMED_UNIT ( * ) SI_UNIT ( .MILLI., .METRE. ) );
#25918 = PRODUCT_DEFINITION ( 'UNKNOWN', '', #20914, #43682 ) ;
#25919 = VERTEX_POINT ( 'NONE', #11152 ) ;
#25920 = CARTESIAN_POINT ( 'NONE',  ( 0.000000000000000000, 28.48684210526315752, 0.000000000000000000 ) ) ;
#25921 = CARTESIAN_POINT ( 'NONE',  ( -2.948105490345101387, -9.555557232197246620, 9.282506307616472441 ) ) ;
#25922 = VECTOR ( 'NONE', #9605, 1000.000000000000000 ) ;
#25923 = VECTOR ( 'NONE', #5432, 1000.000000000000000 ) ;
#25925 = AXIS2_PLACEMENT_3D ( 'NONE', #14138, #36774, #10054 ) ;
#25924 = CARTESIAN_POINT ( 'NONE',  ( 1.320835335343329753, -0.01943189459118491516, 9.943883492372847854 ) ) ;
#25926 = CARTESIAN_POINT ( 'NONE',  ( -124.9459734468149321, 1.025126265847082108, -117.4317124430720440 ) ) ;
#25927 = ORIENTED_EDGE ( 'NONE', *, *, #41518, .F. ) ;
#25928 = DIRECTION ( 'NONE',  ( -0.000000000000000000, -0.000000000000000000, -1.000000000000000000 ) ) ;
#25929 = ADVANCED_FACE ( 'NONE', ( #23192 ), #3950, .T. ) ;
#25930 = DIRECTION ( 'NONE',  ( 0.000000000000000000, 0.000000000000000000, -1.000000000000000000 ) ) ;
#25931 = DIRECTION ( 'NONE',  ( 0.000000000000000000, -1.000000000000000000, 0.000000000000000000 ) ) ;
#25932 = CYLINDRICAL_SURFACE ( 'NONE', #29074, 1.750000000000015543 ) ;
#25933 = SURFACE_STYLE_USAGE ( .BOTH. , #34644 ) ;
#25934 = AXIS2_PLACEMENT_3D ( 'NONE', #37525, #32915, #21590 ) ;
#25935 = ORIENTED_EDGE ( 'NONE', *, *, #41488, .T. ) ;
#25936 = CARTESIAN_POINT ( 'NONE',  ( 359.9999999999999432, -180.9999999999999716, 355.9999999999998295 ) ) ;
#25937 = VERTEX_POINT ( 'NONE', #26799 ) ;
#25938 = CARTESIAN_POINT ( 'NONE',  ( -14.49999999999999822, -46.01315789473684248, 5.916985404131813731 ) ) ;
#25939 = VECTOR ( 'NONE', #33871, 1000.000000000000000 ) ;
#25940 = EDGE_CURVE ( 'NONE', #27545, #49709, #12534, .T. ) ;
#25941 = VERTEX_POINT ( 'NONE', #23960 ) ;
#25942 = LINE ( 'NONE', #41577, #36931 ) ;
#25943 = CARTESIAN_POINT ( 'NONE',  ( 115.0540265531850395, 2.143131898507842906E-16, -165.0000000000000000 ) ) ;
#25944 = ORIENTED_EDGE ( 'NONE', *, *, #14632, .T. ) ;
#25945 = VECTOR ( 'NONE', #32136, 1000.000000000000000 ) ;
#25946 = EDGE_CURVE ( 'NONE', #31529, #26571, #26554, .T. ) ;
#25947 = LINE ( 'NONE', #10530, #4021 ) ;
#25948 = ADVANCED_FACE ( 'NONE', ( #35276 ), #35527, .F. ) ;
#25949 = ORIENTED_EDGE ( 'NONE', *, *, #13130, .F. ) ;
#25950 = CARTESIAN_POINT ( 'NONE',  ( 193.3040265531851105, 1.750000000000009992, 160.8182875569279702 ) ) ;
#25951 = CARTESIAN_POINT ( 'NONE',  ( 210.0000000000000568, 0.000000000000000000, 0.8182875569279768335 ) ) ;
#25952 = DIRECTION ( 'NONE',  ( 0.000000000000000000, 0.000000000000000000, 1.000000000000000000 ) ) ;
#25953 = CARTESIAN_POINT ( 'NONE',  ( 194.3291528190321742, 1.750000000000009548, -40.20683870891912193 ) ) ;
#25954 = CARTESIAN_POINT ( 'NONE',  ( 0.000000000000000000, 0.000000000000000000, 0.000000000000000000 ) ) ;
#25955 = ORIENTED_EDGE ( 'NONE', *, *, #32367, .T. ) ;
#25956 = EDGE_CURVE ( 'NONE', #11106, #34772, #47270, .T. ) ;
#25957 = VERTEX_POINT ( 'NONE', #46255 ) ;
#25958 = CARTESIAN_POINT ( 'NONE',  ( 34.32915281903212446, -1.750000000000009548, 121.8434138227750623 ) ) ;
#25959 = EDGE_CURVE ( 'NONE', #47807, #9479, #28231, .T. ) ;
#25960 = EDGE_CURVE ( 'NONE', #23178, #38152, #27045, .T. ) ;
#25961 = ORIENTED_EDGE ( 'NONE', *, *, #14196, .F. ) ;
#25962 = CIRCLE ( 'NONE', #18573, 2.000000000000001776 ) ;
#25963 = CARTESIAN_POINT ( 'NONE',  ( -124.9459734468149321, -1.025126265847081886, -80.93171244307201562 ) ) ;
#25964 = CARTESIAN_POINT ( 'NONE',  ( 344.0000000000000568, 185.0000000000000284, 349.9999999999998295 ) ) ;
#25965 = ORIENTED_EDGE ( 'NONE', *, *, #726, .F. ) ;
#25966 = FACE_OUTER_BOUND ( 'NONE', #22283, .T. ) ;
#25967 = EDGE_CURVE ( 'NONE', #48612, #7661, #43996, .T. ) ;
#25968 = ORIENTED_EDGE ( 'NONE', *, *, #15366, .F. ) ;
#25969 = CARTESIAN_POINT ( 'NONE',  ( 0.4166666666666664631, 0.000000000000000000, 10.00000000000000000 ) ) ;
#25970 = CARTESIAN_POINT ( 'NONE',  ( -1.148889881503118993, -0.6106841242179669171, 9.986087673579197244 ) ) ;
#25971 = CARTESIAN_POINT ( 'NONE',  ( 153.3040265531850537, 1.750000000000010658, -119.1817124430720440 ) ) ;
#25972 = CARTESIAN_POINT ( 'NONE',  ( 339.9999999999999432, 183.3431457505078583, -358.3431457505080857 ) ) ;
#25973 = CARTESIAN_POINT ( 'NONE',  ( 1.721971274562253740, 0.09408549481334846365, 9.928159647716247704 ) ) ;
#25974 = EDGE_LOOP ( 'NONE', ( #640, #12734, #41477, #41964 ) ) ;
#25975 = ORIENTED_EDGE ( 'NONE', *, *, #18580, .F. ) ;
#25976 = CARTESIAN_POINT ( 'NONE',  ( 152.2789002873379900, 1.750000000000009548, -38.15658617722494483 ) ) ;
#25977 = DIRECTION ( 'NONE',  ( -0.000000000000000000, -1.000000000000000000, -0.000000000000000000 ) ) ;
#25978 = CARTESIAN_POINT ( 'NONE',  ( -88.44597344681497475, 0.000000000000000000, -165.0000000000000000 ) ) ;
#25979 = EDGE_LOOP ( 'NONE', ( #49233, #19733, #47603, #36418, #15099, #43564 ) ) ;
#25980 = AXIS2_PLACEMENT_3D ( 'NONE', #21777, #6886, #2029 ) ;
#25981 = CARTESIAN_POINT ( 'NONE',  ( -167.4999999999999432, 47.50000000000000000, -18.87174264961130987 ) ) ;
#25982 = ORIENTED_EDGE ( 'NONE', *, *, #18934, .F. ) ;
#25983 = FACE_OUTER_BOUND ( 'NONE', #33485, .T. ) ;
#25984 = CYLINDRICAL_SURFACE ( 'NONE', #16246, 1.750000000000015543 ) ;
#25985 = CARTESIAN_POINT ( 'NONE',  ( 168.9999999999999716, -7.999999999999952038, -350.0000000000001705 ) ) ;
#25986 = FACE_OUTER_BOUND ( 'NONE', #46217, .T. ) ;
#25987 =( REPRESENTATION_RELATIONSHIP ('NONE','NONE', #3157, #8438 ) REPRESENTATION_RELATIONSHIP_WITH_TRANSFORMATION ( #48701 )SHAPE_REPRESENTATION_RELATIONSHIP( ) );
#25988 = CYLINDRICAL_SURFACE ( 'NONE', #35485, 1.750000000000015543 ) ;
#25989 = EDGE_LOOP ( 'NONE', ( #9720, #9659, #6868, #41581, #35164, #32031 ) ) ;
#25990 = CARTESIAN_POINT ( 'NONE',  ( -3.231548175622898089, 9.463461120997347820, 9.282506307616472441 ) ) ;
#25991 = DIRECTION ( 'NONE',  ( 1.000000000000000000, 0.000000000000000000, 0.000000000000000000 ) ) ;
#25992 = CARTESIAN_POINT ( 'NONE',  ( 0.9306608372802014362, 1.429911642202264854, 9.912103175172944702 ) ) ;
#25993 = EDGE_CURVE ( 'NONE', #48807, #19760, #32173, .T. ) ;
#25994 = FACE_OUTER_BOUND ( 'NONE', #29676, .T. ) ;
#25996 = ORIENTED_EDGE ( 'NONE', *, *, #40386, .T. ) ;
#25995 = VECTOR ( 'NONE', #45561, 1000.000000000000000 ) ;
#25997 = LINE ( 'NONE', #25742, #18781 ) ;
#25998 = ORIENTED_EDGE ( 'NONE', *, *, #16899, .T. ) ;
#25999 = CARTESIAN_POINT ( 'NONE',  ( 185.0000000000000284, 2.775557561562891351E-14, -111.0000000000001563 ) ) ;
#26000 = LINE ( 'NONE', #34722, #29046 ) ;
#26001 = CARTESIAN_POINT ( 'NONE',  ( 210.0000000000000568, 0.000000000000000000, -39.18171244307202983 ) ) ;
#26002 = ORIENTED_EDGE ( 'NONE', *, *, #12856, .T. ) ;
#26003 = ADVANCED_FACE ( 'NONE', ( #12407, #28061 ), #16262, .F. ) ;
#26004 = ADVANCED_FACE ( 'NONE', ( #17271 ), #13164, .T. ) ;
#26005 = CARTESIAN_POINT ( 'NONE',  ( 30.43621780902783058, -14.03210827430559249, -8.466730184410787174 ) ) ;
#26006 = ORIENTED_EDGE ( 'NONE', *, *, #48586, .T. ) ;
#26007 = CARTESIAN_POINT ( 'NONE',  ( -1.780432407520014415, -1.041450996408466612, 9.894754715216725671 ) ) ;
#26008 = LINE ( 'NONE', #37327, #26175 ) ;
#26009 = LINE ( 'NONE', #5988, #23387 ) ;
#26010 = EDGE_LOOP ( 'NONE', ( #35129, #35134, #44126, #32642, #13951, #48872 ) ) ;
#26011 = ORIENTED_EDGE ( 'NONE', *, *, #45883, .T. ) ;
#26012 = CARTESIAN_POINT ( 'NONE',  ( 15.00000000000000000, -46.01315789473684248, -5.916985404131818171 ) ) ;
#26013 = CARTESIAN_POINT ( 'NONE',  ( -25.79500241909648395, 7.611558401714507482, 229.0000000000000000 ) ) ;
#26014 = EDGE_CURVE ( 'NONE', #33295, #44965, #40628, .T. ) ;
#26015 = ADVANCED_FACE ( 'NONE', ( #48019 ), #28820, .F. ) ;
#26016 = VERTEX_POINT ( 'NONE', #24727 ) ;
#26017 = ORIENTED_EDGE ( 'NONE', *, *, #35057, .F. ) ;
#26018 = CARTESIAN_POINT ( 'NONE',  ( 75.05402655318508209, 0.000000000000000000, 162.5682875569279702 ) ) ;
#26019 = PLANE ( 'NONE',  #30025 ) ;
#26020 = VERTEX_POINT ( 'NONE', #28315 ) ;
#26021 = CARTESIAN_POINT ( 'NONE',  ( 113.3040265531850537, -1.749999999999996891, -159.1817124430720298 ) ) ;
#26022 = EDGE_CURVE ( 'NONE', #18930, #12164, #8822, .T. ) ;
#26023 = ORIENTED_EDGE ( 'NONE', *, *, #4639, .T. ) ;
#26024 = CARTESIAN_POINT ( 'NONE',  ( -177.4999999999999716, 57.49999999999996447, -9.999999999999973355 ) ) ;
#26025 =( BOUNDED_CURVE ( )  B_SPLINE_CURVE ( 3, ( #35087, #15318, #50657, #173 ),
 .UNSPECIFIED., .F., .F. ) 
 B_SPLINE_CURVE_WITH_KNOTS ( ( 4, 4 ),
 ( 0.000000000000000000, 1.570796326794896558 ),
 .UNSPECIFIED. ) 
 CURVE ( )  GEOMETRIC_REPRESENTATION_ITEM ( )  RATIONAL_B_SPLINE_CURVE ( ( 1.000000000000000000, 0.8047378541243649375, 0.8047378541243649375, 1.000000000000000000 ) ) 
 REPRESENTATION_ITEM ( '' )  );
#26026 = FACE_OUTER_BOUND ( 'NONE', #42990, .T. ) ;
#26027 = VECTOR ( 'NONE', #34503, 1000.000000000000000 ) ;
#26028 = ORIENTED_EDGE ( 'NONE', *, *, #50290, .F. ) ;
#26029 = VERTEX_POINT ( 'NONE', #31929 ) ;
#26030 =( BOUNDED_CURVE ( )  B_SPLINE_CURVE ( 3, ( #24140, #39536, #16669, #47180 ),
 .UNSPECIFIED., .F., .F. ) 
 B_SPLINE_CURVE_WITH_KNOTS ( ( 4, 4 ),
 ( 3.141592653589793116, 4.712388980384689674 ),
 .UNSPECIFIED. ) 
 CURVE ( )  GEOMETRIC_REPRESENTATION_ITEM ( )  RATIONAL_B_SPLINE_CURVE ( ( 1.000000000000000000, 0.8047378541243649375, 0.8047378541243649375, 1.000000000000000000 ) ) 
 REPRESENTATION_ITEM ( '' )  );
#26031 = CARTESIAN_POINT ( 'NONE',  ( 181.0000000000000284, -174.9999999999999716, -99.00000000000014211 ) ) ;
#26032 = ORIENTED_EDGE ( 'NONE', *, *, #11274, .T. ) ;
#26033 = DIRECTION ( 'NONE',  ( -1.000000000000000000, 3.172065745548403743E-16, -1.587271980518778491E-16 ) ) ;
#26034 = ORIENTED_EDGE ( 'NONE', *, *, #15636, .F. ) ;
#26035 = DIRECTION ( 'NONE',  ( -1.000000000000000000, -0.000000000000000000, -0.000000000000000000 ) ) ;
#26036 = CARTESIAN_POINT ( 'NONE',  ( 210.0000000000000568, 0.000000000000000000, 80.81828755692798438 ) ) ;
#26037 = VERTEX_POINT ( 'NONE', #32942 ) ;
#26038 = CARTESIAN_POINT ( 'NONE',  ( -208.1473046169136580, -154.8119894309599260, 22.84256005001721945 ) ) ;
#26039 = DIRECTION ( 'NONE',  ( 1.000000000000000000, 0.000000000000000000, 0.000000000000000000 ) ) ;
#26040 = CARTESIAN_POINT ( 'NONE',  ( -88.44597344681494633, 1.025126265847089213, -160.9317124430720014 ) ) ;
#26041 = DIRECTION ( 'NONE',  ( 0.000000000000000000, 0.000000000000000000, 1.000000000000000000 ) ) ;
#26042 = VERTEX_POINT ( 'NONE', #48519 ) ;
#26043 = CARTESIAN_POINT ( 'NONE',  ( 151.5540265531850537, -1.025126265847089435, -157.4317124430720582 ) ) ;
#26044 = LINE ( 'NONE', #6537, #6001 ) ;
#26045 = B_SPLINE_SURFACE_WITH_KNOTS ( 'NONE', 3, 3, ( 
 ( #26119, #29987, #45601, #10476 ),
 ( #28968, #9466, #40775, #44582 ),
 ( #41770, #25132, #21269, #36957 ),
 ( #1777, #7401, #10983, #6883 ) ),
 .UNSPECIFIED., .F., .F., .F.,
 ( 4, 4 ),
 ( 4, 4 ),
 ( 0.000000000000000000, 1.000000000000000000 ),
 ( 0.000000000000000000, 1.000000000000000000 ),
 .UNSPECIFIED. ) ;
#26046 = CARTESIAN_POINT ( 'NONE',  ( -11.73320209285699889, 11.96063479729179768, 9.403735324607438884 ) ) ;
#26047 = CARTESIAN_POINT ( 'NONE',  ( 71.55402655318505367, 0.000000000000000000, -37.43171244307200141 ) ) ;
#26048 = ADVANCED_FACE ( 'NONE', ( #20356, #9319 ), #12652, .F. ) ;
#26049 = CARTESIAN_POINT ( 'NONE',  ( -1.632255792517811388, 3.624924591517729056, 3.247138655587492817 ) ) ;
#26050 = LINE ( 'NONE', #14229, #26132 ) ;
#26051 = CARTESIAN_POINT ( 'NONE',  ( -33.89193117067290473, 21.24469349090191983, 910.0000000000000000 ) ) ;
#26052 = CARTESIAN_POINT ( 'NONE',  ( 210.0000000000000568, 2.143131898507884075E-16, -40.93171244307203693 ) ) ;
#26053 = PLANE ( 'NONE',  #37718 ) ;
#26054 = CARTESIAN_POINT ( 'NONE',  ( 46.75893035013449861, 17.89420872045614885, 3.199614146704519602 ) ) ;
#26055 = ORIENTED_EDGE ( 'NONE', *, *, #14954, .T. ) ;
#26056 = CIRCLE ( 'NONE', #31826, 3.500000000000003109 ) ;
#26057 = CARTESIAN_POINT ( 'NONE',  ( -31.28234235046239320, -11.28615439405757392, -3.760136334089591248 ) ) ;
#26058 = CARTESIAN_POINT ( 'NONE',  ( -25.60949810002096783, -43.19700938445173932, 1.847720168420772691 ) ) ;
#26059 = DIRECTION ( 'NONE',  ( 1.000000000000000000, 0.000000000000000000, -0.000000000000000000 ) ) ;
#26060 = CARTESIAN_POINT ( 'NONE',  ( 37.27397286063867199, -4.111076158911552092, 7.697694107796188234 ) ) ;
#26061 = ORIENTED_EDGE ( 'NONE', *, *, #9943, .T. ) ;
#26062 = EDGE_LOOP ( 'NONE', ( #17219, #35520, #47165, #34434 ) ) ;
#26063 = CARTESIAN_POINT ( 'NONE',  ( 1.250000000000000222, 0.000000000000000000, 3.333333333333333481 ) ) ;
#26064 = LINE ( 'NONE', #6561, #25467 ) ;
#26065 = ORIENTED_EDGE ( 'NONE', *, *, #43904, .F. ) ;
#26066 = CARTESIAN_POINT ( 'NONE',  ( 0.4166666666666664631, 0.000000000000000000, 10.00000000000000000 ) ) ;
#26067 = CARTESIAN_POINT ( 'NONE',  ( 195.0540265531851105, 2.143131898507880377E-16, -37.43171244307205825 ) ) ;
#26068 = ORIENTED_EDGE ( 'NONE', *, *, #29760, .F. ) ;
#26069 = EDGE_LOOP ( 'NONE', ( #30103, #21198, #13173, #35185 ) ) ;
#26070 = EDGE_CURVE ( 'NONE', #23873, #37300, #44790, .T. ) ;
#26071 = ORIENTED_EDGE ( 'NONE', *, *, #35068, .F. ) ;
#26072 = CARTESIAN_POINT ( 'NONE',  ( -14.99999999999906919, 17.00000000000000000, -24.99999999999999289 ) ) ;
#26073 = CARTESIAN_POINT ( 'NONE',  ( -0.1287570809895576818, -0.3962735484563154609, 10.00000000000000000 ) ) ;
#26074 = CARTESIAN_POINT ( 'NONE',  ( 15.00000000000000000, 12.87566193687862004, 19.86060803177194956 ) ) ;
#26075 = ORIENTED_EDGE ( 'NONE', *, *, #23196, .F. ) ;
#26076 = CYLINDRICAL_SURFACE ( 'NONE', #19389, 1.750000000000015543 ) ;
#26077 = CARTESIAN_POINT ( 'NONE',  ( -85.67084718096784002, 1.750000000000009548, -40.20683870891912193 ) ) ;
#26078 = ORIENTED_EDGE ( 'NONE', *, *, #21721, .F. ) ;
#26079 = VERTEX_POINT ( 'NONE', #1129 ) ;
#26080 = CARTESIAN_POINT ( 'NONE',  ( 113.3040265531850537, -1.749999999999996891, 160.8182875569279702 ) ) ;
#26081 = PLANE ( 'NONE',  #26728 ) ;
#26082 = CARTESIAN_POINT ( 'NONE',  ( 85.00000000000152056, 17.00000000000000000, 35.00000000000000000 ) ) ;
#26083 = VERTEX_POINT ( 'NONE', #24980 ) ;
#26084 = CARTESIAN_POINT ( 'NONE',  ( 5.551115123125782702E-14, -184.9999999999999716, 355.9999999999997726 ) ) ;
#26085 = CARTESIAN_POINT ( 'NONE',  ( 224.9999999999998863, -0.000000000000000000, 500.0000000000000000 ) ) ;
#26086 = CARTESIAN_POINT ( 'NONE',  ( -4.945973446814903696, 2.143131898507912917E-16, 122.5682875569279986 ) ) ;
#26087 = CARTESIAN_POINT ( 'NONE',  ( -208.4459734468149463, 0.000000000000000000, 79.06828755692797017 ) ) ;
#26088 = AXIS2_PLACEMENT_3D ( 'NONE', #8827, #28321, #28570 ) ;
#26089 = DIRECTION ( 'NONE',  ( 0.9510565162951545304, -0.3090169943749447312, 0.000000000000000000 ) ) ;
#26090 = VERTEX_POINT ( 'NONE', #20612 ) ;
#26091 = CARTESIAN_POINT ( 'NONE',  ( 31.55402655318503236, 0.000000000000000000, 165.0000000000000000 ) ) ;
#26092 = LINE ( 'NONE', #22250, #44508 ) ;
#26093 = CARTESIAN_POINT ( 'NONE',  ( -36.44255557191976180, -8.993813888722101524, -5.338708898921616708 ) ) ;
#26094 = CARTESIAN_POINT ( 'NONE',  ( -1.011271242968683426, -0.7347315653655928092, 10.00000000000000000 ) ) ;
#26095 = DIRECTION ( 'NONE',  ( -1.000000000000000000, -0.000000000000000000, -0.000000000000000000 ) ) ;
#26096 = VERTEX_POINT ( 'NONE', #37050 ) ;
#26097 = CARTESIAN_POINT ( 'NONE',  ( 181.0000000000000284, -9.999999999999953815, -113.0000000000001563 ) ) ;
#26098 = DIRECTION ( 'NONE',  ( 0.000000000000000000, 0.000000000000000000, 1.000000000000000000 ) ) ;
#26099 = LINE ( 'NONE', #42261, #50028 ) ;
#26100 = VERTEX_POINT ( 'NONE', #9573 ) ;
#26101 = CARTESIAN_POINT ( 'NONE',  ( 135.0000000000021600, 17.00000000000000000, 95.00000000000000000 ) ) ;
#26102 = CARTESIAN_POINT ( 'NONE',  ( -1.841312257079161796, -1.034875951311538422, 9.884520316594374023 ) ) ;
#26103 = VERTEX_POINT ( 'NONE', #12905 ) ;
#26104 = CARTESIAN_POINT ( 'NONE',  ( -126.6959734468149321, -1.749999999999997335, -79.18171244307201562 ) ) ;
#26105 = DIRECTION ( 'NONE',  ( 0.000000000000000000, -0.7071067811865473507, 0.7071067811865475727 ) ) ;
#26106 = DIRECTION ( 'NONE',  ( 1.000000000000000000, 0.000000000000000000, -1.586032892321652482E-16 ) ) ;
#26107 = PLANE ( 'NONE',  #31575 ) ;
#26108 = ORIENTED_EDGE ( 'NONE', *, *, #6367, .F. ) ;
#26109 = CARTESIAN_POINT ( 'NONE',  ( 34.32915281903212446, -1.750000000000009326, 1.843413822775066269 ) ) ;
#26110 = ORIENTED_EDGE ( 'NONE', *, *, #44214, .F. ) ;
#26111 = EDGE_LOOP ( 'NONE', ( #24380, #49507, #5863, #1431, #24055, #16681 ) ) ;
#26112 = CARTESIAN_POINT ( 'NONE',  ( 360.0000000000000568, 166.6568542494923975, 341.6568542494921985 ) ) ;
#26113 = AXIS2_PLACEMENT_3D ( 'NONE', #26540, #33748, #14482 ) ;
#26114 = VECTOR ( 'NONE', #26485, 1000.000000000000000 ) ;
#26115 = ADVANCED_FACE ( 'NONE', ( #47526 ), #28564, .T. ) ;
#26116 = ORIENTED_EDGE ( 'NONE', *, *, #28043, .F. ) ;
#26117 = CARTESIAN_POINT ( 'NONE',  ( 167.5000000000000000, 102.5000000000000284, -10.00000000000000000 ) ) ;
#26118 = CARTESIAN_POINT ( 'NONE',  ( 359.9999999999999432, -181.0000000000001421, -356.0000000000003411 ) ) ;
#26119 = CARTESIAN_POINT ( 'NONE',  ( 45.64490844644691236, 21.32281559348795952, 8.807470649214879543 ) ) ;
#26120 = VECTOR ( 'NONE', #4950, 1000.000000000000000 ) ;
#26121 = VECTOR ( 'NONE', #12015, 1000.000000000000000 ) ;
#26122 = EDGE_CURVE ( 'NONE', #41219, #28277, #32671, .T. ) ;
#26123 = CARTESIAN_POINT ( 'NONE',  ( -48.44597344681496054, -1.025126265847089657, 119.0682875569279560 ) ) ;
#26124 = FACE_OUTER_BOUND ( 'NONE', #15799, .T. ) ;
#26125 = VECTOR ( 'NONE', #17698, 1000.000000000000000 ) ;
#26126 = EDGE_LOOP ( 'NONE', ( #14354, #33921, #23892, #40537 ) ) ;
#26127 = EDGE_CURVE ( 'NONE', #4845, #43762, #44284, .T. ) ;
#26128 = CARTESIAN_POINT ( 'NONE',  ( 12.35406723005396046, -11.51001571518080624, 9.178419661560148768 ) ) ;
#26129 = CARTESIAN_POINT ( 'NONE',  ( 169.0000000000000000, -174.9999999999999716, -97.00000000000014211 ) ) ;
#26130 = EDGE_CURVE ( 'NONE', #47298, #15646, #21362, .T. ) ;
#26131 = CARTESIAN_POINT ( 'NONE',  ( -46.69597344681494633, 0.000000000000000000, -165.0000000000000000 ) ) ;
#26132 = VECTOR ( 'NONE', #10399, 1000.000000000000000 ) ;
#26133 = VERTEX_POINT ( 'NONE', #33687 ) ;
#26134 = CARTESIAN_POINT ( 'NONE',  ( 344.0000000000000000, -167.0000000000001137, -349.9999999999998863 ) ) ;
#26135 = DIRECTION ( 'NONE',  ( 0.000000000000000000, 0.000000000000000000, -1.000000000000000000 ) ) ;
#26136 = ORIENTED_EDGE ( 'NONE', *, *, #38083, .F. ) ;
#26137 = ORIENTED_EDGE ( 'NONE', *, *, #21582, .T. ) ;
#26138 = ORIENTED_EDGE ( 'NONE', *, *, #18452, .T. ) ;
#26139 = CARTESIAN_POINT ( 'NONE',  ( 185.0000000000000000, -168.9999999999999432, -340.0000000000001137 ) ) ;
#26140 = EDGE_CURVE ( 'NONE', #39173, #8236, #2857, .T. ) ;
#26141 = CARTESIAN_POINT ( 'NONE',  ( 342.8284271247460424, -183.0000000000001421, 358.0000000000001705 ) ) ;
#26142 = B_SPLINE_SURFACE_WITH_KNOTS ( 'NONE', 3, 3, ( 
 ( #19008, #34693, #26975, #42611 ),
 ( #38793, #3620, #19267, #50523 ),
 ( #47691, #8502, #27741, #23632 ),
 ( #23889, #43372, #31855, #32353 ) ),
 .UNSPECIFIED., .F., .F., .F.,
 ( 4, 4 ),
 ( 4, 4 ),
 ( 0.000000000000000000, 1.000000000000000000 ),
 ( 0.000000000000000000, 1.000000000000000000 ),
 .UNSPECIFIED. ) ;
#26143 = ORIENTED_EDGE ( 'NONE', *, *, #10803, .T. ) ;
#26144 = CARTESIAN_POINT ( 'NONE',  ( 75.05402655318509630, -1.025126265847089435, 122.5682875569280128 ) ) ;
#26145 = CARTESIAN_POINT ( 'NONE',  ( 181.0000000000000568, 165.0000000000000000, 357.9999999999998863 ) ) ;
#26146 = CARTESIAN_POINT ( 'NONE',  ( -88.44597344681494633, -1.025126265847089657, 119.0682875569279560 ) ) ;
#26147 = B_SPLINE_CURVE_WITH_KNOTS ( 'NONE', 3,
 ( #15773, #142, #31707, #12428 ),
 .UNSPECIFIED., .F., .F.,
 ( 4, 4 ),
 ( 0.003198294599461561517, 0.003311263741940095786 ),
 .UNSPECIFIED. ) ;
#26148 = FACE_OUTER_BOUND ( 'NONE', #34740, .T. ) ;
#26149 = ORIENTED_EDGE ( 'NONE', *, *, #44632, .T. ) ;
#26150 = FACE_BOUND ( 'NONE', #22787, .T. ) ;
#26151 =( NAMED_UNIT ( * ) SI_UNIT ( $, .STERADIAN. ) SOLID_ANGLE_UNIT ( ) );
#26152 = CARTESIAN_POINT ( 'NONE',  ( 210.0000000000000568, 0.000000000000000000, -77.43171244307200141 ) ) ;
#26153 = ADVANCED_FACE ( 'NONE', ( #25473 ), #41119, .F. ) ;
#26154 = EDGE_CURVE ( 'NONE', #15166, #5729, #14170, .T. ) ;
#26155 = VERTEX_POINT ( 'NONE', #6722 ) ;
#26156 = CONTEXT_DEPENDENT_SHAPE_REPRESENTATION ( #5663, #26986 ) ;
#26157 = VECTOR ( 'NONE', #15330, 1000.000000000000000 ) ;
#26158 = DIRECTION ( 'NONE',  ( 1.587271980518778491E-16, -5.169878828456422968E-26, -1.000000000000000000 ) ) ;
#26159 =( BOUNDED_CURVE ( )  B_SPLINE_CURVE ( 3, ( #25558, #41198, #37390, #17101 ),
 .UNSPECIFIED., .F., .F. ) 
 B_SPLINE_CURVE_WITH_KNOTS ( ( 4, 4 ),
 ( 3.141592653589793116, 4.712388980384689674 ),
 .UNSPECIFIED. ) 
 CURVE ( )  GEOMETRIC_REPRESENTATION_ITEM ( )  RATIONAL_B_SPLINE_CURVE ( ( 1.000000000000000000, 0.8047378541243649375, 0.8047378541243649375, 1.000000000000000000 ) ) 
 REPRESENTATION_ITEM ( '' )  );
#26160 = CARTESIAN_POINT ( 'NONE',  ( -168.4459734468149463, 0.000000000000000000, 79.06828755692797017 ) ) ;
#26161 = EDGE_CURVE ( 'NONE', #24507, #4778, #13669, .T. ) ;
#26162 = EDGE_CURVE ( 'NONE', #28181, #23498, #18517, .T. ) ;
#26163 = AXIS2_PLACEMENT_3D ( 'NONE', #14166, #22139, #41127 ) ;
#26164 = FACE_OUTER_BOUND ( 'NONE', #1455, .T. ) ;
#26165 = LINE ( 'NONE', #41809, #41242 ) ;
#26166 = ORIENTED_EDGE ( 'NONE', *, *, #8750, .T. ) ;
#26167 = ADVANCED_FACE ( 'NONE', ( #33192 ), #45690, .T. ) ;
#26168 = CARTESIAN_POINT ( 'NONE',  ( -6.695973446814940111, 1.750000000000024203, 120.8182875569279702 ) ) ;
#26169 = AXIS2_PLACEMENT_3D ( 'NONE', #49720, #21555, #2558 ) ;
#26170 = CARTESIAN_POINT ( 'NONE',  ( 183.0000000000000000, -268.4999999999993747, -114.9999999999999147 ) ) ;
#26171 =( BOUNDED_CURVE ( )  B_SPLINE_CURVE ( 3, ( #46121, #26410, #18456, #2803 ),
 .UNSPECIFIED., .F., .F. ) 
 B_SPLINE_CURVE_WITH_KNOTS ( ( 4, 4 ),
 ( 4.712388980384689674, 6.283185307179586232 ),
 .UNSPECIFIED. ) 
 CURVE ( )  GEOMETRIC_REPRESENTATION_ITEM ( )  RATIONAL_B_SPLINE_CURVE ( ( 1.000000000000000000, 0.8047378541243649375, 0.8047378541243649375, 1.000000000000000000 ) ) 
 REPRESENTATION_ITEM ( '' )  );
#26172 = ADVANCED_FACE ( 'NONE', ( #10568 ), #5965, .F. ) ;
#26173 = CARTESIAN_POINT ( 'NONE',  ( 112.2789002873379758, -1.749999999999996669, -160.2068387089191219 ) ) ;
#26174 = DIRECTION ( 'NONE',  ( 0.000000000000000000, 1.000000000000000000, 0.000000000000000000 ) ) ;
#26175 = VECTOR ( 'NONE', #26502, 1000.000000000000000 ) ;
#26176 = VERTEX_POINT ( 'NONE', #6979 ) ;
#26177 = DIRECTION ( 'NONE',  ( -0.000000000000000000, -0.000000000000000000, -1.000000000000000000 ) ) ;
#26178 = ORIENTED_EDGE ( 'NONE', *, *, #12499, .F. ) ;
#26179 = DIRECTION ( 'NONE',  ( 0.000000000000000000, -1.000000000000000000, 1.734723475976805517E-15 ) ) ;
#26180 = ORIENTED_EDGE ( 'NONE', *, *, #36176, .F. ) ;
#26181 = CARTESIAN_POINT ( 'NONE',  ( -84.94597344681494633, 2.143131898507880377E-16, -37.43171244307205825 ) ) ;
#26182 =( BOUNDED_CURVE ( )  B_SPLINE_CURVE ( 3, ( #40362, #28047, #611, #43435 ),
 .UNSPECIFIED., .F., .F. ) 
 B_SPLINE_CURVE_WITH_KNOTS ( ( 4, 4 ),
 ( 3.141592653589793116, 4.712388980384689674 ),
 .UNSPECIFIED. ) 
 CURVE ( )  GEOMETRIC_REPRESENTATION_ITEM ( )  RATIONAL_B_SPLINE_CURVE ( ( 1.000000000000000000, 0.8047378541243649375, 0.8047378541243649375, 1.000000000000000000 ) ) 
 REPRESENTATION_ITEM ( '' )  );
#26183 = VERTEX_POINT ( 'NONE', #14426 ) ;
#26184 = CARTESIAN_POINT ( 'NONE',  ( 155.0540265531850537, 2.143131898507880377E-16, 159.0682875569279702 ) ) ;
#26185 = EDGE_CURVE ( 'NONE', #40610, #28209, #15458, .T. ) ;
#26186 = ORIENTED_EDGE ( 'NONE', *, *, #20272, .F. ) ;
#26187 = ADVANCED_FACE ( 'NONE', ( #49524 ), #10824, .T. ) ;
#26188 = DIRECTION ( 'NONE',  ( -0.000000000000000000, 0.000000000000000000, 1.000000000000000000 ) ) ;
#26189 = EDGE_CURVE ( 'NONE', #38466, #48958, #33442, .T. ) ;
#26190 = ORIENTED_EDGE ( 'NONE', *, *, #41700, .F. ) ;
#26191 = CARTESIAN_POINT ( 'NONE',  ( 31.55402655318503236, 0.000000000000000000, -77.43171244307198720 ) ) ;
#26192 = CARTESIAN_POINT ( 'NONE',  ( 164.9999999999999716, 165.0000000000000000, -344.0000000000001137 ) ) ;
#26193 = CARTESIAN_POINT ( 'NONE',  ( -26.18032376592659105, 21.95228666728381128, 7.455576670931136185 ) ) ;
#26194 = LINE ( 'NONE', #41840, #45511 ) ;
#26195 = CARTESIAN_POINT ( 'NONE',  ( -8.445973446814964092, -1.025126265847097429, -80.93171244307204404 ) ) ;
#26196 = ORIENTED_EDGE ( 'NONE', *, *, #39677, .T. ) ;
#26197 = ORIENTED_EDGE ( 'NONE', *, *, #46280, .T. ) ;
#26198 = DIRECTION ( 'NONE',  ( -1.000000000000000000, -0.000000000000000000, -0.000000000000000000 ) ) ;
#26199 = CIRCLE ( 'NONE', #42588, 4.000000000000003553 ) ;
#26200 = B_SPLINE_CURVE_WITH_KNOTS ( 'NONE', 3,
 ( #13330, #17442, #44604, #9485 ),
 .UNSPECIFIED., .F., .F.,
 ( 4, 4 ),
 ( 5.641302087948371272E-05, 0.0003272669002642206951 ),
 .UNSPECIFIED. ) ;
#26201 = ADVANCED_FACE ( 'NONE', ( #29326 ), #21617, .F. ) ;
#26202 = VECTOR ( 'NONE', #6356, 1000.000000000000000 ) ;
#26203 = AXIS2_PLACEMENT_3D ( 'NONE', #48084, #9135, #5789 ) ;
#26204 = ORIENTED_EDGE ( 'NONE', *, *, #9992, .F. ) ;
#26205 = LINE ( 'NONE', #42090, #39857 ) ;
#26206 = LINE ( 'NONE', #42349, #17425 ) ;
#26207 = ORIENTED_EDGE ( 'NONE', *, *, #29267, .T. ) ;
#26208 = CARTESIAN_POINT ( 'NONE',  ( 151.5540265531850537, -1.025126265847089657, -120.9317124430720440 ) ) ;
#26209 = CIRCLE ( 'NONE', #45824, 8.000000000000000000 ) ;
#26210 = CARTESIAN_POINT ( 'NONE',  ( 210.0000000000000568, 0.000000000000000000, -117.4317124430720298 ) ) ;
#26211 = ORIENTED_EDGE ( 'NONE', *, *, #11245, .F. ) ;
#26212 = ADVANCED_FACE ( 'NONE', ( #45440 ), #45187, .F. ) ;
#26213 = LINE ( 'NONE', #46168, #47193 ) ;
#26214 = CARTESIAN_POINT ( 'NONE',  ( 25.04522487443081502, -22.77512090857307925, 8.356839323120299312 ) ) ;
#26215 = DIRECTION ( 'NONE',  ( 0.000000000000000000, 0.000000000000000000, -1.000000000000000000 ) ) ;
#26216 = VECTOR ( 'NONE', #30106, 1000.000000000000000 ) ;
#26217 = DIRECTION ( 'NONE',  ( 1.000000000000000000, 0.000000000000000000, 0.000000000000000000 ) ) ;
#26218 = EDGE_LOOP ( 'NONE', ( #21494, #33744, #39340, #32848, #43938 ) ) ;
#26219 = EDGE_CURVE ( 'NONE', #25523, #48356, #6469, .T. ) ;
#26220 = ORIENTED_EDGE ( 'NONE', *, *, #6466, .T. ) ;
#26221 = CARTESIAN_POINT ( 'NONE',  ( 168.9999999999999716, -182.9999999999999716, -350.0000000000001705 ) ) ;
#26222 = CARTESIAN_POINT ( 'NONE',  ( 23.29043492822826167, -24.10797434788167948, 1.847720168420772691 ) ) ;
#26223 = ORIENTED_EDGE ( 'NONE', *, *, #25466, .F. ) ;
#26224 = ORIENTED_EDGE ( 'NONE', *, *, #29996, .F. ) ;
#26225 = CARTESIAN_POINT ( 'NONE',  ( 867.4995338189988843, 1204.403237050701819, 1566.986414963432253 ) ) ;
#26226 = CARTESIAN_POINT ( 'NONE',  ( 151.5540265531850537, 0.000000000000000000, 165.0000000000000000 ) ) ;
#26227 = CARTESIAN_POINT ( 'NONE',  ( -25.79500241909648395, 7.611558401714507482, 229.0000000000000000 ) ) ;
#26228 = CARTESIAN_POINT ( 'NONE',  ( -23.26005729352344176, -44.90397804740339183, 7.906207997025717304 ) ) ;
#26229 = EDGE_CURVE ( 'NONE', #14126, #33150, #23390, .T. ) ;
#26230 = EDGE_CURVE ( 'NONE', #29044, #35915, #43143, .T. ) ;
#26231 = CARTESIAN_POINT ( 'NONE',  ( 165.0000000000000000, -168.9999999999999432, -115.0000000000001705 ) ) ;
#26232 = CARTESIAN_POINT ( 'NONE',  ( 0.5391758413130712801, -1.495929470048738663, 9.933337059263825708 ) ) ;
#26233 = CARTESIAN_POINT ( 'NONE',  ( 2.210477865340801706, 37.43479381012853224, -9.422646554964178023 ) ) ;
#26234 = VERTEX_POINT ( 'NONE', #42371 ) ;
#26235 = CARTESIAN_POINT ( 'NONE',  ( 339.9999999999999432, -174.9999999999999432, 343.9999999999998295 ) ) ;
#26236 = EDGE_CURVE ( 'NONE', #24955, #214, #9242, .T. ) ;
#26237 = CARTESIAN_POINT ( 'NONE',  ( -9.907356528110963012, 1.358045148327947427, 0.000000000000000000 ) ) ;
#26238 = CARTESIAN_POINT ( 'NONE',  ( 181.0000000000000000, -164.9999999999999432, -344.0000000000001137 ) ) ;
#26239 = VECTOR ( 'NONE', #43540, 1000.000000000000000 ) ;
#26240 = EDGE_CURVE ( 'NONE', #40932, #25760, #19274, .T. ) ;
#26241 = VECTOR ( 'NONE', #48798, 1000.000000000000000 ) ;
#26242 = ADVANCED_FACE ( 'NONE', ( #3884 ), #34445, .F. ) ;
#26243 = AXIS2_PLACEMENT_3D ( 'NONE', #48722, #32121, #24429 ) ;
#26244 = DIRECTION ( 'NONE',  ( -1.000000000000000000, 0.000000000000000000, -2.958228394578794708E-31 ) ) ;
#26245 = ORIENTED_EDGE ( 'NONE', *, *, #20609, .F. ) ;
#26246 = VECTOR ( 'NONE', #27629, 999.9999999999998863 ) ;
#26247 = VECTOR ( 'NONE', #25526, 1000.000000000000000 ) ;
#26248 = CARTESIAN_POINT ( 'NONE',  ( 34.99999999999997868, 17.00000000000000000, -114.9999999999999858 ) ) ;
#26249 = ORIENTED_EDGE ( 'NONE', *, *, #9359, .F. ) ;
#26250 = AXIS2_PLACEMENT_3D ( 'NONE', #7415, #19955, #15610 ) ;
#26251 = LINE ( 'NONE', #25999, #12313 ) ;
#26252 = VECTOR ( 'NONE', #35954, 1000.000000000000000 ) ;
#26253 = CARTESIAN_POINT ( 'NONE',  ( 27.33593271309472073, -41.94268121623323964, -9.367992836599951190 ) ) ;
#26254 = ORIENTED_EDGE ( 'NONE', *, *, #3585, .F. ) ;
#26255 = CIRCLE ( 'NONE', #19695, 1.750000000000009992 ) ;
#26256 = B_SPLINE_CURVE_WITH_KNOTS ( 'NONE', 3,
 ( #2572, #17965, #41082, #6430, #37755, #13624 ),
 .UNSPECIFIED., .F., .F.,
 ( 4, 2, 4 ),
 ( 7.757919228897728493E-18, 0.009877169331704830149, 0.01975433866340965336 ),
 .UNSPECIFIED. ) ;
#26257 = EDGE_CURVE ( 'NONE', #12693, #11343, #38307, .T. ) ;
#26258 = CARTESIAN_POINT ( 'NONE',  ( -120.0000000000000426, 16.00000000000000000, -114.9999999999999858 ) ) ;
#26259 = ORIENTED_EDGE ( 'NONE', *, *, #23478, .T. ) ;
#26260 = LINE ( 'NONE', #2636, #30380 ) ;
#26261 = CARTESIAN_POINT ( 'NONE',  ( 165.0000000000000000, 2.775557561562891351E-14, -111.0000000000001563 ) ) ;
#26262 = FACE_OUTER_BOUND ( 'NONE', #31727, .T. ) ;
#26263 = EDGE_LOOP ( 'NONE', ( #18227, #49180, #20261, #31763 ) ) ;
#26264 = ORIENTED_EDGE ( 'NONE', *, *, #26386, .F. ) ;
#26265 = DIRECTION ( 'NONE',  ( 0.000000000000000000, 0.000000000000000000, 1.000000000000000000 ) ) ;
#26266 = CARTESIAN_POINT ( 'NONE',  ( -64.99999999999846523, 17.00000000000000000, 35.00000000000000000 ) ) ;
#26267 = ORIENTED_EDGE ( 'NONE', *, *, #50290, .T. ) ;
#26268 = VERTEX_POINT ( 'NONE', #11594 ) ;
#26269 = DIRECTION ( 'NONE',  ( 1.000000000000000000, 0.000000000000000000, -0.000000000000000000 ) ) ;
#26270 = CARTESIAN_POINT ( 'NONE',  ( 154.1026953830863420, -98.56198943095992604, -17.65743994998275213 ) ) ;
#26271 = DIRECTION ( 'NONE',  ( -1.000000000000000000, -0.000000000000000000, -0.000000000000000000 ) ) ;
#26272 = ORIENTED_EDGE ( 'NONE', *, *, #33765, .T. ) ;
#26273 = FACE_OUTER_BOUND ( 'NONE', #31391, .T. ) ;
#26274 = ORIENTED_EDGE ( 'NONE', *, *, #49483, .T. ) ;
#26275 = DIRECTION ( 'NONE',  ( 0.000000000000000000, 1.000000000000000000, -5.664403186863042467E-17 ) ) ;
#26276 = AXIS2_PLACEMENT_3D ( 'NONE', #42765, #207, #43027 ) ;
#26277 = ORIENTED_EDGE ( 'NONE', *, *, #39909, .T. ) ;
#26278 = EDGE_LOOP ( 'NONE', ( #24068, #37005, #43413 ) ) ;
#26279 = ORIENTED_EDGE ( 'NONE', *, *, #8284, .T. ) ;
#26280 = FILL_AREA_STYLE_COLOUR ( '', #31668 ) ;
#26281 = LINE ( 'NONE', #14472, #23229 ) ;
#26282 = VERTEX_POINT ( 'NONE', #38801 ) ;
#26283 = CARTESIAN_POINT ( 'NONE',  ( 357.1715728752538439, -166.9999999999999432, 341.9999999999998295 ) ) ;
#26284 = VECTOR ( 'NONE', #8947, 1000.000000000000000 ) ;
#26285 = ORIENTED_EDGE ( 'NONE', *, *, #30744, .T. ) ;
#26286 = CARTESIAN_POINT ( 'NONE',  ( -3.414233368894360243, -9.411746240900615845, 6.185594734181532495 ) ) ;
#26287 = CARTESIAN_POINT ( 'NONE',  ( 166.9999999999999716, -272.4999999999999432, -344.0000000000001137 ) ) ;
#26288 = ORIENTED_EDGE ( 'NONE', *, *, #19588, .F. ) ;
#26289 = DIRECTION ( 'NONE',  ( 0.000000000000000000, -2.537652627714643577E-15, -1.000000000000000000 ) ) ;
#26290 = DIRECTION ( 'NONE',  ( 0.000000000000000000, 1.000000000000000000, 0.000000000000000000 ) ) ;
#26291 = DIRECTION ( 'NONE',  ( 0.000000000000000000, 0.000000000000000000, -1.000000000000000000 ) ) ;
#26292 = LINE ( 'NONE', #45998, #1557 ) ;
#26293 = ADVANCED_FACE ( 'NONE', ( #30588 ), #4147, .F. ) ;
#26294 = ADVANCED_FACE ( 'NONE', ( #18764 ), #46444, .F. ) ;
#26295 = LINE ( 'NONE', #18574, #24171 ) ;
#26296 = EDGE_LOOP ( 'NONE', ( #28197, #17262, #35767 ) ) ;
#26297 = CARTESIAN_POINT ( 'NONE',  ( 0.000000000000000000, 0.000000000000000000, 0.000000000000000000 ) ) ;
#26298 = EDGE_CURVE ( 'NONE', #29620, #22392, #11335, .T. ) ;
#26299 = DIRECTION ( 'NONE',  ( -0.000000000000000000, -0.000000000000000000, -1.000000000000000000 ) ) ;
#26300 = DIRECTION ( 'NONE',  ( -0.000000000000000000, -0.000000000000000000, -1.000000000000000000 ) ) ;
#26301 = B_SPLINE_CURVE_WITH_KNOTS ( 'NONE', 3,
 ( #28642, #5295, #20952, #40957 ),
 .UNSPECIFIED., .F., .F.,
 ( 4, 4 ),
 ( 0.001403500796105015260, 0.001586656765099046058 ),
 .UNSPECIFIED. ) ;
#26302 = EDGE_CURVE ( 'NONE', #36488, #1107, #20859, .T. ) ;
#26303 = EDGE_CURVE ( 'NONE', #28349, #37476, #14931, .T. ) ;
#26304 = CARTESIAN_POINT ( 'NONE',  ( -46.69597344681494633, 0.000000000000000000, 165.0000000000000000 ) ) ;
#26305 = DIRECTION ( 'NONE',  ( 0.000000000000000000, 0.000000000000000000, 1.000000000000000000 ) ) ;
#26306 = CARTESIAN_POINT ( 'NONE',  ( -84.94597344681493212, -1.025126265847088991, -157.4317124430720582 ) ) ;
#26307 = DIRECTION ( 'NONE',  ( 0.000000000000000000, 1.000000000000000000, 0.000000000000000000 ) ) ;
#26308 = EDGE_CURVE ( 'NONE', #21982, #45538, #15437, .T. ) ;
#26309 = CARTESIAN_POINT ( 'NONE',  ( 15.00099850811936264, 7.462898891544210933, 9.403735324607438884 ) ) ;
#26310 = VECTOR ( 'NONE', #40656, 1000.000000000000000 ) ;
#26311 = ORIENTED_EDGE ( 'NONE', *, *, #21301, .T. ) ;
#26312 = DIRECTION ( 'NONE',  ( -0.000000000000000000, 1.000000000000000000, 0.000000000000000000 ) ) ;
#26313 = CARTESIAN_POINT ( 'NONE',  ( 181.0000000000000284, 2.775557561562891351E-14, -115.0000000000001563 ) ) ;
#26314 = LINE ( 'NONE', #26562, #18792 ) ;
#26315 = CARTESIAN_POINT ( 'NONE',  ( 26.18032376592674737, -21.95228666728361233, 7.455576670931136185 ) ) ;
#26316 = CARTESIAN_POINT ( 'NONE',  ( -7.721099712662037540, 1.750000000000023315, -40.20683870891912903 ) ) ;
#26317 = VECTOR ( 'NONE', #31139, 1000.000000000000000 ) ;
#26318 = ORIENTED_EDGE ( 'NONE', *, *, #8064, .T. ) ;
#26319 = AXIS2_PLACEMENT_3D ( 'NONE', #38942, #39697, #682 ) ;
#26320 = VERTEX_POINT ( 'NONE', #15686 ) ;
#26321 = CARTESIAN_POINT ( 'NONE',  ( -2.569099690548740877, 33.19126772784019153, 3.199614146704519602 ) ) ;
#26322 = CARTESIAN_POINT ( 'NONE',  ( 1.780494907546722461, 1.041382914740401011, 9.891980816076523908 ) ) ;
#26323 = ORIENTED_EDGE ( 'NONE', *, *, #26447, .F. ) ;
#26324 = CARTESIAN_POINT ( 'NONE',  ( 210.0000000000000568, 0.000000000000000000, 2.568287556927987048 ) ) ;
#26325 = CARTESIAN_POINT ( 'NONE',  ( 191.5540265531851105, 0.000000000000000000, 2.568287556927978166 ) ) ;
#26326 = DIRECTION ( 'NONE',  ( 1.000000000000000000, 0.000000000000000000, 0.000000000000000000 ) ) ;
#26327 = ORIENTED_EDGE ( 'NONE', *, *, #37767, .F. ) ;
#26328 = VERTEX_POINT ( 'NONE', #15187 ) ;
#26329 = ORIENTED_EDGE ( 'NONE', *, *, #4381, .F. ) ;
#26330 =( BOUNDED_CURVE ( )  B_SPLINE_CURVE ( 3, ( #31833, #47418, #12306, #7972 ),
 .UNSPECIFIED., .F., .F. ) 
 B_SPLINE_CURVE_WITH_KNOTS ( ( 4, 4 ),
 ( 1.570796326794896558, 3.141592653589793116 ),
 .UNSPECIFIED. ) 
 CURVE ( )  GEOMETRIC_REPRESENTATION_ITEM ( )  RATIONAL_B_SPLINE_CURVE ( ( 1.000000000000000000, 0.8047378541243649375, 0.8047378541243649375, 1.000000000000000000 ) ) 
 REPRESENTATION_ITEM ( '' )  );
#26331 = EDGE_CURVE ( 'NONE', #30887, #7661, #30850, .T. ) ;
#26332 = CARTESIAN_POINT ( 'NONE',  ( -9.696760411816217839, -2.443938934554997999, 0.000000000000000000 ) ) ;
#26333 = CARTESIAN_POINT ( 'NONE',  ( 169.0000000000000000, -174.9999999999999716, -97.00000000000014211 ) ) ;
#26334 = DIRECTION ( 'NONE',  ( 0.000000000000000000, -1.000000000000000000, -0.000000000000000000 ) ) ;
#26335 = ORIENTED_EDGE ( 'NONE', *, *, #32652, .T. ) ;
#26336 = CYLINDRICAL_SURFACE ( 'NONE', #15304, 4.000000000000003553 ) ;
#26337 = CARTESIAN_POINT ( 'NONE',  ( -86.69597344681494633, 1.750000000000010214, -39.18171244307202983 ) ) ;
#26338 = CARTESIAN_POINT ( 'NONE',  ( 35.05402655318504657, 2.143131898507880377E-16, -0.9317124430720247208 ) ) ;
#26339 = EDGE_LOOP ( 'NONE', ( #13288, #10579, #43579, #27328 ) ) ;
#26340 = ORIENTED_EDGE ( 'NONE', *, *, #3882, .T. ) ;
#26341 = FACE_OUTER_BOUND ( 'NONE', #14971, .T. ) ;
#26342 = CARTESIAN_POINT ( 'NONE',  ( -64.99999999999940314, 17.00000000000000000, -54.99999999999999289 ) ) ;
#26343 = AXIS2_PLACEMENT_3D ( 'NONE', #14012, #36907, #1728 ) ;
#26344 = CARTESIAN_POINT ( 'NONE',  ( 2.948105490344985480, 9.555557232197198658, 9.282506307616484875 ) ) ;
#26345 = VERTEX_POINT ( 'NONE', #7497 ) ;
#26346 = ORIENTED_EDGE ( 'NONE', *, *, #45749, .T. ) ;
#26347 = AXIS2_PLACEMENT_3D ( 'NONE', #9795, #45863, #5952 ) ;
#26348 = CARTESIAN_POINT ( 'NONE',  ( -208.4459734468149463, 0.000000000000000000, -117.4317124430720725 ) ) ;
#26349 = DIRECTION ( 'NONE',  ( -0.000000000000000000, -0.000000000000000000, -1.000000000000000000 ) ) ;
#26350 = CARTESIAN_POINT ( 'NONE',  ( -50.00000000000000000, -50.00000000000000000, 900.0000000000000000 ) ) ;
#26351 = DIRECTION ( 'NONE',  ( 1.000000000000000000, 0.000000000000000000, 0.000000000000000000 ) ) ;
#26352 = LINE ( 'NONE', #41996, #28195 ) ;
#26353 = EDGE_LOOP ( 'NONE', ( #40654, #27077 ) ) ;
#26354 = CARTESIAN_POINT ( 'NONE',  ( 10.00000000000000000, 249.9999999999999716, 225.0000000000000000 ) ) ;
#26355 = CARTESIAN_POINT ( 'NONE',  ( -165.6708471809677974, -1.750000000000009548, -38.15658617722494483 ) ) ;
#26356 = LINE ( 'NONE', #18634, #16662 ) ;
#26357 = AXIS2_PLACEMENT_3D ( 'NONE', #18531, #30102, #29844 ) ;
#26358 = CARTESIAN_POINT ( 'NONE',  ( 50.24128791297869867, -41.04536285977715693, 5.000000000000000000 ) ) ;
#26359 = DIRECTION ( 'NONE',  ( 1.000000000000000000, 0.000000000000000000, 0.000000000000000000 ) ) ;
#26360 = CARTESIAN_POINT ( 'NONE',  ( -3.808200756227646089, -0.8261963378076270237, 9.741991644047246268 ) ) ;
#26361 = ORIENTED_EDGE ( 'NONE', *, *, #1064, .F. ) ;
#26362 = EDGE_CURVE ( 'NONE', #9086, #42678, #23128, .T. ) ;
#26363 = CARTESIAN_POINT ( 'NONE',  ( 6.174150299305392053, -33.14591993373988998, 8.807470649214879543 ) ) ;
#26364 = DIRECTION ( 'NONE',  ( -1.000000000000000000, 0.000000000000000000, -1.612977847700450206E-50 ) ) ;
#26365 = CARTESIAN_POINT ( 'NONE',  ( 0.000000000000000000, 0.000000000000000000, 0.000000000000000000 ) ) ;
#26366 = VERTEX_POINT ( 'NONE', #45588 ) ;
#26367 = CARTESIAN_POINT ( 'NONE',  ( 350.0000000000000000, -168.9999999999999432, -356.0000000000002274 ) ) ;
#26368 = CARTESIAN_POINT ( 'NONE',  ( -1.962712821592842882, -1.022159834731130257, 9.881002359080275355 ) ) ;
#26369 = EDGE_LOOP ( 'NONE', ( #47319, #8095, #35550, #10347, #13327 ) ) ;
#26370 = CARTESIAN_POINT ( 'NONE',  ( 135.0000000000021600, 16.00000000000000000, 95.00000000000000000 ) ) ;
#26371 = CARTESIAN_POINT ( 'NONE',  ( -8.445973446814976526, 0.000000000000000000, 119.0682875569279418 ) ) ;
#26372 = DIRECTION ( 'NONE',  ( 0.000000000000000000, 0.000000000000000000, 1.000000000000000000 ) ) ;
#26373 = CARTESIAN_POINT ( 'NONE',  ( 18.38319608353691947, -32.68498281710168385, -8.192531242611265085 ) ) ;
#26374 = AXIS2_PLACEMENT_3D ( 'NONE', #27792, #40356, #5193 ) ;
#26375 = VERTEX_POINT ( 'NONE', #33832 ) ;
#26376 = ORIENTED_EDGE ( 'NONE', *, *, #43825, .T. ) ;
#26377 = ORIENTED_EDGE ( 'NONE', *, *, #21949, .T. ) ;
#26378 = CARTESIAN_POINT ( 'NONE',  ( -9.999999999999998224, 8.486842105263161073, 18.34680996553531784 ) ) ;
#26379 = ORIENTED_EDGE ( 'NONE', *, *, #42565, .T. ) ;
#26380 = CARTESIAN_POINT ( 'NONE',  ( 168.9999999999999716, -81.49999999999997158, -350.0000000000001705 ) ) ;
#26381 = DIRECTION ( 'NONE',  ( -1.000000000000000000, -0.000000000000000000, -0.000000000000000000 ) ) ;
#26382 = DIRECTION ( 'NONE',  ( 1.000000000000000000, 0.000000000000000000, 0.000000000000000000 ) ) ;
#26383 = CARTESIAN_POINT ( 'NONE',  ( -14.99999999999812594, 17.00000000000000000, 90.00000000000000000 ) ) ;
#26384 = ORIENTED_EDGE ( 'NONE', *, *, #9875, .T. ) ;
#26386 = EDGE_CURVE ( 'NONE', #36764, #38992, #17659, .T. ) ;
#26385 = LINE ( 'NONE', #21780, #47728 ) ;
#26387 = DIRECTION ( 'NONE',  ( 0.000000000000000000, 0.000000000000000000, 1.000000000000000000 ) ) ;
#26388 = LINE ( 'NONE', #6133, #13572 ) ;
#26389 = VERTEX_POINT ( 'NONE', #18154 ) ;
#26390 = PLANE ( 'NONE',  #13010 ) ;
#26391 = ORIENTED_EDGE ( 'NONE', *, *, #16276, .T. ) ;
#26392 = ORIENTED_EDGE ( 'NONE', *, *, #24019, .F. ) ;
#26393 = ORIENTED_EDGE ( 'NONE', *, *, #29265, .T. ) ;
#26394 = DIRECTION ( 'NONE',  ( 0.000000000000000000, 0.000000000000000000, 1.000000000000000000 ) ) ;
#26395 = CARTESIAN_POINT ( 'NONE',  ( 341.9999999999998863, -182.1715728752539292, 357.1715728752539007 ) ) ;
#26396 = ORIENTED_EDGE ( 'NONE', *, *, #41736, .T. ) ;
#26397 = CARTESIAN_POINT ( 'NONE',  ( -1.249999999999999778, 0.000000000000000000, 10.00000000000000000 ) ) ;
#26398 = CARTESIAN_POINT ( 'NONE',  ( -46.69597344681494633, -1.750000000000009992, 160.8182875569279702 ) ) ;
#26399 = CARTESIAN_POINT ( 'NONE',  ( 113.3040265531850537, 1.749999999999997335, 120.8182875569279702 ) ) ;
#26400 = FACE_OUTER_BOUND ( 'NONE', #44220, .T. ) ;
#26401 = LINE ( 'NONE', #22548, #23406 ) ;
#26402 = CARTESIAN_POINT ( 'NONE',  ( -126.6959734468149321, -1.749999999999997335, 80.81828755692798438 ) ) ;
#26403 = VECTOR ( 'NONE', #37849, 1000.000000000000000 ) ;
#26404 = CARTESIAN_POINT ( 'NONE',  ( 1.011271242968683648, 0.7347315653655930312, 9.972675548442463622 ) ) ;
#26405 = AXIS2_PLACEMENT_3D ( 'NONE', #3180, #30662, #18832 ) ;
#26406 = ORIENTED_EDGE ( 'NONE', *, *, #31588, .F. ) ;
#26407 = CARTESIAN_POINT ( 'NONE',  ( 71.55402655318505367, 1.025126265847089435, -77.43171244307200141 ) ) ;
#26408 = CARTESIAN_POINT ( 'NONE',  ( 168.9999999999999716, -164.9999999999999432, -356.0000000000001705 ) ) ;
#26409 = AXIS2_PLACEMENT_3D ( 'NONE', #1657, #33226, #37079 ) ;
#26410 = CARTESIAN_POINT ( 'NONE',  ( -45.67084718096785423, -1.750000000000009548, 39.79316129108089228 ) ) ;
#26411 = ORIENTED_EDGE ( 'NONE', *, *, #43707, .T. ) ;
#26412 = CARTESIAN_POINT ( 'NONE',  ( 1.315487699543018918, -0.8933127557395131868, 9.933337059263825708 ) ) ;
#26413 = EDGE_CURVE ( 'NONE', #11508, #50635, #37439, .T. ) ;
#26414 = CARTESIAN_POINT ( 'NONE',  ( 0.3370904143228981575, -0.2449105217885261532, 10.00000000000000000 ) ) ;
#26415 = LINE ( 'NONE', #6924, #50660 ) ;
#26416 = CARTESIAN_POINT ( 'NONE',  ( 73.30402655318508209, 1.750000000000009992, 160.8182875569279702 ) ) ;
#26417 = DIRECTION ( 'NONE',  ( -0.000000000000000000, -0.000000000000000000, -1.000000000000000000 ) ) ;
#26418 = ORIENTED_EDGE ( 'NONE', *, *, #24409, .F. ) ;
#26419 =( NAMED_UNIT ( * ) SI_UNIT ( $, .STERADIAN. ) SOLID_ANGLE_UNIT ( ) );
#26420 = ORIENTED_EDGE ( 'NONE', *, *, #25089, .F. ) ;
#26421 = B_SPLINE_CURVE_WITH_KNOTS ( 'NONE', 3,
 ( #39754, #28888, #31300, #47140 ),
 .UNSPECIFIED., .F., .F.,
 ( 4, 4 ),
 ( 0.0009539133080775338879, 0.009404495247862345794 ),
 .UNSPECIFIED. ) ;
#26422 = DIRECTION ( 'NONE',  ( 0.000000000000000000, 1.734723475976805319E-15, 1.000000000000000000 ) ) ;
#26423 = ORIENTED_EDGE ( 'NONE', *, *, #40602, .F. ) ;
#26424 = CARTESIAN_POINT ( 'NONE',  ( 210.0000000000000568, 2.143131898507876926E-16, 79.06828755692797017 ) ) ;
#26426 = ADVANCED_FACE ( 'NONE', ( #41517 ), #49166, .T. ) ;
#26425 = CARTESIAN_POINT ( 'NONE',  ( 75.05402655318509630, 2.143131898507880377E-16, -120.9317124430720725 ) ) ;
#26427 = ADVANCED_FACE ( 'NONE', ( #17896 ), #13793, .T. ) ;
#26428 = ORIENTED_EDGE ( 'NONE', *, *, #30180, .T. ) ;
#26429 = DIRECTION ( 'NONE',  ( -1.000000000000000000, 0.000000000000000000, 0.000000000000000000 ) ) ;
#26430 = ORIENTED_EDGE ( 'NONE', *, *, #28417, .F. ) ;
#26431 = EDGE_CURVE ( 'NONE', #42347, #22458, #42199, .T. ) ;
#26432 = CARTESIAN_POINT ( 'NONE',  ( 191.5540265531851105, 0.000000000000000000, 82.56828755692798438 ) ) ;
#26433 = ORIENTED_EDGE ( 'NONE', *, *, #25001, .T. ) ;
#26434 = PLANE ( 'NONE',  #47475 ) ;
#26435 = FACE_OUTER_BOUND ( 'NONE', #42318, .T. ) ;
#26436 = MECHANICAL_DESIGN_GEOMETRIC_PRESENTATION_REPRESENTATION (  '', ( #45229 ), #19882 ) ;
#26437 = ORIENTED_EDGE ( 'NONE', *, *, #47534, .T. ) ;
#26438 = CARTESIAN_POINT ( 'NONE',  ( 210.0000000000000568, 2.143131898507881856E-16, 79.06828755692797017 ) ) ;
#26439 = AXIS2_PLACEMENT_3D ( 'NONE', #37420, #21482, #37172 ) ;
#26440 = CARTESIAN_POINT ( 'NONE',  ( 350.0000000000001137, 169.0000000000000000, 359.9999999999997726 ) ) ;
#26441 = EDGE_LOOP ( 'NONE', ( #40181, #40090 ) ) ;
#26443 = ORIENTED_EDGE ( 'NONE', *, *, #12770, .F. ) ;
#26442 = ADVANCED_FACE ( 'NONE', ( #10218 ), #14048, .T. ) ;
#26444 = CARTESIAN_POINT ( 'NONE',  ( -33.64889274059387958, 3.704246042440976439, 8.356839323120299312 ) ) ;
#26445 = EDGE_CURVE ( 'NONE', #9702, #7456, #8944, .T. ) ;
#26446 = VECTOR ( 'NONE', #46646, 1000.000000000000000 ) ;
#26447 = EDGE_CURVE ( 'NONE', #8111, #40403, #7295, .T. ) ;
#26448 = EDGE_CURVE ( 'NONE', #35388, #27665, #45330, .T. ) ;
#26449 = VERTEX_POINT ( 'NONE', #22008 ) ;
#26450 = AXIS2_PLACEMENT_3D ( 'NONE', #49687, #14834, #3025 ) ;
#26451 = DIRECTION ( 'NONE',  ( -0.000000000000000000, 0.000000000000000000, -1.000000000000000000 ) ) ;
#26452 = LINE ( 'NONE', #50510, #16619 ) ;
#26453 = ORIENTED_EDGE ( 'NONE', *, *, #48497, .T. ) ;
#26454 = CARTESIAN_POINT ( 'NONE',  ( -4.945973446814903696, 2.143131898507912917E-16, -120.9317124430720725 ) ) ;
#26455 = EDGE_CURVE ( 'NONE', #7807, #37221, #36947, .T. ) ;
#26456 = CARTESIAN_POINT ( 'NONE',  ( -208.4459734468149463, 0.000000000000000000, -77.43171244307204404 ) ) ;
#26457 = EDGE_LOOP ( 'NONE', ( #11552, #16164, #10059, #44710 ) ) ;
#26458 = LINE ( 'NONE', #50515, #32496 ) ;
#26459 = CARTESIAN_POINT ( 'NONE',  ( 154.3291528190321458, 1.750000000000010214, -118.1565861772249519 ) ) ;
#26460 = FACE_OUTER_BOUND ( 'NONE', #5048, .T. ) ;
#26461 =( BOUNDED_CURVE ( )  B_SPLINE_CURVE ( 3, ( #10708, #6869, #22511, #14045 ),
 .UNSPECIFIED., .F., .F. ) 
 B_SPLINE_CURVE_WITH_KNOTS ( ( 4, 4 ),
 ( 0.000000000000000000, 1.570796326794896558 ),
 .UNSPECIFIED. ) 
 CURVE ( )  GEOMETRIC_REPRESENTATION_ITEM ( )  RATIONAL_B_SPLINE_CURVE ( ( 1.000000000000000000, 0.8047378541243649375, 0.8047378541243649375, 1.000000000000000000 ) ) 
 REPRESENTATION_ITEM ( '' )  );
#26462 = CARTESIAN_POINT ( 'NONE',  ( -1.540526284687967706, 1.371707213411501147, 9.886433018048069954 ) ) ;
#26463 = ORIENTED_EDGE ( 'NONE', *, *, #8185, .F. ) ;
#26464 = CARTESIAN_POINT ( 'NONE',  ( -7.129058724845069861, -15.30620660340479766, 9.178419661560148768 ) ) ;
#26465 = CARTESIAN_POINT ( 'NONE',  ( -25.61277432017861955, 22.36370378792854297, 7.906207997025717304 ) ) ;
#26466 =( BOUNDED_CURVE ( )  B_SPLINE_CURVE ( 3, ( #8783, #4905, #20567, #40578 ),
 .UNSPECIFIED., .F., .F. ) 
 B_SPLINE_CURVE_WITH_KNOTS ( ( 4, 4 ),
 ( 0.000000000000000000, 1.570796326794896558 ),
 .UNSPECIFIED. ) 
 CURVE ( )  GEOMETRIC_REPRESENTATION_ITEM ( )  RATIONAL_B_SPLINE_CURVE ( ( 1.000000000000000000, 0.8047378541243649375, 0.8047378541243649375, 1.000000000000000000 ) ) 
 REPRESENTATION_ITEM ( '' )  );
#26467 = CARTESIAN_POINT ( 'NONE',  ( -0.3656201545664206076, 2.182515578491385000, 9.881002359080270026 ) ) ;
#26468 = EDGE_LOOP ( 'NONE', ( #45589, #4512, #26969, #14, #48253 ) ) ;
#26469 = EDGE_CURVE ( 'NONE', #26449, #2601, #41015, .T. ) ;
#26470 = ORIENTED_EDGE ( 'NONE', *, *, #27418, .T. ) ;
#26471 =( NAMED_UNIT ( * ) SI_UNIT ( $, .STERADIAN. ) SOLID_ANGLE_UNIT ( ) );
#26472 = DIRECTION ( 'NONE',  ( 0.000000000000000000, 0.000000000000000000, -1.000000000000000000 ) ) ;
#26473 = CARTESIAN_POINT ( 'NONE',  ( -176.3085477938156487, 57.49999999999996447, -19.92876838486919411 ) ) ;
#26474 = CARTESIAN_POINT ( 'NONE',  ( -114.9999999999984652, 17.00000000000000000, 35.00000000000000000 ) ) ;
#26475 = ADVANCED_FACE ( 'NONE', ( #10711 ), #37684, .F. ) ;
#26476 = EDGE_CURVE ( 'NONE', #9422, #48932, #37191, .T. ) ;
#26477 = LINE ( 'NONE', #22627, #43055 ) ;
#26478 = VECTOR ( 'NONE', #43277, 1000.000000000000000 ) ;
#26479 = CARTESIAN_POINT ( 'NONE',  ( 341.9999999999999432, 174.9999999999996589, -344.0000000000002842 ) ) ;
#26480 = CARTESIAN_POINT ( 'NONE',  ( 153.3040265531850537, 1.750000000000010658, 80.81828755692798438 ) ) ;
#26481 = ORIENTED_EDGE ( 'NONE', *, *, #16868, .F. ) ;
#26482 = CARTESIAN_POINT ( 'NONE',  ( 214.9999999999999432, 173.0000000000000000, 132.0000000000000000 ) ) ;
#26483 = ADVANCED_FACE ( 'NONE', ( #45081 ), #26107, .F. ) ;
#26484 =( BOUNDED_CURVE ( )  B_SPLINE_CURVE ( 3, ( #46045, #11205, #11698, #11963 ),
 .UNSPECIFIED., .F., .F. ) 
 B_SPLINE_CURVE_WITH_KNOTS ( ( 4, 4 ),
 ( 3.141592653589793116, 4.712388980384689674 ),
 .UNSPECIFIED. ) 
 CURVE ( )  GEOMETRIC_REPRESENTATION_ITEM ( )  RATIONAL_B_SPLINE_CURVE ( ( 1.000000000000000000, 0.8047378541243649375, 0.8047378541243649375, 1.000000000000000000 ) ) 
 REPRESENTATION_ITEM ( '' )  );
#26485 = DIRECTION ( 'NONE',  ( -0.000000000000000000, -1.000000000000000000, -0.000000000000000000 ) ) ;
#26486 = DIRECTION ( 'NONE',  ( -0.000000000000000000, -0.000000000000000000, -1.000000000000000000 ) ) ;
#26487 = AXIS2_PLACEMENT_3D ( 'NONE', #29211, #24855, #9700 ) ;
#26488 = EDGE_CURVE ( 'NONE', #23271, #26375, #24693, .T. ) ;
#26489 = FACE_OUTER_BOUND ( 'NONE', #33178, .T. ) ;
#26490 = ORIENTED_EDGE ( 'NONE', *, *, #46294, .T. ) ;
#26491 = AXIS2_PLACEMENT_3D ( 'NONE', #9007, #6162, #33626 ) ;
#26492 = CARTESIAN_POINT ( 'NONE',  ( 14.48769039275578407, 30.44468701195595983, 8.807470649214879543 ) ) ;
#26493 = ORIENTED_EDGE ( 'NONE', *, *, #9799, .T. ) ;
#26494 = DIRECTION ( 'NONE',  ( 0.000000000000000000, -1.000000000000000000, 0.000000000000000000 ) ) ;
#26495 = DIRECTION ( 'NONE',  ( 0.000000000000000000, 0.000000000000000000, 1.000000000000000000 ) ) ;
#26496 = DIRECTION ( 'NONE',  ( 6.765175596986472868E-16, -0.9749645535258953943, -0.2223603367690637489 ) ) ;
#26497 = EDGE_LOOP ( 'NONE', ( #39111, #46085, #5822, #1929 ) ) ;
#26498 = CARTESIAN_POINT ( 'NONE',  ( -1.377636575563021992, 0.6021164824561227036, 9.953784399990620813 ) ) ;
#26499 = ORIENTED_EDGE ( 'NONE', *, *, #15503, .F. ) ;
#26500 = CARTESIAN_POINT ( 'NONE',  ( -0.3862712429686977478, 1.188820645368937390, 10.00000000000000000 ) ) ;
#26501 = EDGE_CURVE ( 'NONE', #37542, #12765, #22267, .T. ) ;
#26502 = DIRECTION ( 'NONE',  ( 1.000000000000000000, 0.000000000000000000, 0.000000000000000000 ) ) ;
#26503 = CARTESIAN_POINT ( 'NONE',  ( -88.44597344681497475, 0.000000000000000000, 122.5682875569279986 ) ) ;
#26504 = VERTEX_POINT ( 'NONE', #38441 ) ;
#26505 = ORIENTED_EDGE ( 'NONE', *, *, #26928, .F. ) ;
#26506 = PLANE ( 'NONE',  #41461 ) ;
#26507 = DIRECTION ( 'NONE',  ( 0.000000000000000000, -0.000000000000000000, 1.000000000000000000 ) ) ;
#26508 = EDGE_CURVE ( 'NONE', #25153, #16301, #3257, .T. ) ;
#26509 = EDGE_CURVE ( 'NONE', #27159, #13148, #27100, .T. ) ;
#26510 = ORIENTED_EDGE ( 'NONE', *, *, #27169, .F. ) ;
#26511 = ORIENTED_EDGE ( 'NONE', *, *, #48982, .F. ) ;
#26512 = PLANE ( 'NONE',  #11015 ) ;
#26513 = CARTESIAN_POINT ( 'NONE',  ( 85.00000000000123634, 16.00000000000000000, 5.000000000000004441 ) ) ;
#26514 = AXIS2_PLACEMENT_3D ( 'NONE', #4850, #36179, #32328 ) ;
#26515 = CARTESIAN_POINT ( 'NONE',  ( -64.99999999999877787, 17.00000000000000000, 5.000000000000004441 ) ) ;
#26516 = ORIENTED_EDGE ( 'NONE', *, *, #1178, .F. ) ;
#26517 = FACE_OUTER_BOUND ( 'NONE', #19958, .T. ) ;
#26518 = EDGE_CURVE ( 'NONE', #26564, #6437, #14818, .T. ) ;
#26519 = VECTOR ( 'NONE', #37732, 1000.000000000000000 ) ;
#26520 = ORIENTED_EDGE ( 'NONE', *, *, #39750, .T. ) ;
#26521 = EDGE_CURVE ( 'NONE', #4446, #45409, #3782, .T. ) ;
#26522 = LINE ( 'NONE', #11126, #18935 ) ;
#26523 = VECTOR ( 'NONE', #7707, 1000.000000000000000 ) ;
#26524 = EDGE_CURVE ( 'NONE', #5061, #1180, #50323, .T. ) ;
#26525 = CARTESIAN_POINT ( 'NONE',  ( -168.4459734468149747, 1.025126265847089657, -80.93171244307201562 ) ) ;
#26526 = CARTESIAN_POINT ( 'NONE',  ( 2.961022939495062900, -16.59676755884084187, 2.590526750877053086 ) ) ;
#26527 = ORIENTED_EDGE ( 'NONE', *, *, #27586, .T. ) ;
#26528 = ORIENTED_EDGE ( 'NONE', *, *, #38369, .F. ) ;
#26529 = ORIENTED_EDGE ( 'NONE', *, *, #6410, .T. ) ;
#26530 = CARTESIAN_POINT ( 'NONE',  ( -14.76429217231967428, -8.192625680377590314, 9.178419661560148768 ) ) ;
#26531 = ORIENTED_EDGE ( 'NONE', *, *, #46224, .T. ) ;
#26532 = CARTESIAN_POINT ( 'NONE',  ( 0.8738110990266874101, 1.684976543153885453, 9.900811091504547079 ) ) ;
#26533 = ORIENTED_EDGE ( 'NONE', *, *, #19699, .F. ) ;
#26534 = CARTESIAN_POINT ( 'NONE',  ( 73.30402655318508209, 0.000000000000000000, 165.0000000000000000 ) ) ;
#26535 =( LENGTH_UNIT ( ) NAMED_UNIT ( * ) SI_UNIT ( .MILLI., .METRE. ) );
#26536 = VERTEX_POINT ( 'NONE', #19430 ) ;
#26537 = CARTESIAN_POINT ( 'NONE',  ( -12.35406723005387875, 11.51001571518090039, 9.178419661560148768 ) ) ;
#26538 = DIRECTION ( 'NONE',  ( 0.000000000000000000, 1.000000000000000000, -2.406552799042969348E-16 ) ) ;
#26539 = CARTESIAN_POINT ( 'NONE',  ( 74.32915281903215998, -1.750000000000009548, -118.1565861772249519 ) ) ;
#26540 = CARTESIAN_POINT ( 'NONE',  ( -54.99999999999997868, -52.50000000000000711, 5.000000000000000000 ) ) ;
#26541 = AXIS2_PLACEMENT_3D ( 'NONE', #7353, #39427, #22982 ) ;
#26542 = EDGE_CURVE ( 'NONE', #19082, #1605, #35108, .T. ) ;
#26543 = CARTESIAN_POINT ( 'NONE',  ( 214.9999999999999432, -173.0000000000000000, 352.0000000000000568 ) ) ;
#26544 = VERTEX_POINT ( 'NONE', #46840 ) ;
#26545 = CARTESIAN_POINT ( 'NONE',  ( 154.3291528190321458, -1.750000000000010436, 119.7931612910808781 ) ) ;
#26546 = DIRECTION ( 'NONE',  ( -0.000000000000000000, -0.000000000000000000, -1.000000000000000000 ) ) ;
#26547 = PRODUCT_DEFINITION ( 'UNKNOWN', '', #49539, #31917 ) ;
#26548 = CARTESIAN_POINT ( 'NONE',  ( 31.44259251615245176, 38.95901822126168668, -9.367992836599951190 ) ) ;
#26549 = CARTESIAN_POINT ( 'NONE',  ( 2.499999999999948930, -214.9999999999999716, -234.7500000000000000 ) ) ;
#26550 = CARTESIAN_POINT ( 'NONE',  ( -49.67735855322972327, 8.912210285362091255, 8.356839323120299312 ) ) ;
#26551 = VECTOR ( 'NONE', #29230, 1000.000000000000000 ) ;
#26552 = AXIS2_PLACEMENT_3D ( 'NONE', #49922, #46356, #26636 ) ;
#26553 = CARTESIAN_POINT ( 'NONE',  ( 34.32915281903212446, -1.750000000000010436, -80.20683870891910772 ) ) ;
#26554 = B_SPLINE_CURVE_WITH_KNOTS ( 'NONE', 3,
 ( #42431, #31682, #4213, #50345 ),
 .UNSPECIFIED., .F., .F.,
 ( 4, 4 ),
 ( 0.000000000000000000, 0.0002520763768929632940 ),
 .UNSPECIFIED. ) ;
#26555 = VECTOR ( 'NONE', #45703, 1000.000000000000000 ) ;
#26556 = EDGE_CURVE ( 'NONE', #38220, #13983, #17790, .T. ) ;
#26557 = DIRECTION ( 'NONE',  ( 0.000000000000000000, 1.000000000000000000, 0.000000000000000000 ) ) ;
#26558 = CARTESIAN_POINT ( 'NONE',  ( -166.6959734468149463, 1.750000000000010658, 120.8182875569279702 ) ) ;
#26559 = VECTOR ( 'NONE', #18911, 1000.000000000000000 ) ;
#26560 = EDGE_LOOP ( 'NONE', ( #41367, #29624, #44746, #30260 ) ) ;
#26561 = CARTESIAN_POINT ( 'NONE',  ( 1.011271242968677653, 0.7347315653656002477, 3.333333333333333481 ) ) ;
#26562 = CARTESIAN_POINT ( 'NONE',  ( -165.0000000000000284, 16.00000000000000000, 115.0000000000000142 ) ) ;
#26563 = CARTESIAN_POINT ( 'NONE',  ( -50.64730461691362962, 47.68801056904006685, 742.8425600500171413 ) ) ;
#26564 = VERTEX_POINT ( 'NONE', #15837 ) ;
#26565 = PRODUCT ( 'tire holder', 'tire holder', '', ( #21050 ) ) ;
#26566 = ORIENTED_EDGE ( 'NONE', *, *, #45015, .T. ) ;
#26567 = CARTESIAN_POINT ( 'NONE',  ( 72.27890028733797578, -1.750000000000010214, 119.7931612910808781 ) ) ;
#26568 = ADVANCED_FACE ( 'NONE', ( #7640 ), #22514, .T. ) ;
#26569 = AXIS2_PLACEMENT_3D ( 'NONE', #24350, #35901, #492 ) ;
#26570 = EDGE_CURVE ( 'NONE', #29055, #13717, #24994, .T. ) ;
#26571 = VERTEX_POINT ( 'NONE', #18908 ) ;
#26572 = ORIENTED_EDGE ( 'NONE', *, *, #15287, .T. ) ;
#26573 = CARTESIAN_POINT ( 'NONE',  ( 344.0000000000000000, 165.0000000000000000, -94.00000000000019895 ) ) ;
#26574 = CARTESIAN_POINT ( 'NONE',  ( 343.9999999999994316, 183.0000000000000284, -358.0000000000001705 ) ) ;
#26575 = CARTESIAN_POINT ( 'NONE',  ( -86.69597344681496054, 0.000000000000000000, 165.0000000000000000 ) ) ;
#26576 = ORIENTED_EDGE ( 'NONE', *, *, #34367, .T. ) ;
#26577 = ORIENTED_EDGE ( 'NONE', *, *, #42742, .T. ) ;
#26578 = ORIENTED_EDGE ( 'NONE', *, *, #11170, .T. ) ;
#26579 = EDGE_CURVE ( 'NONE', #41804, #36, #3009, .T. ) ;
#26581 = EDGE_CURVE ( 'NONE', #34586, #24521, #3507, .T. ) ;
#26580 = CARTESIAN_POINT ( 'NONE',  ( 75.05402655318509630, 2.143131898507880377E-16, 119.0682875569279560 ) ) ;
#26582 = DIRECTION ( 'NONE',  ( -0.000000000000000000, -0.000000000000000000, -1.000000000000000000 ) ) ;
#26583 = EDGE_CURVE ( 'NONE', #35690, #15972, #22769, .T. ) ;
#26584 = ORIENTED_EDGE ( 'NONE', *, *, #41650, .T. ) ;
#26585 = CARTESIAN_POINT ( 'NONE',  ( -48.44597344681495343, 0.000000000000000000, 165.0000000000000000 ) ) ;
#26586 = CARTESIAN_POINT ( 'NONE',  ( 31.55402655318503236, 0.000000000000000000, 82.56828755692798438 ) ) ;
#26587 = PLANE ( 'NONE',  #47445 ) ;
#26588 = AXIS2_PLACEMENT_3D ( 'NONE', #13195, #20645, #4991 ) ;
#26589 = ORIENTED_EDGE ( 'NONE', *, *, #1690, .F. ) ;
#26590 = ORIENTED_EDGE ( 'NONE', *, *, #13570, .T. ) ;
#26591 = CARTESIAN_POINT ( 'NONE',  ( 167.0000000000000000, -9.999999999999953815, -99.00000000000014211 ) ) ;
#26592 = AXIS2_PLACEMENT_3D ( 'NONE', #45587, #6871, #18907 ) ;
#26593 = CARTESIAN_POINT ( 'NONE',  ( -44.94597344681493922, 2.143131898507880377E-16, -40.93171244307205825 ) ) ;
#26594 = EDGE_CURVE ( 'NONE', #48164, #48573, #13641, .T. ) ;
#26595 = PLANE ( 'NONE',  #3730 ) ;
#26596 = ORIENTED_EDGE ( 'NONE', *, *, #92, .F. ) ;
#26597 = ORIENTED_EDGE ( 'NONE', *, *, #41357, .T. ) ;
#26598 = VECTOR ( 'NONE', #38154, 1000.000000000000000 ) ;
#26599 = CARTESIAN_POINT ( 'NONE',  ( -0.3862712429686977478, 1.188820645368937390, -10.00000000000000000 ) ) ;
#26600 = FACE_BOUND ( 'NONE', #47006, .T. ) ;
#26601 = CARTESIAN_POINT ( 'NONE',  ( 232.4999999999999716, -169.9999999999999716, 4.999999999999616307 ) ) ;
#26602 = DIRECTION ( 'NONE',  ( -1.000000000000000000, 0.000000000000000000, -1.612977847700450206E-50 ) ) ;
#26603 = CARTESIAN_POINT ( 'NONE',  ( -204.9459734468148895, 1.025126265847089879, -77.43171244307200141 ) ) ;
#26604 = ORIENTED_EDGE ( 'NONE', *, *, #19758, .T. ) ;
#26605 = CARTESIAN_POINT ( 'NONE',  ( -1.011271242968677875, -0.7347315653656004697, 10.00000000000000000 ) ) ;
#26606 = PLANE ( 'NONE',  #28135 ) ;
#26607 = CARTESIAN_POINT ( 'NONE',  ( 1.057156451998911839, -0.7920882637786250680, 9.943883492372851407 ) ) ;
#26608 = CYLINDRICAL_SURFACE ( 'NONE', #42700, 1.749999999999973799 ) ;
#26609 = AXIS2_PLACEMENT_3D ( 'NONE', #5711, #47766, #36794 ) ;
#26610 = CARTESIAN_POINT ( 'NONE',  ( -126.6959734468149321, 1.749999999999997335, -119.1817124430720440 ) ) ;
#26611 = AXIS2_PLACEMENT_3D ( 'NONE', #10512, #26174, #29769 ) ;
#26612 = EDGE_LOOP ( 'NONE', ( #47800, #39899 ) ) ;
#26613 = DIRECTION ( 'NONE',  ( -1.000000000000000000, 0.000000000000000000, 0.000000000000000000 ) ) ;
#26614 = CARTESIAN_POINT ( 'NONE',  ( -2.462075149652696027, 16.57295996686994499, 9.403735324607438884 ) ) ;
#26615 = DIRECTION ( 'NONE',  ( -0.000000000000000000, -0.000000000000000000, -1.000000000000000000 ) ) ;
#26616 = EDGE_CURVE ( 'NONE', #36948, #1440, #29544, .T. ) ;
#26617 = ORIENTED_EDGE ( 'NONE', *, *, #933, .T. ) ;
#26618 = CARTESIAN_POINT ( 'NONE',  ( 113.3040265531850537, 1.749999999999997335, -79.18171244307201562 ) ) ;
#26619 = CARTESIAN_POINT ( 'NONE',  ( 340.0000000000000568, 183.0000000000000284, 343.9999999999997726 ) ) ;
#26620 = VECTOR ( 'NONE', #34283, 1000.000000000000000 ) ;
#26621 = ORIENTED_EDGE ( 'NONE', *, *, #47852, .F. ) ;
#26622 = DIRECTION ( 'NONE',  ( 0.000000000000000000, 1.000000000000000000, 0.000000000000000000 ) ) ;
#26623 = CARTESIAN_POINT ( 'NONE',  ( -126.6959734468149321, 1.749999999999997335, 120.8182875569279702 ) ) ;
#26624 = CARTESIAN_POINT ( 'NONE',  ( 2.500000000000003997, 194.9999999999999716, -240.0000000000000000 ) ) ;
#26625 =( BOUNDED_CURVE ( )  B_SPLINE_CURVE ( 3, ( #32964, #2394, #17545, #10094 ),
 .UNSPECIFIED., .F., .F. ) 
 B_SPLINE_CURVE_WITH_KNOTS ( ( 4, 4 ),
 ( 0.000000000000000000, 1.570796326794896558 ),
 .UNSPECIFIED. ) 
 CURVE ( )  GEOMETRIC_REPRESENTATION_ITEM ( )  RATIONAL_B_SPLINE_CURVE ( ( 1.000000000000000000, 0.8047378541243649375, 0.8047378541243649375, 1.000000000000000000 ) ) 
 REPRESENTATION_ITEM ( '' )  );
#26626 = ORIENTED_EDGE ( 'NONE', *, *, #6195, .T. ) ;
#26627 = CARTESIAN_POINT ( 'NONE',  ( 33.30402655318503946, -1.750000000000009992, 0.8182875569279768335 ) ) ;
#26628 = ORIENTED_EDGE ( 'NONE', *, *, #23108, .T. ) ;
#26629 = ORIENTED_EDGE ( 'NONE', *, *, #16468, .T. ) ;
#26630 = AXIS2_PLACEMENT_3D ( 'NONE', #17570, #21931, #41676 ) ;
#26631 = CARTESIAN_POINT ( 'NONE',  ( -84.94597344681494633, 2.143131898507880377E-16, 165.0000000000000000 ) ) ;
#26632 = EDGE_CURVE ( 'NONE', #2845, #18735, #27389, .T. ) ;
#26633 = EDGE_CURVE ( 'NONE', #35523, #32541, #44273, .T. ) ;
#26634 = EDGE_LOOP ( 'NONE', ( #23645, #16066, #23880, #8074 ) ) ;
#26635 = DIRECTION ( 'NONE',  ( -1.000000000000000000, -0.000000000000000000, -0.000000000000000000 ) ) ;
#26636 = DIRECTION ( 'NONE',  ( 0.000000000000000000, 0.000000000000000000, 1.000000000000000000 ) ) ;
#26637 = CARTESIAN_POINT ( 'NONE',  ( 165.0000000000000284, 175.0000000000000284, 355.9999999999998863 ) ) ;
#26638 = LINE ( 'NONE', #35379, #42334 ) ;
#26639 = B_SPLINE_CURVE_WITH_KNOTS ( 'NONE', 3,
 ( #49020, #6725, #10075, #33445 ),
 .UNSPECIFIED., .F., .F.,
 ( 4, 4 ),
 ( 8.940560153363745023E-19, 0.0003726843654217072417 ),
 .UNSPECIFIED. ) ;
#26640 = ORIENTED_EDGE ( 'NONE', *, *, #31652, .F. ) ;
#26641 = CARTESIAN_POINT ( 'NONE',  ( 35.00000000000152767, 17.00000000000000000, 60.00000000000000000 ) ) ;
#26643 = EDGE_CURVE ( 'NONE', #27700, #40814, #33525, .T. ) ;
#26642 = FACE_OUTER_BOUND ( 'NONE', #24560, .T. ) ;
#26644 = CYLINDRICAL_SURFACE ( 'NONE', #47965, 1.750000000000008438 ) ;
#26645 = EDGE_CURVE ( 'NONE', #10986, #42541, #28404, .T. ) ;
#26646 = DIRECTION ( 'NONE',  ( -1.000000000000000000, -0.000000000000000000, -0.000000000000000000 ) ) ;
#26647 = VECTOR ( 'NONE', #12742, 1000.000000000000000 ) ;
#26648 = VERTEX_POINT ( 'NONE', #23794 ) ;
#26649 = CARTESIAN_POINT ( 'NONE',  ( -204.9459734468149463, 2.143131898507880377E-16, -120.9317124430720156 ) ) ;
#26650 = CARTESIAN_POINT ( 'NONE',  ( -582.5000000000000000, 57.49999999999996447, -58.60000000000003695 ) ) ;
#26651 = ORIENTED_EDGE ( 'NONE', *, *, #47726, .T. ) ;
#26652 = VECTOR ( 'NONE', #50422, 1000.000000000000000 ) ;
#26653 = ORIENTED_EDGE ( 'NONE', *, *, #18249, .T. ) ;
#26654 = ORIENTED_EDGE ( 'NONE', *, *, #35975, .F. ) ;
#26655 = DIRECTION ( 'NONE',  ( 1.000000000000000000, 0.000000000000000000, 7.793956916774525800E-48 ) ) ;
#26656 = EDGE_CURVE ( 'NONE', #4452, #31279, #42352, .T. ) ;
#26657 = CARTESIAN_POINT ( 'NONE',  ( 25.60949810002064098, 43.19700938445193827, 1.847720168420772691 ) ) ;
#26658 = ORIENTED_EDGE ( 'NONE', *, *, #28450, .F. ) ;
#26659 = CARTESIAN_POINT ( 'NONE',  ( -208.4459734468149463, 0.000000000000000000, -0.9317124430720247208 ) ) ;
#26660 = FACE_BOUND ( 'NONE', #38301, .T. ) ;
#26661 = CARTESIAN_POINT ( 'NONE',  ( -114.9999999999978542, 17.00000000000000000, 95.00000000000000000 ) ) ;
#26662 = CARTESIAN_POINT ( 'NONE',  ( 344.0000000000000000, -165.0000000000001137, -340.0000000000003411 ) ) ;
#26663 = CARTESIAN_POINT ( 'NONE',  ( 340.0000000000000000, 165.0000000000000000, -106.0000000000001990 ) ) ;
#26664 = AXIS2_PLACEMENT_3D ( 'NONE', #18071, #26289, #22934 ) ;
#26665 = AXIS2_PLACEMENT_3D ( 'NONE', #20219, #3808, #47369 ) ;
#26666 = CARTESIAN_POINT ( 'NONE',  ( -9.999999999999998224, 8.486842105263161073, -18.34680996553531784 ) ) ;
#26667 = DIRECTION ( 'NONE',  ( -1.000000000000000000, 0.000000000000000000, 0.000000000000000000 ) ) ;
#26668 = LINE ( 'NONE', #22303, #41194 ) ;
#26669 = AXIS2_PLACEMENT_3D ( 'NONE', #38796, #15948, #561 ) ;
#26670 = VECTOR ( 'NONE', #28055, 1000.000000000000000 ) ;
#26671 = ORIENTED_EDGE ( 'NONE', *, *, #12404, .F. ) ;
#26672 = CARTESIAN_POINT ( 'NONE',  ( -164.4973046169135955, -97.66198943095992036, -17.65743994998277699 ) ) ;
#26673 = DIRECTION ( 'NONE',  ( 0.000000000000000000, 0.000000000000000000, 1.000000000000000000 ) ) ;
#26674 = LINE ( 'NONE', #42315, #38847 ) ;
#26675 = CARTESIAN_POINT ( 'NONE',  ( -1.642172164747307761, 0.000000000000000000, 0.000000000000000000 ) ) ;
#26676 = ORIENTED_EDGE ( 'NONE', *, *, #30989, .F. ) ;
#26677 = CARTESIAN_POINT ( 'NONE',  ( -9.221081804193374865, -13.81382350053984176, 3.266473740018926541 ) ) ;
#26678 = CYLINDRICAL_SURFACE ( 'NONE', #29462, 1.750000000000001554 ) ;
#26679 = CARTESIAN_POINT ( 'NONE',  ( -114.9999999999987779, 17.00000000000000000, 5.000000000000004441 ) ) ;
#26680 = CARTESIAN_POINT ( 'NONE',  ( -4.999999999999999112, 222.4999999999999716, -228.6347188485896140 ) ) ;
#26681 = CARTESIAN_POINT ( 'NONE',  ( 72.27890028733797578, 1.750000000000009326, 1.843413822775066269 ) ) ;
#26682 = EDGE_CURVE ( 'NONE', #24906, #35538, #42054, .T. ) ;
#26683 = ORIENTED_EDGE ( 'NONE', *, *, #20669, .T. ) ;
#26684 = AXIS2_PLACEMENT_3D ( 'NONE', #24190, #36248, #20323 ) ;
#26685 = FILL_AREA_STYLE ('',( #19217 ) ) ;
#26686 = ORIENTED_EDGE ( 'NONE', *, *, #32682, .F. ) ;
#26687 = CARTESIAN_POINT ( 'NONE',  ( 16.52264463346132572, -2.779753662172757878, 9.403735324607438884 ) ) ;
#26688 = VECTOR ( 'NONE', #31721, 1000.000000000000000 ) ;
#26689 = EDGE_LOOP ( 'NONE', ( #38694, #40858, #25700, #24248 ) ) ;
#26690 = CARTESIAN_POINT ( 'NONE',  ( -84.94597344681493212, 1.025126265847089657, 119.0682875569279560 ) ) ;
#26691 = LINE ( 'NONE', #49228, #15088 ) ;
#26692 = VECTOR ( 'NONE', #5963, 1000.000000000000000 ) ;
#26693 = EDGE_LOOP ( 'NONE', ( #17031, #18806, #47748, #28217 ) ) ;
#26694 = LINE ( 'NONE', #8465, #38809 ) ;
#26695 = ORIENTED_EDGE ( 'NONE', *, *, #23688, .F. ) ;
#26696 = AXIS2_PLACEMENT_3D ( 'NONE', #41276, #45609, #34106 ) ;
#26697 = ORIENTED_EDGE ( 'NONE', *, *, #35912, .T. ) ;
#26698 = CARTESIAN_POINT ( 'NONE',  ( -0.9390173899430289683, -1.130417317737636651, 9.958264684458541183 ) ) ;
#26699 = DIRECTION ( 'NONE',  ( -0.000000000000000000, -0.000000000000000000, -1.000000000000000000 ) ) ;
#26700 = VECTOR ( 'NONE', #12150, 1000.000000000000000 ) ;
#26701 = VERTEX_POINT ( 'NONE', #36635 ) ;
#26702 = DIRECTION ( 'NONE',  ( -1.000000000000000000, -0.000000000000000000, -0.000000000000000000 ) ) ;
#26703 = DIRECTION ( 'NONE',  ( 0.000000000000000000, 0.000000000000000000, 1.000000000000000000 ) ) ;
#26704 = DIRECTION ( 'NONE',  ( -1.000000000000000000, 0.000000000000000000, 0.000000000000000000 ) ) ;
#26705 = ORIENTED_EDGE ( 'NONE', *, *, #14056, .T. ) ;
#26706 = ORIENTED_EDGE ( 'NONE', *, *, #13026, .T. ) ;
#26707 = DIRECTION ( 'NONE',  ( 0.000000000000000000, 0.000000000000000000, -1.000000000000000000 ) ) ;
#26708 = AXIS2_PLACEMENT_3D ( 'NONE', #38932, #39185, #30718 ) ;
#26709 = AXIS2_PLACEMENT_3D ( 'NONE', #37074, #16545, #25247 ) ;
#26710 = CARTESIAN_POINT ( 'NONE',  ( -47.55282581475762527, -15.45084971874758217, 0.000000000000000000 ) ) ;
#26711 = EDGE_LOOP ( 'NONE', ( #34409, #20754, #49378, #30693, #39937, #7408 ) ) ;
#26712 = DIRECTION ( 'NONE',  ( -1.000000000000000000, 0.000000000000000000, 0.000000000000000000 ) ) ;
#26713 = DIRECTION ( 'NONE',  ( 0.000000000000000000, 0.000000000000000000, 1.000000000000000000 ) ) ;
#26714 =( BOUNDED_CURVE ( )  B_SPLINE_CURVE ( 3, ( #14458, #5997, #33470, #45722 ),
 .UNSPECIFIED., .F., .F. ) 
 B_SPLINE_CURVE_WITH_KNOTS ( ( 4, 4 ),
 ( 1.570796326794896558, 3.141592653589793116 ),
 .UNSPECIFIED. ) 
 CURVE ( )  GEOMETRIC_REPRESENTATION_ITEM ( )  RATIONAL_B_SPLINE_CURVE ( ( 1.000000000000000000, 0.8047378541243649375, 0.8047378541243649375, 1.000000000000000000 ) ) 
 REPRESENTATION_ITEM ( '' )  );
#26715 = ORIENTED_EDGE ( 'NONE', *, *, #32744, .T. ) ;
#26716 = CARTESIAN_POINT ( 'NONE',  ( -4.945973446814916130, 1.025126265847097429, -120.9317124430720440 ) ) ;
#26717 = ADVANCED_FACE ( 'NONE', ( #12480 ), #691, .T. ) ;
#26718 = CARTESIAN_POINT ( 'NONE',  ( -166.6959734468149463, 1.750000000000010658, 80.81828755692798438 ) ) ;
#26719 = ORIENTED_EDGE ( 'NONE', *, *, #21814, .T. ) ;
#26720 = CARTESIAN_POINT ( 'NONE',  ( 130.0000000000002842, 17.00000000000000000, -84.99999999999998579 ) ) ;
#26721 = CARTESIAN_POINT ( 'NONE',  ( 339.9999999999999432, -180.9999999999999716, -358.0000000000002274 ) ) ;
#26722 = DIRECTION ( 'NONE',  ( -3.364279341222521245E-16, -0.7071067811865474617, 0.7071067811865476838 ) ) ;
#26723 = CARTESIAN_POINT ( 'NONE',  ( 0.5113015165352333691, 1.175527691268683395, 9.948547179989619238 ) ) ;
#26724 = VECTOR ( 'NONE', #19379, 1000.000000000000000 ) ;
#26725 = VECTOR ( 'NONE', #11311, 1000.000000000000000 ) ;
#26726 = ORIENTED_EDGE ( 'NONE', *, *, #12037, .F. ) ;
#26727 = LINE ( 'NONE', #3358, #29433 ) ;
#26728 = AXIS2_PLACEMENT_3D ( 'NONE', #26342, #21979, #32347 ) ;
#26729 = CARTESIAN_POINT ( 'NONE',  ( -165.3973046169136012, 70.03596893647589638, -94.69675437945477370 ) ) ;
#26730 = CARTESIAN_POINT ( 'NONE',  ( -86.69597344681494633, 1.750000000000009992, -159.1817124430720298 ) ) ;
#26731 = VERTEX_POINT ( 'NONE', #17096 ) ;
#26732 = ADVANCED_FACE ( 'NONE', ( #28148 ), #12234, .F. ) ;
#26733 = ORIENTED_EDGE ( 'NONE', *, *, #7078, .F. ) ;
#26734 = DIRECTION ( 'NONE',  ( -0.9976107099581958959, 4.447988690094345558E-15, 0.06908597091091805975 ) ) ;
#26735 = LINE ( 'NONE', #42367, #49835 ) ;
#26736 = VECTOR ( 'NONE', #11058, 1000.000000000000000 ) ;
#26737 = CARTESIAN_POINT ( 'NONE',  ( 1.962558162476984114, -3.366505435497487042, 9.741991644047251597 ) ) ;
#26738 = CARTESIAN_POINT ( 'NONE',  ( 155.0540265531850537, 1.025126265847089435, 2.568287556927986159 ) ) ;
#26739 = CARTESIAN_POINT ( 'NONE',  ( 35.00000000000186162, 17.00000000000000000, 65.00000000000000000 ) ) ;
#26740 =( GEOMETRIC_REPRESENTATION_CONTEXT ( 3 ) GLOBAL_UNCERTAINTY_ASSIGNED_CONTEXT ( ( #996 ) ) GLOBAL_UNIT_ASSIGNED_CONTEXT ( ( #25917, #30018, #26151 ) ) REPRESENTATION_CONTEXT ( 'NONE', 'WORKASPACE' ) );
#26741 = CARTESIAN_POINT ( 'NONE',  ( -168.4459734468149463, 0.000000000000000000, -120.9317124430720156 ) ) ;
#26742 = ORIENTED_EDGE ( 'NONE', *, *, #37262, .T. ) ;
#26743 = CARTESIAN_POINT ( 'NONE',  ( 49.46074318306830975, -9.578883844006833570, 8.807470649214879543 ) ) ;
#26744 = CARTESIAN_POINT ( 'NONE',  ( 1.057156451998911839, -0.7920882637786250680, 9.943883492372851407 ) ) ;
#26745 = VECTOR ( 'NONE', #34996, 1000.000000000000000 ) ;
#26746 = FACE_OUTER_BOUND ( 'NONE', #17371, .T. ) ;
#26747 = ORIENTED_EDGE ( 'NONE', *, *, #10598, .F. ) ;
#26748 = CARTESIAN_POINT ( 'NONE',  ( -543.3973046169135159, -62.56198943095993315, -177.1374399499827916 ) ) ;
#26749 = ORIENTED_EDGE ( 'NONE', *, *, #7485, .F. ) ;
#26750 = DIRECTION ( 'NONE',  ( -0.000000000000000000, -1.000000000000000000, -0.000000000000000000 ) ) ;
#26751 = CARTESIAN_POINT ( 'NONE',  ( 164.9999999999999716, -272.5000000000000000, -99.00000000000014211 ) ) ;
#26752 = CARTESIAN_POINT ( 'NONE',  ( 191.5540265531851105, 0.000000000000000000, -157.4317124430720582 ) ) ;
#26753 = ORIENTED_EDGE ( 'NONE', *, *, #1857, .F. ) ;
#26754 = LINE ( 'NONE', #50557, #18759 ) ;
#26755 = AXIS2_PLACEMENT_3D ( 'NONE', #6203, #41092, #36513 ) ;
#26756 = DIRECTION ( 'NONE',  ( -0.000000000000000000, -0.2791762785758810095, 0.9602398687205827565 ) ) ;
#26757 = EDGE_LOOP ( 'NONE', ( #17903, #12531, #19321, #4575, #85, #29184 ) ) ;
#26758 = CARTESIAN_POINT ( 'NONE',  ( 1.873480598308087330, -3.275918692700725110, 9.865049507598753209 ) ) ;
#26759 = MECHANICAL_DESIGN_GEOMETRIC_PRESENTATION_REPRESENTATION (  '', ( #15308 ), #39894 ) ;
#26760 = FACE_OUTER_BOUND ( 'NONE', #7071, .T. ) ;
#26761 = DIRECTION ( 'NONE',  ( -1.000000000000000000, 0.000000000000000000, 0.000000000000000000 ) ) ;
#26762 = ORIENTED_EDGE ( 'NONE', *, *, #19758, .F. ) ;
#26763 = VERTEX_POINT ( 'NONE', #40199 ) ;
#26764 = CARTESIAN_POINT ( 'NONE',  ( -5.297167662385172449, -5.958617466648796324, 3.455894424797545383E-16 ) ) ;
#26765 = CARTESIAN_POINT ( 'NONE',  ( 0.000000000000000000, 0.000000000000000000, 0.000000000000000000 ) ) ;
#26766 =( BOUNDED_CURVE ( )  B_SPLINE_CURVE ( 3, ( #31379, #12123, #11104, #50299 ),
 .UNSPECIFIED., .F., .F. ) 
 B_SPLINE_CURVE_WITH_KNOTS ( ( 4, 4 ),
 ( 4.712388980384689674, 6.283185307179586232 ),
 .UNSPECIFIED. ) 
 CURVE ( )  GEOMETRIC_REPRESENTATION_ITEM ( )  RATIONAL_B_SPLINE_CURVE ( ( 1.000000000000000000, 0.8047378541243649375, 0.8047378541243649375, 1.000000000000000000 ) ) 
 REPRESENTATION_ITEM ( '' )  );
#26767 = ORIENTED_EDGE ( 'NONE', *, *, #8825, .T. ) ;
#26768 = EDGE_CURVE ( 'NONE', #2436, #46647, #27901, .T. ) ;
#26769 = ORIENTED_EDGE ( 'NONE', *, *, #12063, .F. ) ;
#26770 = FACE_OUTER_BOUND ( 'NONE', #39820, .T. ) ;
#26771 = DIRECTION ( 'NONE',  ( 1.000000000000000000, -4.758098676964957447E-16, 2.958228394578795584E-31 ) ) ;
#26772 = CARTESIAN_POINT ( 'NONE',  ( -164.9999999999994031, 17.00000000000000000, -54.99999999999999289 ) ) ;
#26773 = EDGE_LOOP ( 'NONE', ( #47902, #22956, #23334, #16117, #10718, #13071 ) ) ;
#26774 = CARTESIAN_POINT ( 'NONE',  ( -1.224837355095377500, -1.100071488488243876, 9.927568724237806563 ) ) ;
#26775 = EDGE_CURVE ( 'NONE', #29100, #2097, #19735, .T. ) ;
#26776 = ORIENTED_EDGE ( 'NONE', *, *, #25021, .F. ) ;
#26777 =( BOUNDED_CURVE ( )  B_SPLINE_CURVE ( 3, ( #4915, #20573, #41084, #36500 ),
 .UNSPECIFIED., .F., .F. ) 
 B_SPLINE_CURVE_WITH_KNOTS ( ( 4, 4 ),
 ( 0.000000000000000000, 1.570796326794896558 ),
 .UNSPECIFIED. ) 
 CURVE ( )  GEOMETRIC_REPRESENTATION_ITEM ( )  RATIONAL_B_SPLINE_CURVE ( ( 1.000000000000000000, 0.8047378541243649375, 0.8047378541243649375, 1.000000000000000000 ) ) 
 REPRESENTATION_ITEM ( '' )  );
#26778 = CARTESIAN_POINT ( 'NONE',  ( 210.0000000000000568, 0.000000000000000000, 120.8182875569279702 ) ) ;
#26779 = EDGE_CURVE ( 'NONE', #8816, #23986, #23329, .T. ) ;
#26780 = CIRCLE ( 'NONE', #7111, 4.000000000000003553 ) ;
#26781 = CARTESIAN_POINT ( 'NONE',  ( -10.49999999999999467, -46.40197772635232099, 5.828307196921264755 ) ) ;
#26782 = EDGE_CURVE ( 'NONE', #27194, #38568, #16446, .T. ) ;
#26783 = CARTESIAN_POINT ( 'NONE',  ( 195.9526953830863079, -290.4457172416107937, 144.9816133044550668 ) ) ;
#26784 = ORIENTED_EDGE ( 'NONE', *, *, #29028, .T. ) ;
#26785 = ORIENTED_EDGE ( 'NONE', *, *, #11371, .T. ) ;
#26786 = EDGE_LOOP ( 'NONE', ( #36980, #36462, #50574, #24165, #4747, #4324 ) ) ;
#26787 = FACE_OUTER_BOUND ( 'NONE', #11252, .T. ) ;
#26788 = CARTESIAN_POINT ( 'NONE',  ( 73.30402655318508209, -1.750000000000010214, 40.81828755692798438 ) ) ;
#26789 = ORIENTED_EDGE ( 'NONE', *, *, #306, .T. ) ;
#26790 = CARTESIAN_POINT ( 'NONE',  ( -1.320835335343009787, 0.01943189458965158267, 9.943883492372876276 ) ) ;
#26791 = ORIENTED_EDGE ( 'NONE', *, *, #7993, .F. ) ;
#26792 = DIRECTION ( 'NONE',  ( 0.000000000000000000, 0.000000000000000000, 1.000000000000000000 ) ) ;
#26793 = ORIENTED_EDGE ( 'NONE', *, *, #3883, .F. ) ;
#26794 = CARTESIAN_POINT ( 'NONE',  ( -12.97493236725075683, 11.05939663307000664, 8.953103998512858652 ) ) ;
#26795 = CYLINDRICAL_SURFACE ( 'NONE', #1475, 1.750000000000008438 ) ;
#26796 = PLANE ( 'NONE',  #46486 ) ;
#26797 = CYLINDRICAL_SURFACE ( 'NONE', #19556, 1.750000000000001554 ) ;
#26798 = AXIS2_PLACEMENT_3D ( 'NONE', #6894, #8169, #31269 ) ;
#26799 = CARTESIAN_POINT ( 'NONE',  ( -15.00000000000001421, 16.00000000000000000, -114.9999999999999858 ) ) ;
#26800 = ORIENTED_EDGE ( 'NONE', *, *, #27225, .T. ) ;
#26801 = DIRECTION ( 'NONE',  ( 0.000000000000000000, 0.2223603367690632493, 0.9749645535258955054 ) ) ;
#26802 = FACE_OUTER_BOUND ( 'NONE', #22586, .T. ) ;
#26803 = DIRECTION ( 'NONE',  ( -1.000000000000000000, 7.930164457481157120E-16, -1.587271980518778491E-16 ) ) ;
#26804 = CARTESIAN_POINT ( 'NONE',  ( 232.4999999999999716, -169.9999999999999716, 32.29650858650035161 ) ) ;
#26805 = EDGE_CURVE ( 'NONE', #18208, #3827, #16340, .T. ) ;
#26806 = EDGE_CURVE ( 'NONE', #34694, #17244, #48098, .T. ) ;
#26807 = ADVANCED_FACE ( 'NONE', ( #35864 ), #43782, .T. ) ;
#26808 = EDGE_CURVE ( 'NONE', #38906, #43683, #49104, .T. ) ;
#26809 = DIRECTION ( 'NONE',  ( 1.000000000000000000, 0.000000000000000000, 0.000000000000000000 ) ) ;
#26810 = CARTESIAN_POINT ( 'NONE',  ( -29.61572577327014955, -16.11461842845715253, 8.807470649214879543 ) ) ;
#26811 = EDGE_CURVE ( 'NONE', #12229, #10849, #22211, .T. ) ;
#26812 = ORIENTED_EDGE ( 'NONE', *, *, #32471, .F. ) ;
#26813 = LINE ( 'NONE', #49348, #10630 ) ;
#26814 = ADVANCED_FACE ( 'NONE', ( #29652 ), #41193, .T. ) ;
#26815 = PLANE ( 'NONE',  #3339 ) ;
#26816 = ORIENTED_EDGE ( 'NONE', *, *, #28846, .T. ) ;
#26817 = DIRECTION ( 'NONE',  ( 0.000000000000000000, 0.000000000000000000, -1.000000000000000000 ) ) ;
#26818 = DIRECTION ( 'NONE',  ( -1.000000000000000000, 0.000000000000000000, 0.000000000000000000 ) ) ;
#26819 = CARTESIAN_POINT ( 'NONE',  ( 357.9999999999999432, -174.9999999999999716, 355.9999999999998295 ) ) ;
#26820 = ORIENTED_EDGE ( 'NONE', *, *, #37276, .F. ) ;
#26821 = ORIENTED_EDGE ( 'NONE', *, *, #8416, .F. ) ;
#26822 = EDGE_CURVE ( 'NONE', #39178, #16051, #17599, .T. ) ;
#26823 = CARTESIAN_POINT ( 'NONE',  ( -8.277096487746778308, 33.14818118907697198, 7.455576670931136185 ) ) ;
#26824 = ADVANCED_FACE ( 'NONE', ( #25300 ), #18097, .T. ) ;
#26825 = AXIS2_PLACEMENT_3D ( 'NONE', #22802, #43309, #38724 ) ;
#26826 = EDGE_LOOP ( 'NONE', ( #50074, #6150, #45134, #41425, #15403, #11851 ) ) ;
#26827 = EDGE_CURVE ( 'NONE', #36974, #9702, #21376, .T. ) ;
#26828 = ORIENTED_EDGE ( 'NONE', *, *, #40658, .F. ) ;
#26829 = CARTESIAN_POINT ( 'NONE',  ( 15.00099850811936264, 7.462898891544210933, 9.403735324607438884 ) ) ;
#26830 = LINE ( 'NONE', #30165, #21638 ) ;
#26831 = CARTESIAN_POINT ( 'NONE',  ( 193.3040265531851105, -1.750000000000010214, -39.18171244307202983 ) ) ;
#26832 = ORIENTED_EDGE ( 'NONE', *, *, #11357, .T. ) ;
#26833 = ORIENTED_EDGE ( 'NONE', *, *, #11138, .F. ) ;
#26834 = ORIENTED_EDGE ( 'NONE', *, *, #13949, .T. ) ;
#26835 = CARTESIAN_POINT ( 'NONE',  ( -49.67735855322972327, 8.912210285362091255, 8.356839323120299312 ) ) ;
#26836 = CARTESIAN_POINT ( 'NONE',  ( 210.0000000000000568, 2.143131898507881856E-16, 79.06828755692797017 ) ) ;
#26837 = VERTEX_POINT ( 'NONE', #13493 ) ;
#26838 = DIRECTION ( 'NONE',  ( 3.172065745548403743E-16, 1.000000000000000000, 0.000000000000000000 ) ) ;
#26839 = SURFACE_STYLE_USAGE ( .BOTH. , #14783 ) ;
#26840 = VERTEX_POINT ( 'NONE', #2697 ) ;
#26841 = ORIENTED_EDGE ( 'NONE', *, *, #46269, .F. ) ;
#26842 = CARTESIAN_POINT ( 'NONE',  ( -4.945973446814903696, 2.143131898507912917E-16, 165.0000000000000000 ) ) ;
#26843 = EDGE_CURVE ( 'NONE', #7812, #6992, #37387, .T. ) ;
#26844 = DIRECTION ( 'NONE',  ( 0.000000000000000000, 0.000000000000000000, 1.000000000000000000 ) ) ;
#26845 = CARTESIAN_POINT ( 'NONE',  ( 3.414233368894302068, 9.411746240900633609, 6.185594734181435683 ) ) ;
#26846 = VERTEX_POINT ( 'NONE', #10409 ) ;
#26847 = VERTEX_POINT ( 'NONE', #5801 ) ;
#26848 = LINE ( 'NONE', #27624, #37322 ) ;
#26849 = CARTESIAN_POINT ( 'NONE',  ( 151.5540265531850537, 0.000000000000000000, -120.9317124430720156 ) ) ;
#26850 = DIRECTION ( 'NONE',  ( -1.000000000000000000, 0.000000000000000000, 0.000000000000000000 ) ) ;
#26851 = CARTESIAN_POINT ( 'NONE',  ( -165.0000000000000284, 16.00000000000000000, -90.00000000000000000 ) ) ;
#26852 = ADVANCED_FACE ( 'NONE', ( #45018 ), #41455, .F. ) ;
#26853 = CARTESIAN_POINT ( 'NONE',  ( -1.142975459103954705, -16.61830776097024653, -2.870787844569587133 ) ) ;
#26854 = ORIENTED_EDGE ( 'NONE', *, *, #49601, .T. ) ;
#26855 = DIRECTION ( 'NONE',  ( 0.000000000000000000, -0.3846153846153845812, -0.9230769230769231282 ) ) ;
#26856 = DIRECTION ( 'NONE',  ( 0.000000000000000000, -0.000000000000000000, 1.000000000000000000 ) ) ;
#26857 = DIRECTION ( 'NONE',  ( -0.000000000000000000, -0.000000000000000000, -1.000000000000000000 ) ) ;
#26858 = LINE ( 'NONE', #7366, #32076 ) ;
#26859 = EDGE_CURVE ( 'NONE', #18811, #26282, #48349, .T. ) ;
#26860 = ADVANCED_FACE ( 'NONE', ( #21194 ), #9899, .T. ) ;
#26861 = FACE_OUTER_BOUND ( 'NONE', #29112, .T. ) ;
#26862 = ORIENTED_EDGE ( 'NONE', *, *, #222, .T. ) ;
#26863 = FACE_OUTER_BOUND ( 'NONE', #43935, .T. ) ;
#26864 = EDGE_CURVE ( 'NONE', #46895, #29584, #21679, .T. ) ;
#26865 = CARTESIAN_POINT ( 'NONE',  ( 32.27890028733795447, -1.750000000000010214, 79.79316129108087807 ) ) ;
#26866 = CARTESIAN_POINT ( 'NONE',  ( 1.468713901642212161, 0.3220470327672588229, 9.927319414211225990 ) ) ;
#26867 = ADVANCED_FACE ( 'NONE', ( #29159 ), #44518, .F. ) ;
#26868 = EDGE_CURVE ( 'NONE', #9910, #980, #33275, .T. ) ;
#26869 = EDGE_LOOP ( 'NONE', ( #49613, #39924, #26017, #11641 ) ) ;
#26870 = DIRECTION ( 'NONE',  ( 0.000000000000000000, 0.000000000000000000, 1.000000000000000000 ) ) ;
#26871 = CARTESIAN_POINT ( 'NONE',  ( 341.6568542494924827, 185.0000000000000568, 359.9999999999998295 ) ) ;
#26872 = ORIENTED_EDGE ( 'NONE', *, *, #20315, .F. ) ;
#26873 = LINE ( 'NONE', #49668, #38636 ) ;
#26874 = CARTESIAN_POINT ( 'NONE',  ( 355.9999999999999432, 183.0000000000002558, -358.0000000000003411 ) ) ;
#26875 = CARTESIAN_POINT ( 'NONE',  ( -204.9459734468149463, 2.143131898507880377E-16, 165.0000000000000000 ) ) ;
#26876 = CARTESIAN_POINT ( 'NONE',  ( -0.1475726264153620626, -1.496347932843211215, 9.927319414211227766 ) ) ;
#26877 = EDGE_CURVE ( 'NONE', #14899, #3733, #36842, .T. ) ;
#26878 = VERTEX_POINT ( 'NONE', #33770 ) ;
#26879 = B_SPLINE_SURFACE_WITH_KNOTS ( 'NONE', 3, 3, ( 
 ( #47791, #28337, #43969, #36310 ),
 ( #13687, #6258, #9344, #44465 ),
 ( #14178, #40892, #29592, #29851 ),
 ( #9593, #28841, #37328, #17291 ) ),
 .UNSPECIFIED., .F., .F., .F.,
 ( 4, 4 ),
 ( 4, 4 ),
 ( 0.000000000000000000, 1.000000000000000000 ),
 ( 0.000000000000000000, 1.000000000000000000 ),
 .UNSPECIFIED. ) ;
#26880 = EDGE_LOOP ( 'NONE', ( #12931, #37095, #20208, #9154, #24541, #27736 ) ) ;
#26881 = ORIENTED_EDGE ( 'NONE', *, *, #43990, .F. ) ;
#26882 = LINE ( 'NONE', #3514, #29561 ) ;
#26883 = ORIENTED_EDGE ( 'NONE', *, *, #44981, .T. ) ;
#26884 = CARTESIAN_POINT ( 'NONE',  ( 1.962558162476984114, -3.366505435497487042, 9.741991644047251597 ) ) ;
#26885 = PLANE ( 'NONE',  #15900 ) ;
#26886 = DIRECTION ( 'NONE',  ( 0.000000000000000000, -1.000000000000000000, 8.673617379884027583E-15 ) ) ;
#26887 = DIRECTION ( 'NONE',  ( 0.000000000000000000, -0.3846153846153844702, 0.9230769230769231282 ) ) ;
#26888 = VERTEX_POINT ( 'NONE', #30940 ) ;
#26889 = DIRECTION ( 'NONE',  ( -1.000000000000000000, 0.000000000000000000, 0.000000000000000000 ) ) ;
#26890 = CARTESIAN_POINT ( 'NONE',  ( 168.9999999999999716, -272.4999999999999432, -339.9999999999998863 ) ) ;
#26891 = CARTESIAN_POINT ( 'NONE',  ( -6.174150299305392053, 50.00000000000000000, 8.807470649214879543 ) ) ;
#26892 = EDGE_LOOP ( 'NONE', ( #35877, #41877, #41031, #30477, #33195, #44038, #153, #45048 ) ) ;
#26893 = VECTOR ( 'NONE', #43003, 1000.000000000000000 ) ;
#26894 = FACE_OUTER_BOUND ( 'NONE', #42783, .T. ) ;
#26895 = CARTESIAN_POINT ( 'NONE',  ( -194.9999999999999432, 164.9999999999999716, 500.0000000000000000 ) ) ;
#26896 = EDGE_LOOP ( 'NONE', ( #12813, #7535, #49159, #19399 ) ) ;
#26897 = ORIENTED_EDGE ( 'NONE', *, *, #5165, .F. ) ;
#26898 = ORIENTED_EDGE ( 'NONE', *, *, #29379, .T. ) ;
#26899 = CARTESIAN_POINT ( 'NONE',  ( -114.9999999999994031, 16.00000000000000000, -54.99999999999999289 ) ) ;
#26900 = DIRECTION ( 'NONE',  ( 0.000000000000000000, 0.000000000000000000, -1.000000000000000000 ) ) ;
#26901 = B_SPLINE_CURVE_WITH_KNOTS ( 'NONE', 3,
 ( #29759, #13833, #34136, #49714 ),
 .UNSPECIFIED., .F., .F.,
 ( 4, 4 ),
 ( 2.453269466693398698E-18, 0.002466147708923231013 ),
 .UNSPECIFIED. ) ;
#26902 = VERTEX_POINT ( 'NONE', #7315 ) ;
#26903 = CARTESIAN_POINT ( 'NONE',  ( -5.647304616913629616, 47.08801056904012228, 741.9425600500172777 ) ) ;
#26904 = CARTESIAN_POINT ( 'NONE',  ( -8.445973446814976526, 0.000000000000000000, -120.9317124430720725 ) ) ;
#26905 =( BOUNDED_CURVE ( )  B_SPLINE_CURVE ( 3, ( #47633, #28441, #16131, #23831 ),
 .UNSPECIFIED., .F., .F. ) 
 B_SPLINE_CURVE_WITH_KNOTS ( ( 4, 4 ),
 ( 1.570796326794896558, 3.141592653589793116 ),
 .UNSPECIFIED. ) 
 CURVE ( )  GEOMETRIC_REPRESENTATION_ITEM ( )  RATIONAL_B_SPLINE_CURVE ( ( 1.000000000000000000, 0.8047378541243649375, 0.8047378541243649375, 1.000000000000000000 ) ) 
 REPRESENTATION_ITEM ( '' )  );
#26906 = CARTESIAN_POINT ( 'NONE',  ( 168.9999999999999716, -272.4999999999999432, -357.9999999999999432 ) ) ;
#26907 = CARTESIAN_POINT ( 'NONE',  ( 130.0000000000002842, 17.00000000000000000, -60.00000000000000000 ) ) ;
#26908 = LINE ( 'NONE', #11520, #27959 ) ;
#26909 = CARTESIAN_POINT ( 'NONE',  ( 210.0000000000000568, 2.143131898507881856E-16, -120.9317124430720582 ) ) ;
#26910 = DIRECTION ( 'NONE',  ( -1.000000000000000000, 0.000000000000000000, 0.000000000000000000 ) ) ;
#26911 = DIRECTION ( 'NONE',  ( -0.000000000000000000, -0.000000000000000000, -1.000000000000000000 ) ) ;
#26912 = CARTESIAN_POINT ( 'NONE',  ( 1.011271242968683648, 0.7347315653655930312, 10.00000000000000000 ) ) ;
#26913 = CARTESIAN_POINT ( 'NONE',  ( -21.61731705588949737, -25.43568671410585935, -9.367992836599954742 ) ) ;
#26914 = ORIENTED_EDGE ( 'NONE', *, *, #16232, .T. ) ;
#26915 = LINE ( 'NONE', #27180, #1949 ) ;
#26916 = DIRECTION ( 'NONE',  ( -0.4740998230350175202, 0.3386427307392980701, -0.8127425537743157014 ) ) ;
#26917 = ADVANCED_FACE ( 'NONE', ( #15520 ), #50622, .T. ) ;
#26918 = EDGE_CURVE ( 'NONE', #50401, #26389, #49606, .T. ) ;
#26919 = DIRECTION ( 'NONE',  ( -1.000000000000000000, 0.000000000000000000, -2.958228394578794270E-31 ) ) ;
#26920 = ORIENTED_EDGE ( 'NONE', *, *, #27860, .T. ) ;
#26921 = CARTESIAN_POINT ( 'NONE',  ( 344.0000000000000568, 181.0000000000000284, 349.9999999999998295 ) ) ;
#26922 = FACE_OUTER_BOUND ( 'NONE', #31816, .T. ) ;
#26923 =( BOUNDED_CURVE ( )  B_SPLINE_CURVE ( 3, ( #41967, #20513, #44583, #21516 ),
 .UNSPECIFIED., .F., .F. ) 
 B_SPLINE_CURVE_WITH_KNOTS ( ( 4, 4 ),
 ( 3.141592653589793116, 4.712388980384703885 ),
 .UNSPECIFIED. ) 
 CURVE ( )  GEOMETRIC_REPRESENTATION_ITEM ( )  RATIONAL_B_SPLINE_CURVE ( ( 1.000000000000000000, 0.8047378541243617178, 0.8047378541243617178, 1.000000000000000000 ) ) 
 REPRESENTATION_ITEM ( '' )  );
#26924 = ADVANCED_FACE ( 'NONE', ( #30158, #38379 ), #46771, .T. ) ;
#26925 = CARTESIAN_POINT ( 'NONE',  ( 111.5540265531850537, -1.025126265847081442, -160.9317124430720014 ) ) ;
#26926 = CARTESIAN_POINT ( 'NONE',  ( -65.00000000000002842, 17.00000000000000000, -90.00000000000000000 ) ) ;
#26927 = LINE ( 'NONE', #15127, #49996 ) ;
#26928 = EDGE_CURVE ( 'NONE', #36302, #31660, #7840, .T. ) ;
#26929 = EDGE_CURVE ( 'NONE', #40517, #2086, #15280, .T. ) ;
#26930 = ORIENTED_EDGE ( 'NONE', *, *, #25813, .F. ) ;
#26931 = FACE_OUTER_BOUND ( 'NONE', #4616, .T. ) ;
#26933 = ORIENTED_EDGE ( 'NONE', *, *, #24034, .T. ) ;
#26932 = VECTOR ( 'NONE', #27885, 1000.000000000000000 ) ;
#26934 = CARTESIAN_POINT ( 'NONE',  ( 339.9999999999999432, 165.0000000000000000, -344.0000000000001705 ) ) ;
#26935 = ORIENTED_EDGE ( 'NONE', *, *, #32772, .F. ) ;
#26936 = EDGE_CURVE ( 'NONE', #28100, #31529, #5003, .T. ) ;
#26937 = DIRECTION ( 'NONE',  ( 0.000000000000000000, 0.000000000000000000, -1.000000000000000000 ) ) ;
#26938 = CARTESIAN_POINT ( 'NONE',  ( 210.0000000000000568, 0.000000000000000000, 162.5682875569279702 ) ) ;
#26939 = EDGE_CURVE ( 'NONE', #27665, #41907, #41957, .T. ) ;
#26940 = ORIENTED_EDGE ( 'NONE', *, *, #22110, .F. ) ;
#26941 = PRESENTATION_STYLE_ASSIGNMENT (( #46408 ) ) ;
#26942 = VECTOR ( 'NONE', #14143, 1000.000000000000000 ) ;
#26943 = ORIENTED_EDGE ( 'NONE', *, *, #12596, .T. ) ;
#26944 = ORIENTED_EDGE ( 'NONE', *, *, #27740, .F. ) ;
#26945 = CARTESIAN_POINT ( 'NONE',  ( 191.5540265531851105, 0.000000000000000000, 82.56828755692798438 ) ) ;
#26946 = VERTEX_POINT ( 'NONE', #11418 ) ;
#26947 = CARTESIAN_POINT ( 'NONE',  ( -13.59579750444763668, 10.60877755095910935, 8.727788335465566760 ) ) ;
#26948 = CARTESIAN_POINT ( 'NONE',  ( -204.9459734468149463, 2.143131898507880377E-16, -160.9317124430720014 ) ) ;
#26949 = CARTESIAN_POINT ( 'NONE',  ( -44.94597344681493922, 2.143131898507880377E-16, 2.568287556927978166 ) ) ;
#26950 = ORIENTED_EDGE ( 'NONE', *, *, #2594, .F. ) ;
#26951 = VERTEX_POINT ( 'NONE', #38633 ) ;
#26952 = DIRECTION ( 'NONE',  ( 0.000000000000000000, -2.265761274745217480E-16, 1.000000000000000000 ) ) ;
#26953 = CARTESIAN_POINT ( 'NONE',  ( -165.3973046169136012, 103.9380105690400597, -17.65743994998277699 ) ) ;
#26954 = ORIENTED_EDGE ( 'NONE', *, *, #9948, .T. ) ;
#26955 = LINE ( 'NONE', #50001, #26725 ) ;
#26956 = CARTESIAN_POINT ( 'NONE',  ( -214.9999999999999432, -172.9999999999999716, 232.0000000000000284 ) ) ;
#26957 = VERTEX_POINT ( 'NONE', #3449 ) ;
#26958 = LINE ( 'NONE', #39035, #46636 ) ;
#26959 = EDGE_CURVE ( 'NONE', #47057, #7107, #39092, .T. ) ;
#26960 = CYLINDRICAL_SURFACE ( 'NONE', #32503, 5.000000000000000000 ) ;
#26961 = ORIENTED_EDGE ( 'NONE', *, *, #11657, .F. ) ;
#26962 = EDGE_CURVE ( 'NONE', #49029, #50662, #22722, .T. ) ;
#26963 = DIRECTION ( 'NONE',  ( 0.000000000000000000, 1.000000000000000000, 6.123233995736766036E-17 ) ) ;
#26964 = CIRCLE ( 'NONE', #15504, 22.00000000000000000 ) ;
#26965 = CARTESIAN_POINT ( 'NONE',  ( -16.73672383626882976, -2.341008440547992731, -9.008049429158102583 ) ) ;
#26966 = PLANE ( 'NONE',  #23836 ) ;
#26967 = PLANE ( 'NONE',  #10798 ) ;
#26968 = VECTOR ( 'NONE', #43636, 1000.000000000000000 ) ;
#26969 = ORIENTED_EDGE ( 'NONE', *, *, #16565, .T. ) ;
#26970 = CARTESIAN_POINT ( 'NONE',  ( 16.16402646813543242, -4.033894069732437693, -3.546734833711462365 ) ) ;
#26971 = CIRCLE ( 'NONE', #36011, 0.5000000000000004441 ) ;
#26972 = VECTOR ( 'NONE', #28234, 1000.000000000000000 ) ;
#26973 = CARTESIAN_POINT ( 'NONE',  ( 168.9999999999999716, -79.49999999999997158, -350.0000000000001705 ) ) ;
#26974 = VECTOR ( 'NONE', #8451, 1000.000000000000000 ) ;
#26975 = CARTESIAN_POINT ( 'NONE',  ( 15.00099850811936264, 7.462898891544210933, 9.403735324607438884 ) ) ;
#26976 = VERTEX_POINT ( 'NONE', #34022 ) ;
#26977 = ORIENTED_EDGE ( 'NONE', *, *, #5796, .F. ) ;
#26979 = LINE ( 'NONE', #43376, #4013 ) ;
#26978 = AXIS2_PLACEMENT_3D ( 'NONE', #15210, #14952, #42893 ) ;
#26980 = FACE_OUTER_BOUND ( 'NONE', #42156, .T. ) ;
#26981 = DIRECTION ( 'NONE',  ( 1.000000000000000000, 0.000000000000000000, 0.000000000000000000 ) ) ;
#26982 = CARTESIAN_POINT ( 'NONE',  ( 210.0000000000000568, 2.143131898507881856E-16, 119.0682875569279560 ) ) ;
#26983 = DIRECTION ( 'NONE',  ( 0.000000000000000000, 1.000000000000000000, 0.000000000000000000 ) ) ;
#26984 = ORIENTED_EDGE ( 'NONE', *, *, #40688, .T. ) ;
#26985 = CARTESIAN_POINT ( 'NONE',  ( 154.3291528190321458, 1.750000000000009548, 39.79316129108089228 ) ) ;
#26986 = PRODUCT_DEFINITION_SHAPE ( 'NONE', 'NONE',  #50730 ) ;
#26987 = CARTESIAN_POINT ( 'NONE',  ( 0.2450692849603075263, -0.3373089330821618104, 9.992737347336294818 ) ) ;
#26988 = CARTESIAN_POINT ( 'NONE',  ( 34.38161489319228536, -14.98878603239685070, -8.600750091277035381 ) ) ;
#26989 = CARTESIAN_POINT ( 'NONE',  ( -168.4459734468149747, 1.025126265847089435, 82.56828755692798438 ) ) ;
#26990 = EDGE_LOOP ( 'NONE', ( #17223, #49728, #2660, #10625, #15846, #44221 ) ) ;
#26991 = LINE ( 'NONE', #16214, #43362 ) ;
#26992 = LINE ( 'NONE', #7507, #791 ) ;
#26993 = VERTEX_POINT ( 'NONE', #2945 ) ;
#26994 = EDGE_CURVE ( 'NONE', #32522, #16517, #19102, .T. ) ;
#26995 = CARTESIAN_POINT ( 'NONE',  ( -46.69597344681494633, 0.000000000000000000, 165.0000000000000000 ) ) ;
#26996 = DIRECTION ( 'NONE',  ( -1.000000000000000000, -0.000000000000000000, -0.000000000000000000 ) ) ;
#26997 = DIRECTION ( 'NONE',  ( -1.000000000000000000, -0.000000000000000000, -0.000000000000000000 ) ) ;
#26998 = VECTOR ( 'NONE', #19488, 1000.000000000000000 ) ;
#26999 = ORIENTED_EDGE ( 'NONE', *, *, #49536, .T. ) ;
#27000 = AXIS2_PLACEMENT_3D ( 'NONE', #24174, #9017, #28268 ) ;
#27001 = AXIS2_PLACEMENT_3D ( 'NONE', #890, #40137, #40639 ) ;
#27002 = CARTESIAN_POINT ( 'NONE',  ( 432.7825420346616170, 74.83106485270648989, -120.5992382549688955 ) ) ;
#27003 = CARTESIAN_POINT ( 'NONE',  ( 130.0000000000018474, 16.00000000000000000, 65.00000000000000000 ) ) ;
#27004 = ORIENTED_EDGE ( 'NONE', *, *, #1726, .T. ) ;
#27005 = CARTESIAN_POINT ( 'NONE',  ( -1.780557400379564337, -1.041314823045429661, 9.889206917020301191 ) ) ;
#27006 =( BOUNDED_CURVE ( )  B_SPLINE_CURVE ( 3, ( #12934, #37080, #43733, #910 ),
 .UNSPECIFIED., .F., .F. ) 
 B_SPLINE_CURVE_WITH_KNOTS ( ( 4, 4 ),
 ( 1.570796326794896558, 3.141592653589793116 ),
 .UNSPECIFIED. ) 
 CURVE ( )  GEOMETRIC_REPRESENTATION_ITEM ( )  RATIONAL_B_SPLINE_CURVE ( ( 1.000000000000000000, 0.8047378541243649375, 0.8047378541243649375, 1.000000000000000000 ) ) 
 REPRESENTATION_ITEM ( '' )  );
#27007 = DIRECTION ( 'NONE',  ( -0.000000000000000000, -0.000000000000000000, 1.000000000000000000 ) ) ;
#27008 = UNCERTAINTY_MEASURE_WITH_UNIT (LENGTH_MEASURE( 1.000000000000000082E-05 ), #18758, 'distance_accuracy_value', 'NONE');
#27009 = LINE ( 'NONE', #22902, #11115 ) ;
#27010 = ORIENTED_EDGE ( 'NONE', *, *, #17678, .F. ) ;
#27011 = ORIENTED_EDGE ( 'NONE', *, *, #38922, .T. ) ;
#27012 = CARTESIAN_POINT ( 'NONE',  ( 113.3040265531850537, -1.749999999999997335, -119.1817124430720440 ) ) ;
#27013 = DIRECTION ( 'NONE',  ( -1.000000000000000000, 0.000000000000000000, 0.000000000000000000 ) ) ;
#27014 = CIRCLE ( 'NONE', #8167, 4.000000000000003553 ) ;
#27015 = EDGE_LOOP ( 'NONE', ( #4427, #6768, #48270, #24240, #34043, #24962 ) ) ;
#27016 = ORIENTED_EDGE ( 'NONE', *, *, #46512, .F. ) ;
#27017 = CARTESIAN_POINT ( 'NONE',  ( -128.4459734468149463, -1.025126265847082108, -117.4317124430720440 ) ) ;
#27018 = CARTESIAN_POINT ( 'NONE',  ( -86.69597344681494633, 1.750000000000010658, -119.1817124430720440 ) ) ;
#27019 = FACE_OUTER_BOUND ( 'NONE', #3352, .T. ) ;
#27020 = ORIENTED_EDGE ( 'NONE', *, *, #26448, .F. ) ;
#27021 = LINE ( 'NONE', #15472, #12061 ) ;
#27022 = ORIENTED_EDGE ( 'NONE', *, *, #27402, .F. ) ;
#27023 = CARTESIAN_POINT ( 'NONE',  ( -175.0000000000000000, 0.000000000000000000, 122.5000000000000142 ) ) ;
#27024 = EDGE_CURVE ( 'NONE', #42417, #17157, #14757, .T. ) ;
#27025 = DIRECTION ( 'NONE',  ( 0.000000000000000000, 0.9152942571496521795, -0.4027858274925601445 ) ) ;
#27026 = CARTESIAN_POINT ( 'NONE',  ( 10.50000000000000178, -46.40197772635230677, 5.828307196921267419 ) ) ;
#27027 = ORIENTED_EDGE ( 'NONE', *, *, #13758, .T. ) ;
#27028 = ORIENTED_EDGE ( 'NONE', *, *, #44492, .T. ) ;
#27029 = ORIENTED_EDGE ( 'NONE', *, *, #32201, .F. ) ;
#27030 = DIRECTION ( 'NONE',  ( -1.000000000000000000, 0.000000000000000000, -0.000000000000000000 ) ) ;
#27031 = CARTESIAN_POINT ( 'NONE',  ( -16.91580242619126295, -33.50775492265634625, 4.835783797351798086 ) ) ;
#27032 = ORIENTED_EDGE ( 'NONE', *, *, #37256, .F. ) ;
#27033 = CARTESIAN_POINT ( 'NONE',  ( -88.44597344681494633, -1.025126265847089435, 39.06828755692797728 ) ) ;
#27035 = EDGE_LOOP ( 'NONE', ( #45911, #35518, #1269, #30637, #44969, #28029 ) ) ;
#27034 = VECTOR ( 'NONE', #6433, 1000.000000000000000 ) ;
#27036 = FACE_OUTER_BOUND ( 'NONE', #14151, .T. ) ;
#27038 = ORIENTED_EDGE ( 'NONE', *, *, #14286, .T. ) ;
#27037 = VECTOR ( 'NONE', #12541, 1000.000000000000000 ) ;
#27039 = SHAPE_REPRESENTATION_RELATIONSHIP ( 'NONE' , 'NONE' ,  #35275, #27107 ) ;
#27040 = DIRECTION ( 'NONE',  ( 7.793956916774525800E-48, 0.000000000000000000, 1.000000000000000000 ) ) ;
#27041 = B_SPLINE_CURVE_WITH_KNOTS ( 'NONE', 3,
 ( #19734, #42063, #3060, #7442 ),
 .UNSPECIFIED., .F., .F.,
 ( 4, 4 ),
 ( 0.000000000000000000, 0.002466147708923234483 ),
 .UNSPECIFIED. ) ;
#27042 = CARTESIAN_POINT ( 'NONE',  ( -31.94178169330213279, 9.256608784834037706, -3.760136334089591248 ) ) ;
#27043 = CARTESIAN_POINT ( 'NONE',  ( 355.9999999999999432, -165.0000000000001137, -106.0000000000001990 ) ) ;
#27044 = VECTOR ( 'NONE', #33453, 1000.000000000000000 ) ;
#27045 = LINE ( 'NONE', #3694, #2033 ) ;
#27046 = ORIENTED_EDGE ( 'NONE', *, *, #36702, .F. ) ;
#27047 = ORIENTED_EDGE ( 'NONE', *, *, #46824, .T. ) ;
#27049 = VECTOR ( 'NONE', #45049, 1000.000000000000000 ) ;
#27048 = FACE_OUTER_BOUND ( 'NONE', #45373, .T. ) ;
#27050 = LINE ( 'NONE', #40309, #15865 ) ;
#27051 = CARTESIAN_POINT ( 'NONE',  ( 355.9999999999999432, -185.0000000000000284, 359.9999999999998295 ) ) ;
#27052 = DIRECTION ( 'NONE',  ( -0.000000000000000000, -0.000000000000000000, 1.000000000000000000 ) ) ;
#27053 = AXIS2_PLACEMENT_3D ( 'NONE', #14896, #15148, #15655 ) ;
#27054 = FACE_OUTER_BOUND ( 'NONE', #42, .T. ) ;
#27055 = CARTESIAN_POINT ( 'NONE',  ( -45.21167770612412085, -22.65616271077779942, 7.906207997025717304 ) ) ;
#27056 = VERTEX_POINT ( 'NONE', #27066 ) ;
#27057 = EDGE_CURVE ( 'NONE', #33060, #4645, #3191, .T. ) ;
#27058 = CARTESIAN_POINT ( 'NONE',  ( 358.0000000000000568, -3.000000000000197176, -178.0000000000003979 ) ) ;
#27059 = FACE_OUTER_BOUND ( 'NONE', #49169, .T. ) ;
#27060 = EDGE_CURVE ( 'NONE', #7200, #20659, #46272, .T. ) ;
#27061 = ORIENTED_EDGE ( 'NONE', *, *, #44607, .F. ) ;
#27062 = EDGE_CURVE ( 'NONE', #10058, #22540, #7069, .T. ) ;
#27063 =( BOUNDED_CURVE ( )  B_SPLINE_CURVE ( 3, ( #11367, #3407, #3923, #38844 ),
 .UNSPECIFIED., .F., .F. ) 
 B_SPLINE_CURVE_WITH_KNOTS ( ( 4, 4 ),
 ( 0.000000000000000000, 1.570796326794896558 ),
 .UNSPECIFIED. ) 
 CURVE ( )  GEOMETRIC_REPRESENTATION_ITEM ( )  RATIONAL_B_SPLINE_CURVE ( ( 1.000000000000000000, 0.8047378541243649375, 0.8047378541243649375, 1.000000000000000000 ) ) 
 REPRESENTATION_ITEM ( '' )  );
#27064 = CARTESIAN_POINT ( 'NONE',  ( 210.0000000000000568, 0.000000000000000000, -39.18171244307202983 ) ) ;
#27065 = LINE ( 'NONE', #35051, #22065 ) ;
#27066 = CARTESIAN_POINT ( 'NONE',  ( 164.9999999999999716, 17.00000000000000000, -60.00000000000001421 ) ) ;
#27067 = ADVANCED_FACE ( 'NONE', ( #7575 ), #23209, .F. ) ;
#27068 =( BOUNDED_CURVE ( )  B_SPLINE_CURVE ( 3, ( #25543, #9641, #5023, #25049 ),
 .UNSPECIFIED., .F., .F. ) 
 B_SPLINE_CURVE_WITH_KNOTS ( ( 4, 4 ),
 ( 0.000000000000000000, 1.570796326794896558 ),
 .UNSPECIFIED. ) 
 CURVE ( )  GEOMETRIC_REPRESENTATION_ITEM ( )  RATIONAL_B_SPLINE_CURVE ( ( 1.000000000000000000, 0.8047378541243649375, 0.8047378541243649375, 1.000000000000000000 ) ) 
 REPRESENTATION_ITEM ( '' )  );
#27069 = EDGE_CURVE ( 'NONE', #24870, #4802, #45470, .T. ) ;
#27070 = ORIENTED_EDGE ( 'NONE', *, *, #43388, .T. ) ;
#27071 = ORIENTED_EDGE ( 'NONE', *, *, #29090, .F. ) ;
#27072 = FACE_OUTER_BOUND ( 'NONE', #45159, .T. ) ;
#27073 = CARTESIAN_POINT ( 'NONE',  ( -0.4166666666666669072, 0.000000000000000000, 10.00000000000000000 ) ) ;
#27074 = AXIS2_PLACEMENT_3D ( 'NONE', #3132, #14693, #10591 ) ;
#27075 = ADVANCED_FACE ( 'NONE', ( #9093 ), #35546, .T. ) ;
#27076 = AXIS2_PLACEMENT_3D ( 'NONE', #42127, #38318, #41386 ) ;
#27077 = ORIENTED_EDGE ( 'NONE', *, *, #35944, .T. ) ;
#27078 = VERTEX_POINT ( 'NONE', #24495 ) ;
#27079 = CARTESIAN_POINT ( 'NONE',  ( 45.21167770612395742, 22.65616271077811206, 7.906207997025717304 ) ) ;
#27080 = CARTESIAN_POINT ( 'NONE',  ( 194.9999999999999432, -173.0000000000000000, 132.0000000000000853 ) ) ;
#27081 = FACE_OUTER_BOUND ( 'NONE', #48768, .T. ) ;
#27082 = VERTEX_POINT ( 'NONE', #12677 ) ;
#27083 = ORIENTED_EDGE ( 'NONE', *, *, #49279, .F. ) ;
#27084 = VERTEX_POINT ( 'NONE', #8340 ) ;
#27085 = AXIS2_PLACEMENT_3D ( 'NONE', #17057, #16812, #29809 ) ;
#27086 =( GEOMETRIC_REPRESENTATION_CONTEXT ( 3 ) GLOBAL_UNCERTAINTY_ASSIGNED_CONTEXT ( ( #16902 ) ) GLOBAL_UNIT_ASSIGNED_CONTEXT ( ( #2311, #50216, #49475 ) ) REPRESENTATION_CONTEXT ( 'NONE', 'WORKASPACE' ) );
#27087 = EDGE_CURVE ( 'NONE', #5199, #30729, #47769, .T. ) ;
#27088 = EDGE_CURVE ( 'NONE', #4851, #15322, #32194, .T. ) ;
#27089 = FACE_OUTER_BOUND ( 'NONE', #4554, .T. ) ;
#27090 = CARTESIAN_POINT ( 'NONE',  ( 181.0000000000000000, -77.49999999999997158, -350.0000000000001705 ) ) ;
#27091 = ADVANCED_FACE ( 'NONE', ( #39640 ), #39400, .T. ) ;
#27092 = VERTEX_POINT ( 'NONE', #24244 ) ;
#27093 = EDGE_CURVE ( 'NONE', #2811, #27098, #16286, .T. ) ;
#27094 = CARTESIAN_POINT ( 'NONE',  ( 357.1715728752542418, 167.0000000000003411, 342.0000000000001137 ) ) ;
#27095 = CARTESIAN_POINT ( 'NONE',  ( 10.50000000000000178, -46.12433806312137108, -6.404467680894765813 ) ) ;
#27096 = CARTESIAN_POINT ( 'NONE',  ( 1.011271242968688311, -0.7347315653655854817, 9.972675548442463622 ) ) ;
#27097 = ORIENTED_EDGE ( 'NONE', *, *, #1369, .F. ) ;
#27098 = VERTEX_POINT ( 'NONE', #27837 ) ;
#27099 = CARTESIAN_POINT ( 'NONE',  ( -194.9999999999999432, -173.0000000000000000, 372.0000000000000568 ) ) ;
#27100 = B_SPLINE_CURVE_WITH_KNOTS ( 'NONE', 3,
 ( #26373, #47090, #42756, #4034, #46344, #10970 ),
 .UNSPECIFIED., .F., .F.,
 ( 4, 2, 4 ),
 ( 4.906538933386797396E-18, 0.009877169331704833619, 0.01975433866340966030 ),
 .UNSPECIFIED. ) ;
#27101 = DIRECTION ( 'NONE',  ( -0.000000000000000000, -1.000000000000000000, -0.000000000000000000 ) ) ;
#27102 = EDGE_CURVE ( 'NONE', #23633, #46654, #24753, .T. ) ;
#27103 = LINE ( 'NONE', #42727, #12575 ) ;
#27104 = UNCERTAINTY_MEASURE_WITH_UNIT (LENGTH_MEASURE( 1.000000000000000082E-05 ), #23127, 'distance_accuracy_value', 'NONE');
#27105 = VERTEX_POINT ( 'NONE', #28086 ) ;
#27106 = VERTEX_POINT ( 'NONE', #16037 ) ;
#27107 = ADVANCED_BREP_SHAPE_REPRESENTATION ( '', ( #22320, #45486 ), #13533 ) ;
#27108 = CARTESIAN_POINT ( 'NONE',  ( 191.5540265531851105, 0.000000000000000000, 119.0682875569279702 ) ) ;
#27109 = DIRECTION ( 'NONE',  ( 1.333906992743555050E-23, -1.000000000000000000, 0.000000000000000000 ) ) ;
#27110 = ORIENTED_EDGE ( 'NONE', *, *, #3537, .F. ) ;
#27111 = DIRECTION ( 'NONE',  ( 0.000000000000000000, 1.000000000000000000, 0.000000000000000000 ) ) ;
#27112 = CARTESIAN_POINT ( 'NONE',  ( 72.27890028733797578, -1.750000000000009548, -158.1565861772249377 ) ) ;
#27113 = CARTESIAN_POINT ( 'NONE',  ( 357.9999999999999432, -181.0000000000000568, -356.0000000000002842 ) ) ;
#27114 = CARTESIAN_POINT ( 'NONE',  ( 1.011271242968677653, 0.7347315653656002477, -3.333333333333333481 ) ) ;
#27115 = ORIENTED_EDGE ( 'NONE', *, *, #16460, .F. ) ;
#27116 = CARTESIAN_POINT ( 'NONE',  ( -3.566525152643847285, 1.569997364305458776, 9.741991644046965604 ) ) ;
#27117 = DIRECTION ( 'NONE',  ( 0.000000000000000000, -0.9749645535258955054, -0.2223603367690637767 ) ) ;
#27118 = DIRECTION ( 'NONE',  ( -1.000000000000000000, -0.000000000000000000, -0.000000000000000000 ) ) ;
#27119 = ADVANCED_FACE ( 'NONE', ( #40401 ), #35299, .T. ) ;
#27120 = CARTESIAN_POINT ( 'NONE',  ( 16.26331699892969951, 3.800463913881183764, -9.458680755252684591 ) ) ;
#27121 = VECTOR ( 'NONE', #45710, 1000.000000000000000 ) ;
#27122 = EDGE_CURVE ( 'NONE', #9291, #33463, #19867, .T. ) ;
#27123 = EDGE_CURVE ( 'NONE', #566, #10187, #29446, .T. ) ;
#27124 = ORIENTED_EDGE ( 'NONE', *, *, #7377, .F. ) ;
#27125 = CARTESIAN_POINT ( 'NONE',  ( 6.875132362119187768, -33.14667368551891258, 8.356839323120299312 ) ) ;
#27126 = ADVANCED_FACE ( 'NONE', ( #137 ), #31703, .F. ) ;
#27127 = CARTESIAN_POINT ( 'NONE',  ( 210.0000000000000568, 0.000000000000000000, -37.43171244307202272 ) ) ;
#27128 = VECTOR ( 'NONE', #49098, 1000.000000000000000 ) ;
#27129 = DIRECTION ( 'NONE',  ( -1.000000000000000000, 0.000000000000000000, 0.000000000000000000 ) ) ;
#27130 = EDGE_CURVE ( 'NONE', #28471, #39841, #39903, .T. ) ;
#27131 = ORIENTED_EDGE ( 'NONE', *, *, #50234, .F. ) ;
#27132 = LINE ( 'NONE', #16590, #28940 ) ;
#27133 = CARTESIAN_POINT ( 'NONE',  ( -49.75871208702130133, -40.58472229863598102, -5.000000000000000000 ) ) ;
#27134 = ORIENTED_EDGE ( 'NONE', *, *, #38022, .F. ) ;
#27135 = CARTESIAN_POINT ( 'NONE',  ( -14.99999999999970868, 17.00000000000000000, -84.99999999999998579 ) ) ;
#27136 = CARTESIAN_POINT ( 'NONE',  ( -125.6708471809678542, 1.749999999999996891, 121.8434138227750481 ) ) ;
#27137 = CARTESIAN_POINT ( 'NONE',  ( 0.000000000000000000, 0.000000000000000000, 910.0000000000000000 ) ) ;
#27138 = CARTESIAN_POINT ( 'NONE',  ( -88.44597344681497475, 0.000000000000000000, 42.56828755692799859 ) ) ;
#27139 = VERTEX_POINT ( 'NONE', #20125 ) ;
#27140 = CARTESIAN_POINT ( 'NONE',  ( 4.999999999999999112, -175.0000000000000284, 353.7500000000001705 ) ) ;
#27141 = VERTEX_POINT ( 'NONE', #4476 ) ;
#27142 = VERTEX_POINT ( 'NONE', #35816 ) ;
#27143 = EDGE_CURVE ( 'NONE', #46256, #5374, #4733, .T. ) ;
#27144 = ORIENTED_EDGE ( 'NONE', *, *, #12225, .T. ) ;
#27145 = CARTESIAN_POINT ( 'NONE',  ( 71.55402655318505367, 0.000000000000000000, -37.43171244307200141 ) ) ;
#27146 = CARTESIAN_POINT ( 'NONE',  ( -6.695973446814940111, -1.750000000000023315, 160.8182875569279702 ) ) ;
#27147 = ADVANCED_FACE ( 'NONE', ( #16540 ), #26879, .T. ) ;
#27148 = CARTESIAN_POINT ( 'NONE',  ( 181.0000000000000284, -174.9999999999999716, -97.00000000000014211 ) ) ;
#27149 = ORIENTED_EDGE ( 'NONE', *, *, #32914, .T. ) ;
#27150 = VECTOR ( 'NONE', #40613, 1000.000000000000000 ) ;
#27151 = CARTESIAN_POINT ( 'NONE',  ( 168.9999999999999716, -81.49999999999997158, -340.0000000000001137 ) ) ;
#27152 = CARTESIAN_POINT ( 'NONE',  ( 31.55402655318506788, 0.000000000000000000, 162.5682875569279702 ) ) ;
#27153 = CARTESIAN_POINT ( 'NONE',  ( 9.999999999999994671, -0.7319447344931275801, 9.406212099230870649 ) ) ;
#27154 = EDGE_CURVE ( 'NONE', #36736, #2086, #40652, .T. ) ;
#27155 = ORIENTED_EDGE ( 'NONE', *, *, #10879, .T. ) ;
#27156 = EDGE_CURVE ( 'NONE', #47093, #18308, #37145, .T. ) ;
#27157 = CARTESIAN_POINT ( 'NONE',  ( -0.3370904143228927730, -0.2449105217885335917, 10.00000000000000000 ) ) ;
#27158 = DIRECTION ( 'NONE',  ( -1.000000000000000000, 0.000000000000000000, -2.958228394578794270E-31 ) ) ;
#27159 = VERTEX_POINT ( 'NONE', #48802 ) ;
#27160 = ORIENTED_EDGE ( 'NONE', *, *, #47904, .F. ) ;
#27161 = VERTEX_POINT ( 'NONE', #29348 ) ;
#27162 = CARTESIAN_POINT ( 'NONE',  ( -29.12062022658179217, 29.99172060348970348, 8.846626183609803462 ) ) ;
#27163 = EDGE_CURVE ( 'NONE', #19943, #25904, #26625, .T. ) ;
#27164 = AXIS2_PLACEMENT_3D ( 'NONE', #47075, #432, #8386 ) ;
#27165 = EDGE_CURVE ( 'NONE', #41907, #22974, #21136, .T. ) ;
#27166 = CARTESIAN_POINT ( 'NONE',  ( 153.3040265531850537, -1.750000000000009992, 0.8182875569279768335 ) ) ;
#27167 = AXIS2_PLACEMENT_3D ( 'NONE', #49418, #26622, #2752 ) ;
#27168 = VERTEX_POINT ( 'NONE', #25000 ) ;
#27169 = EDGE_CURVE ( 'NONE', #42432, #45549, #25243, .T. ) ;
#27170 = CARTESIAN_POINT ( 'NONE',  ( 31.55402655318503236, 0.000000000000000000, 2.568287556927978166 ) ) ;
#27171 = CARTESIAN_POINT ( 'NONE',  ( -14.52758583651993618, -8.922352469211071835, 8.953103998512858652 ) ) ;
#27172 = CARTESIAN_POINT ( 'NONE',  ( 165.0000000000000000, -174.9999999999999716, -111.0000000000001563 ) ) ;
#27173 = DIRECTION ( 'NONE',  ( -0.000000000000000000, -1.000000000000000000, -0.000000000000000000 ) ) ;
#27174 = FACE_OUTER_BOUND ( 'NONE', #29374, .T. ) ;
#27175 = FACE_OUTER_BOUND ( 'NONE', #16686, .T. ) ;
#27176 = DIRECTION ( 'NONE',  ( 0.000000000000000000, 0.000000000000000000, 1.000000000000000000 ) ) ;
#27177 = CARTESIAN_POINT ( 'NONE',  ( 85.00000000000029843, 17.00000000000000000, -84.99999999999998579 ) ) ;
#27178 = CYLINDRICAL_SURFACE ( 'NONE', #10076, 1.749999999999973799 ) ;
#27179 = EDGE_LOOP ( 'NONE', ( #48292, #43532, #800, #8901, #14631, #41539 ) ) ;
#27180 = CARTESIAN_POINT ( 'NONE',  ( 177.5000000000000284, -102.5000000000000142, -8.575805527524005711 ) ) ;
#27181 = DIRECTION ( 'NONE',  ( 0.000000000000000000, 1.000000000000000000, 4.687818848539279227E-49 ) ) ;
#27182 = EDGE_CURVE ( 'NONE', #33773, #27818, #26009, .T. ) ;
#27183 = DIRECTION ( 'NONE',  ( 1.121065046350011585E-16, 0.7071067811865475727, 0.7071067811865474617 ) ) ;
#27184 = DIRECTION ( 'NONE',  ( 0.000000000000000000, -1.000000000000000000, 0.000000000000000000 ) ) ;
#27185 = EDGE_LOOP ( 'NONE', ( #50504, #8759, #35166, #8142 ) ) ;
#27186 = CYLINDRICAL_SURFACE ( 'NONE', #8332, 2.000000000000001776 ) ;
#27187 = DIRECTION ( 'NONE',  ( -0.000000000000000000, -0.000000000000000000, -1.000000000000000000 ) ) ;
#27188 = VECTOR ( 'NONE', #36267, 1000.000000000000000 ) ;
#27189 = AXIS2_PLACEMENT_3D ( 'NONE', #20159, #11454, #27111 ) ;
#27190 = CARTESIAN_POINT ( 'NONE',  ( -15.00099850811941948, -7.462898891544107016, 9.403735324607438884 ) ) ;
#27191 = CARTESIAN_POINT ( 'NONE',  ( 210.0000000000000568, 2.143131898507880377E-16, -0.9317124430720331585 ) ) ;
#27192 = PRODUCT_RELATED_PRODUCT_CATEGORY ( 'part', '', ( #44939 ) ) ;
#27193 = DIRECTION ( 'NONE',  ( -1.000000000000000000, -0.000000000000000000, -0.000000000000000000 ) ) ;
#27194 = VERTEX_POINT ( 'NONE', #29098 ) ;
#27195 = ORIENTED_EDGE ( 'NONE', *, *, #13263, .T. ) ;
#27196 = VECTOR ( 'NONE', #42183, 1000.000000000000000 ) ;
#27197 = DIRECTION ( 'NONE',  ( -0.000000000000000000, -0.000000000000000000, -1.000000000000000000 ) ) ;
#27198 = ORIENTED_EDGE ( 'NONE', *, *, #2203, .F. ) ;
#27199 = FACE_OUTER_BOUND ( 'NONE', #18986, .T. ) ;
#27201 = ADVANCED_FACE ( 'NONE', ( #20886 ), #36573, .T. ) ;
#27200 = CARTESIAN_POINT ( 'NONE',  ( -125.6708471809678542, 1.749999999999996891, -78.15658617722492352 ) ) ;
#27202 = ORIENTED_EDGE ( 'NONE', *, *, #5278, .T. ) ;
#27203 =( NAMED_UNIT ( * ) PLANE_ANGLE_UNIT ( ) SI_UNIT ( $, .RADIAN. ) );
#27204 = ORIENTED_EDGE ( 'NONE', *, *, #23378, .T. ) ;
#27205 = ORIENTED_EDGE ( 'NONE', *, *, #17136, .T. ) ;
#27206 = DIRECTION ( 'NONE',  ( -1.000000000000000000, 0.000000000000000000, 0.000000000000000000 ) ) ;
#27207 = CARTESIAN_POINT ( 'NONE',  ( -164.4973046169135955, 103.0380105690400683, 23.74256005001722158 ) ) ;
#27208 = ORIENTED_EDGE ( 'NONE', *, *, #33534, .F. ) ;
#27209 = LINE ( 'NONE', #23092, #13921 ) ;
#27210 = DIRECTION ( 'NONE',  ( -1.000000000000000000, 0.000000000000000000, 1.860490536778032451E-50 ) ) ;
#27211 = LINE ( 'NONE', #20515, #2766 ) ;
#27212 = EDGE_LOOP ( 'NONE', ( #27846, #32581, #15855, #21923 ) ) ;
#27213 = DIRECTION ( 'NONE',  ( -1.000000000000000000, 0.000000000000000000, -0.000000000000000000 ) ) ;
#27214 = LINE ( 'NONE', #43607, #17403 ) ;
#27215 =( BOUNDED_CURVE ( )  B_SPLINE_CURVE ( 3, ( #32751, #12737, #36631, #4777 ),
 .UNSPECIFIED., .F., .F. ) 
 B_SPLINE_CURVE_WITH_KNOTS ( ( 4, 4 ),
 ( 1.570796326794896558, 3.141592653589793116 ),
 .UNSPECIFIED. ) 
 CURVE ( )  GEOMETRIC_REPRESENTATION_ITEM ( )  RATIONAL_B_SPLINE_CURVE ( ( 1.000000000000000000, 0.8047378541243649375, 0.8047378541243649375, 1.000000000000000000 ) ) 
 REPRESENTATION_ITEM ( '' )  );
#27216 = EDGE_CURVE ( 'NONE', #42459, #25772, #2055, .T. ) ;
#27217 = ORIENTED_EDGE ( 'NONE', *, *, #8134, .F. ) ;
#27218 = EDGE_CURVE ( 'NONE', #28673, #4784, #38647, .T. ) ;
#27219 = CARTESIAN_POINT ( 'NONE',  ( 45.64490844644690526, 21.32281559348795597, 8.807470649214879543 ) ) ;
#27220 = CARTESIAN_POINT ( 'NONE',  ( 2.500000000000002665, 204.9999999999999716, -234.7500000000000000 ) ) ;
#27221 = ORIENTED_EDGE ( 'NONE', *, *, #49745, .F. ) ;
#27222 = DIRECTION ( 'NONE',  ( 0.000000000000000000, 0.000000000000000000, 1.000000000000000000 ) ) ;
#27223 =( BOUNDED_CURVE ( )  B_SPLINE_CURVE ( 3, ( #10633, #34252, #26043, #40934 ),
 .UNSPECIFIED., .F., .F. ) 
 B_SPLINE_CURVE_WITH_KNOTS ( ( 4, 4 ),
 ( 1.570796326794896558, 3.141592653589793116 ),
 .UNSPECIFIED. ) 
 CURVE ( )  GEOMETRIC_REPRESENTATION_ITEM ( )  RATIONAL_B_SPLINE_CURVE ( ( 1.000000000000000000, 0.8047378541243649375, 0.8047378541243649375, 1.000000000000000000 ) ) 
 REPRESENTATION_ITEM ( '' )  );
#27224 = VECTOR ( 'NONE', #18691, 1000.000000000000000 ) ;
#27225 = EDGE_CURVE ( 'NONE', #31434, #23873, #35035, .T. ) ;
#27226 = CARTESIAN_POINT ( 'NONE',  ( 355.9999999999999432, -181.0000000000001421, -349.9999999999999432 ) ) ;
#27227 = ORIENTED_EDGE ( 'NONE', *, *, #47148, .F. ) ;
#27228 = AXIS2_PLACEMENT_3D ( 'NONE', #27254, #7761, #15696 ) ;
#27229 = DIRECTION ( 'NONE',  ( -1.000000000000000000, 4.996003610813203446E-16, -1.033975765691284410E-24 ) ) ;
#27230 = ADVANCED_FACE ( 'NONE', ( #48291 ), #1898, .T. ) ;
#27231 = CARTESIAN_POINT ( 'NONE',  ( 135.0000000000012790, 16.00000000000000000, 5.000000000000004441 ) ) ;
#27232 = CARTESIAN_POINT ( 'NONE',  ( 397.9839762253770346, 0.000000000000000000, 197.0020682315616796 ) ) ;
#27233 = EDGE_CURVE ( 'NONE', #46411, #6309, #7835, .T. ) ;
#27234 = DIRECTION ( 'NONE',  ( 0.000000000000000000, 0.000000000000000000, -1.000000000000000000 ) ) ;
#27235 = VECTOR ( 'NONE', #19377, 1000.000000000000000 ) ;
#27236 = ORIENTED_EDGE ( 'NONE', *, *, #25801, .T. ) ;
#27237 = DIRECTION ( 'NONE',  ( 0.000000000000000000, 0.000000000000000000, -1.000000000000000000 ) ) ;
#27238 = ADVANCED_FACE ( 'NONE', ( #46722 ), #41649, .T. ) ;
#27239 =( BOUNDED_CURVE ( )  B_SPLINE_CURVE ( 3, ( #25585, #49639, #3222, #41225 ),
 .UNSPECIFIED., .F., .F. ) 
 B_SPLINE_CURVE_WITH_KNOTS ( ( 4, 4 ),
 ( 1.570796326794896558, 3.141592653589793116 ),
 .UNSPECIFIED. ) 
 CURVE ( )  GEOMETRIC_REPRESENTATION_ITEM ( )  RATIONAL_B_SPLINE_CURVE ( ( 1.000000000000000000, 0.8047378541243649375, 0.8047378541243649375, 1.000000000000000000 ) ) 
 REPRESENTATION_ITEM ( '' )  );
#27240 = DIRECTION ( 'NONE',  ( 1.000000000000000000, 1.156482317317870492E-16, -0.000000000000000000 ) ) ;
#27241 = ORIENTED_EDGE ( 'NONE', *, *, #12442, .F. ) ;
#27242 = EDGE_LOOP ( 'NONE', ( #8487, #48988, #47337, #49767 ) ) ;
#27243 = DIRECTION ( 'NONE',  ( 0.04278265094206106650, 0.7851806034415852453, 0.6177872325950720667 ) ) ;
#27244 = LINE ( 'NONE', #38797, #47398 ) ;
#27245 = DIRECTION ( 'NONE',  ( -1.000000000000000000, 1.586032892321652236E-16, 9.711650524620651178E-33 ) ) ;
#27246 = CARTESIAN_POINT ( 'NONE',  ( -204.9459734468149463, 2.143131898507880377E-16, -157.4317124430720582 ) ) ;
#27247 = DIRECTION ( 'NONE',  ( -0.000000000000000000, -0.000000000000000000, -1.000000000000000000 ) ) ;
#27248 = EDGE_LOOP ( 'NONE', ( #7022, #3920, #23885, #34807 ) ) ;
#27249 = CARTESIAN_POINT ( 'NONE',  ( 194.3291528190321742, -1.750000000000010436, 119.7931612910808781 ) ) ;
#27250 = VECTOR ( 'NONE', #37341, 1000.000000000000000 ) ;
#27251 = LINE ( 'NONE', #19529, #36810 ) ;
#27252 = DIRECTION ( 'NONE',  ( 0.000000000000000000, 0.000000000000000000, 1.000000000000000000 ) ) ;
#27253 = EDGE_LOOP ( 'NONE', ( #9044, #34756, #38383, #8687, #36361 ) ) ;
#27254 = CARTESIAN_POINT ( 'NONE',  ( -5.647304616913629616, -291.2764864723799860, 145.3277671506088780 ) ) ;
#27255 = EDGE_LOOP ( 'NONE', ( #14515, #21451, #21530, #27529, #34952, #3133, #24477, #28548, #25706, #22775, #28597, #28957, #24620, #45171 ) ) ;
#27256 = CARTESIAN_POINT ( 'NONE',  ( 114.3291528190321173, 1.749999999999996669, -160.2068387089191219 ) ) ;
#27257 = PRESENTATION_LAYER_ASSIGNMENT (  '', '', ( #29698 ) ) ;
#27258 = CARTESIAN_POINT ( 'NONE',  ( -0.5359691244547112321, 1.100286284792928893, 9.966990753365127631 ) ) ;
#27259 = VERTEX_POINT ( 'NONE', #30360 ) ;
#27260 = DIRECTION ( 'NONE',  ( 0.000000000000000000, 0.000000000000000000, 1.000000000000000000 ) ) ;
#27261 = VECTOR ( 'NONE', #615, 1000.000000000000000 ) ;
#27262 = CARTESIAN_POINT ( 'NONE',  ( 31.44259251615245887, 38.95901822126168668, -9.367992836599954742 ) ) ;
#27263 = DIRECTION ( 'NONE',  ( 0.000000000000000000, 0.000000000000000000, -1.000000000000000000 ) ) ;
#27264 = ORIENTED_EDGE ( 'NONE', *, *, #24742, .T. ) ;
#27266 = ADVANCED_FACE ( 'NONE', ( #3393 ), #38582, .T. ) ;
#27265 = VECTOR ( 'NONE', #11546, 1000.000000000000000 ) ;
#27267 = DIRECTION ( 'NONE',  ( 0.000000000000000000, 1.000000000000000000, -1.822804496942679766E-16 ) ) ;
#27268 = CIRCLE ( 'NONE', #23149, 2.000000000000001776 ) ;
#27269 = LINE ( 'NONE', #2634, #12312 ) ;
#27270 = ORIENTED_EDGE ( 'NONE', *, *, #41494, .T. ) ;
#27271 = FACE_OUTER_BOUND ( 'NONE', #9727, .T. ) ;
#27272 = CARTESIAN_POINT ( 'NONE',  ( 2.595273106918288164, 2.906811120256387326, 9.741991644047248045 ) ) ;
#27273 = CARTESIAN_POINT ( 'NONE',  ( 210.0000000000000568, 2.143131898507881856E-16, -120.9317124430720582 ) ) ;
#27274 = CARTESIAN_POINT ( 'NONE',  ( 0.3862712429686894766, -1.188820645368940276, 10.00000000000000000 ) ) ;
#27275 = ORIENTED_EDGE ( 'NONE', *, *, #31229, .F. ) ;
#27276 = ORIENTED_EDGE ( 'NONE', *, *, #36565, .T. ) ;
#27277 = FACE_OUTER_BOUND ( 'NONE', #41458, .T. ) ;
#27278 = CARTESIAN_POINT ( 'NONE',  ( -206.6959734468149463, -1.750000000000010214, 40.81828755692798438 ) ) ;
#27279 = ORIENTED_EDGE ( 'NONE', *, *, #2428, .F. ) ;
#27280 = LINE ( 'NONE', #86, #44565 ) ;
#27281 = FACE_OUTER_BOUND ( 'NONE', #9339, .T. ) ;
#27282 = FACE_BOUND ( 'NONE', #8061, .T. ) ;
#27283 = VERTEX_POINT ( 'NONE', #19047 ) ;
#27284 = CARTESIAN_POINT ( 'NONE',  ( 153.3040265531850537, -1.750000000000010658, 80.81828755692798438 ) ) ;
#27285 = ORIENTED_EDGE ( 'NONE', *, *, #25956, .T. ) ;
#27286 = CARTESIAN_POINT ( 'NONE',  ( -5.000000000000000000, -184.7999999999999545, -340.2000000000001592 ) ) ;
#27287 = DIRECTION ( 'NONE',  ( -1.000000000000000000, 0.000000000000000000, 1.860490536778032451E-50 ) ) ;
#27288 = EDGE_CURVE ( 'NONE', #7259, #26234, #2877, .T. ) ;
#27289 = EDGE_CURVE ( 'NONE', #33462, #31257, #42391, .T. ) ;
#27290 = CARTESIAN_POINT ( 'NONE',  ( 181.0000000000000000, -272.5000000000000000, -112.9999999999999005 ) ) ;
#27291 = VERTEX_POINT ( 'NONE', #38067 ) ;
#27292 = ORIENTED_EDGE ( 'NONE', *, *, #15196, .F. ) ;
#27293 = ORIENTED_EDGE ( 'NONE', *, *, #44019, .F. ) ;
#27294 = DIRECTION ( 'NONE',  ( 4.440892098500625176E-16, 0.7071067811865474617, 0.7071067811865475727 ) ) ;
#27295 = ADVANCED_FACE ( 'NONE', ( #10596 ), #7520, .T. ) ;
#27296 = CARTESIAN_POINT ( 'NONE',  ( 168.9999999999999716, -164.9999999999999432, 343.9999999999998863 ) ) ;
#27297 = AXIS2_PLACEMENT_3D ( 'NONE', #24096, #7941, #47381 ) ;
#27298 = CARTESIAN_POINT ( 'NONE',  ( 356.0000000000000000, -174.9999999999999432, 341.9999999999998295 ) ) ;
#27299 = EDGE_LOOP ( 'NONE', ( #18937, #20625, #33862, #28980, #32255, #41929 ) ) ;
#27300 = FACE_OUTER_BOUND ( 'NONE', #50455, .T. ) ;
#27301 = ORIENTED_EDGE ( 'NONE', *, *, #34048, .T. ) ;
#27302 = AXIS2_PLACEMENT_3D ( 'NONE', #25548, #13739, #9644 ) ;
#27303 = EDGE_LOOP ( 'NONE', ( #32356, #48547, #39481, #42040 ) ) ;
#27304 = CARTESIAN_POINT ( 'NONE',  ( 356.0000000000000000, 185.0000000000000284, -360.0000000000002274 ) ) ;
#27305 = CARTESIAN_POINT ( 'NONE',  ( -85.67084718096784002, -1.750000000000010436, 119.7931612910808781 ) ) ;
#27306 = CARTESIAN_POINT ( 'NONE',  ( -6.000000000000000888, 0.000000000000000000, 15.00000000000000000 ) ) ;
#27307 = VECTOR ( 'NONE', #742, 1000.000000000000000 ) ;
#27308 = CARTESIAN_POINT ( 'NONE',  ( 1.158497635116737312, -16.61944452314319420, -3.546734833711462365 ) ) ;
#27309 = ORIENTED_EDGE ( 'NONE', *, *, #10302, .F. ) ;
#27310 = ORIENTED_EDGE ( 'NONE', *, *, #40658, .T. ) ;
#27311 = CARTESIAN_POINT ( 'NONE',  ( -33.47329838550543712, 31.99020508012724662, 7.455576670931136185 ) ) ;
#27312 = B_SPLINE_SURFACE_WITH_KNOTS ( 'NONE', 3, 3, ( 
 ( #46024, #26823, #11676, #11939 ),
 ( #2952, #42963, #18597, #19108 ),
 ( #46779, #22958, #34274, #3197 ),
 ( #18845, #14762, #3973, #38639 ) ),
 .UNSPECIFIED., .F., .F., .F.,
 ( 4, 4 ),
 ( 4, 4 ),
 ( 0.000000000000000000, 1.000000000000000000 ),
 ( 0.000000000000000000, 1.000000000000000000 ),
 .UNSPECIFIED. ) ;
#27313 = CARTESIAN_POINT ( 'NONE',  ( -167.7210997126620384, -1.750000000000009548, 161.8434138227750907 ) ) ;
#27314 = CARTESIAN_POINT ( 'NONE',  ( -16.15814872688569181, -4.048305257546697788, -2.870787844569587133 ) ) ;
#27315 = CARTESIAN_POINT ( 'NONE',  ( -50.11058929355266400, 7.578863168071933387, 7.455576670931136185 ) ) ;
#27316 =( BOUNDED_CURVE ( )  B_SPLINE_CURVE ( 3, ( #18272, #38571, #14948, #30603 ),
 .UNSPECIFIED., .F., .F. ) 
 B_SPLINE_CURVE_WITH_KNOTS ( ( 4, 4 ),
 ( 4.712388980384669246, 6.283185307179586232 ),
 .UNSPECIFIED. ) 
 CURVE ( )  GEOMETRIC_REPRESENTATION_ITEM ( )  RATIONAL_B_SPLINE_CURVE ( ( 1.000000000000000000, 0.8047378541243601635, 0.8047378541243601635, 1.000000000000000000 ) ) 
 REPRESENTATION_ITEM ( '' )  );
#27317 = CARTESIAN_POINT ( 'NONE',  ( 36.76598589393955052, 7.383243274241862331, -8.192531242611266862 ) ) ;
#27318 = ORIENTED_EDGE ( 'NONE', *, *, #32983, .T. ) ;
#27319 = DIRECTION ( 'NONE',  ( 1.000000000000000000, -1.586032892321652236E-16, -9.711650524620651178E-33 ) ) ;
#27320 = CARTESIAN_POINT ( 'NONE',  ( 44.99506233596246574, 23.32283626942318477, 7.455576670931136185 ) ) ;
#27321 = EDGE_CURVE ( 'NONE', #38840, #17911, #34469, .T. ) ;
#27322 = EDGE_LOOP ( 'NONE', ( #30021, #14329, #16986, #21314 ) ) ;
#27323 = CARTESIAN_POINT ( 'NONE',  ( 115.0540265531850395, 2.143131898507847836E-16, -160.9317124430720014 ) ) ;
#27324 = VECTOR ( 'NONE', #17895, 1000.000000000000000 ) ;
#27325 = CARTESIAN_POINT ( 'NONE',  ( 1.011271242968688311, -0.7347315653655855927, -10.00000000000000000 ) ) ;
#27326 = CARTESIAN_POINT ( 'NONE',  ( 181.0000000000000000, -7.999999999999952038, -350.0000000000001705 ) ) ;
#27327 = VECTOR ( 'NONE', #12848, 1000.000000000000000 ) ;
#27328 = ORIENTED_EDGE ( 'NONE', *, *, #32908, .F. ) ;
#27329 = ORIENTED_EDGE ( 'NONE', *, *, #10927, .T. ) ;
#27330 = CARTESIAN_POINT ( 'NONE',  ( 6.196515397221660670, 4.974751005920831304, 9.432811472610147518 ) ) ;
#27331 = CARTESIAN_POINT ( 'NONE',  ( -2.595273106918313033, -2.906811120256372671, 9.741991644047246268 ) ) ;
#27332 = EDGE_LOOP ( 'NONE', ( #21765, #25975, #22487, #18606 ) ) ;
#27333 = AXIS2_PLACEMENT_3D ( 'NONE', #48587, #13480, #18083 ) ;
#27334 = EDGE_LOOP ( 'NONE', ( #47929, #19477, #14739, #26075 ) ) ;
#27335 = DIRECTION ( 'NONE',  ( 1.333906992743555050E-23, -1.000000000000000000, 0.000000000000000000 ) ) ;
#27336 = CARTESIAN_POINT ( 'NONE',  ( 11.73320209285708415, -11.96063479729170886, 9.403735324607438884 ) ) ;
#27337 = DIRECTION ( 'NONE',  ( 1.000000000000000000, -0.000000000000000000, -0.000000000000000000 ) ) ;
#27338 = CARTESIAN_POINT ( 'NONE',  ( -164.9459734468149463, 2.143131898507880377E-16, 82.56828755692798438 ) ) ;
#27339 = EDGE_LOOP ( 'NONE', ( #15467, #823, #8491 ) ) ;
#27340 = ORIENTED_EDGE ( 'NONE', *, *, #25802, .T. ) ;
#27341 = EDGE_LOOP ( 'NONE', ( #6616, #616, #8015, #47240, #40270 ) ) ;
#27342 = CARTESIAN_POINT ( 'NONE',  ( 195.0540265531851105, 2.143131898507890731E-16, 165.0000000000000000 ) ) ;
#27343 = LINE ( 'NONE', #19120, #31665 ) ;
#27344 = VERTEX_POINT ( 'NONE', #22396 ) ;
#27345 = VECTOR ( 'NONE', #11964, 1000.000000000000000 ) ;
#27346 = DIRECTION ( 'NONE',  ( -7.793956916774525800E-48, 0.000000000000000000, 1.000000000000000000 ) ) ;
#27347 = CYLINDRICAL_SURFACE ( 'NONE', #5281, 2.000000000000001776 ) ;
#27348 = CARTESIAN_POINT ( 'NONE',  ( 71.55402655318505367, 1.025126265847089657, -120.9317124430720440 ) ) ;
#27349 = ORIENTED_EDGE ( 'NONE', *, *, #16309, .T. ) ;
#27350 = ORIENTED_EDGE ( 'NONE', *, *, #27884, .F. ) ;
#27351 = DIRECTION ( 'NONE',  ( -1.586032892321652236E-16, -1.000000000000000000, -6.853681917100419162E-49 ) ) ;
#27352 = ADVANCED_FACE ( 'NONE', ( #26262 ), #6495, .T. ) ;
#27353 = CARTESIAN_POINT ( 'NONE',  ( -127.7210997126620242, -1.749999999999996669, 161.8434138227750907 ) ) ;
#27354 = CARTESIAN_POINT ( 'NONE',  ( 192.2789002873380184, 1.750000000000009548, -118.1565861772249519 ) ) ;
#27355 = ORIENTED_EDGE ( 'NONE', *, *, #24275, .T. ) ;
#27356 = EDGE_LOOP ( 'NONE', ( #3465, #11301, #28430, #12126 ) ) ;
#27357 = CARTESIAN_POINT ( 'NONE',  ( 0.000000000000000000, 0.000000000000000000, 800.0000000000000000 ) ) ;
#27358 = ORIENTED_EDGE ( 'NONE', *, *, #38085, .T. ) ;
#27359 = LINE ( 'NONE', #42996, #30344 ) ;
#27360 = LINE ( 'NONE', #15319, #19459 ) ;
#27361 = CARTESIAN_POINT ( 'NONE',  ( 130.0000000000015064, 16.00000000000000000, 60.00000000000000000 ) ) ;
#27362 = CARTESIAN_POINT ( 'NONE',  ( 10.70590866674922204, -12.76446523155706814, -3.546734833711462365 ) ) ;
#27363 = ORIENTED_EDGE ( 'NONE', *, *, #30339, .F. ) ;
#27364 = AXIS2_PLACEMENT_3D ( 'NONE', #7369, #38676, #33732 ) ;
#27365 = EDGE_CURVE ( 'NONE', #44977, #35508, #27009, .T. ) ;
#27366 = CARTESIAN_POINT ( 'NONE',  ( 2.052581215100350853, -0.2042358160480859663, 9.886433018048069954 ) ) ;
#27367 = CARTESIAN_POINT ( 'NONE',  ( 341.6568542494922553, -185.0000000000000853, -360.0000000000003411 ) ) ;
#27368 = LINE ( 'NONE', #35348, #41655 ) ;
#27369 = AXIS2_PLACEMENT_3D ( 'NONE', #24056, #11995, #39709 ) ;
#27370 = EDGE_CURVE ( 'NONE', #29584, #40814, #10847, .T. ) ;
#27371 = VECTOR ( 'NONE', #44871, 1000.000000000000000 ) ;
#27372 = CARTESIAN_POINT ( 'NONE',  ( 48.33712804702526000, 13.03701565032775811, -9.367992836599951190 ) ) ;
#27373 =( BOUNDED_CURVE ( )  B_SPLINE_CURVE ( 3, ( #473, #16116, #31778, #24075 ),
 .UNSPECIFIED., .F., .F. ) 
 B_SPLINE_CURVE_WITH_KNOTS ( ( 4, 4 ),
 ( 6.280369834735098695E-16, 1.570796326794897002 ),
 .UNSPECIFIED. ) 
 CURVE ( )  GEOMETRIC_REPRESENTATION_ITEM ( )  RATIONAL_B_SPLINE_CURVE ( ( 1.000000000000000000, 0.8047378541243650485, 0.8047378541243650485, 1.000000000000000000 ) ) 
 REPRESENTATION_ITEM ( '' )  );
#27374 = ORIENTED_EDGE ( 'NONE', *, *, #18686, .T. ) ;
#27375 = CARTESIAN_POINT ( 'NONE',  ( 4.763548243873389154, -16.57409059453848599, 8.727788335465566760 ) ) ;
#27376 =( BOUNDED_CURVE ( )  B_SPLINE_CURVE ( 3, ( #6188, #21846, #37512, #25950 ),
 .UNSPECIFIED., .F., .F. ) 
 B_SPLINE_CURVE_WITH_KNOTS ( ( 4, 4 ),
 ( 3.141592653589793116, 4.712388980384689674 ),
 .UNSPECIFIED. ) 
 CURVE ( )  GEOMETRIC_REPRESENTATION_ITEM ( )  RATIONAL_B_SPLINE_CURVE ( ( 1.000000000000000000, 0.8047378541243649375, 0.8047378541243649375, 1.000000000000000000 ) ) 
 REPRESENTATION_ITEM ( '' )  );
#27377 = CARTESIAN_POINT ( 'NONE',  ( 0.3862712429686810944, 1.188820645368943607, 10.00000000000000000 ) ) ;
#27378 = EDGE_CURVE ( 'NONE', #25557, #39055, #10582, .T. ) ;
#27379 = EDGE_CURVE ( 'NONE', #30568, #16843, #38832, .T. ) ;
#27380 = CARTESIAN_POINT ( 'NONE',  ( 181.0000000000000284, -174.9999999999999716, -97.00000000000014211 ) ) ;
#27382 = ORIENTED_EDGE ( 'NONE', *, *, #36859, .F. ) ;
#27381 = EDGE_CURVE ( 'NONE', #27344, #42411, #30217, .T. ) ;
#27383 = LINE ( 'NONE', #12474, #20734 ) ;
#27384 = VECTOR ( 'NONE', #24028, 1000.000000000000000 ) ;
#27385 = DIRECTION ( 'NONE',  ( -0.000000000000000000, -1.000000000000000000, -0.000000000000000000 ) ) ;
#27386 = VERTEX_POINT ( 'NONE', #6747 ) ;
#27387 = DIRECTION ( 'NONE',  ( -0.000000000000000000, -0.000000000000000000, -1.000000000000000000 ) ) ;
#27388 = LINE ( 'NONE', #26875, #273 ) ;
#27389 = LINE ( 'NONE', #28640, #26647 ) ;
#27390 = ORIENTED_EDGE ( 'NONE', *, *, #18991, .F. ) ;
#27391 = CARTESIAN_POINT ( 'NONE',  ( 115.0540265531850395, 2.143131898507847836E-16, -80.93171244307201562 ) ) ;
#27392 = ORIENTED_EDGE ( 'NONE', *, *, #23988, .F. ) ;
#27393 = ORIENTED_EDGE ( 'NONE', *, *, #33478, .F. ) ;
#27394 = CARTESIAN_POINT ( 'NONE',  ( 164.9999999999999716, -5.999999999999950262, -350.0000000000001705 ) ) ;
#27395 = DIRECTION ( 'NONE',  ( -1.000000000000000000, -0.000000000000000000, -0.000000000000000000 ) ) ;
#27396 = VERTEX_POINT ( 'NONE', #18539 ) ;
#27397 = CARTESIAN_POINT ( 'NONE',  ( 181.0000000000000568, 175.0000000000000284, 339.9999999999998863 ) ) ;
#27398 = DIRECTION ( 'NONE',  ( -0.000000000000000000, -0.000000000000000000, -1.000000000000000000 ) ) ;
#27399 = AXIS2_PLACEMENT_3D ( 'NONE', #34339, #19171, #24321 ) ;
#27400 = AXIS2_PLACEMENT_3D ( 'NONE', #15449, #6737, #22384 ) ;
#27401 = CARTESIAN_POINT ( 'NONE',  ( 360.0000000000001137, 178.0000000000000284, 352.9999999999998295 ) ) ;
#27402 = EDGE_CURVE ( 'NONE', #20193, #47543, #30613, .T. ) ;
#27403 = ORIENTED_EDGE ( 'NONE', *, *, #24063, .F. ) ;
#27404 = VECTOR ( 'NONE', #2542, 1000.000000000000000 ) ;
#27405 = CYLINDRICAL_SURFACE ( 'NONE', #9409, 4.000000000000003553 ) ;
#27406 = EDGE_CURVE ( 'NONE', #41782, #48234, #15838, .T. ) ;
#27407 = ORIENTED_EDGE ( 'NONE', *, *, #37119, .T. ) ;
#27408 = ADVANCED_FACE ( 'NONE', ( #34218 ), #15217, .F. ) ;
#27409 = DIRECTION ( 'NONE',  ( 0.000000000000000000, 0.000000000000000000, 1.000000000000000000 ) ) ;
#27410 = DIRECTION ( 'NONE',  ( 0.000000000000000000, -1.000000000000000000, 2.537652627714643577E-15 ) ) ;
#27411 = VERTEX_POINT ( 'NONE', #23427 ) ;
#27412 = ORIENTED_EDGE ( 'NONE', *, *, #15569, .F. ) ;
#27413 = ORIENTED_EDGE ( 'NONE', *, *, #3635, .F. ) ;
#27414 = LINE ( 'NONE', #7663, #42635 ) ;
#27415 = ADVANCED_FACE ( 'NONE', ( #16230 ), #35236, .T. ) ;
#27416 = DIRECTION ( 'NONE',  ( 0.000000000000000000, 0.000000000000000000, -1.000000000000000000 ) ) ;
#27417 = ORIENTED_EDGE ( 'NONE', *, *, #26130, .F. ) ;
#27418 = EDGE_CURVE ( 'NONE', #2035, #29662, #35491, .T. ) ;
#27419 = CARTESIAN_POINT ( 'NONE',  ( 35.00000000000122213, 17.00000000000000000, 5.000000000000004441 ) ) ;
#27420 = CARTESIAN_POINT ( 'NONE',  ( -70.00000000000002842, 17.00000000000000000, -114.9999999999999858 ) ) ;
#27421 = DIRECTION ( 'NONE',  ( 1.000000000000000000, 0.000000000000000000, -0.000000000000000000 ) ) ;
#27422 = DIRECTION ( 'NONE',  ( 0.000000000000000000, 0.000000000000000000, 1.000000000000000000 ) ) ;
#27423 = CARTESIAN_POINT ( 'NONE',  ( 151.5540265531850537, 0.000000000000000000, -37.43171244307205825 ) ) ;
#27424 = CARTESIAN_POINT ( 'NONE',  ( 32.27890028733795447, -1.750000000000009548, -38.15658617722494483 ) ) ;
#27425 = CARTESIAN_POINT ( 'NONE',  ( -205.6708471809678827, 1.750000000000010214, -80.20683870891910772 ) ) ;
#27426 = VECTOR ( 'NONE', #18579, 1000.000000000000000 ) ;
#27427 = LINE ( 'NONE', #39999, #7067 ) ;
#27428 = CARTESIAN_POINT ( 'NONE',  ( 164.9999999999999716, 17.00000000000000000, -90.00000000000002842 ) ) ;
#27429 = CARTESIAN_POINT ( 'NONE',  ( -4.945973446814903696, 2.143131898507912917E-16, -37.43171244307200141 ) ) ;
#27430 = ORIENTED_EDGE ( 'NONE', *, *, #27623, .F. ) ;
#27431 = LINE ( 'NONE', #27685, #30802 ) ;
#27432 = AXIS2_PLACEMENT_3D ( 'NONE', #27151, #42777, #38705 ) ;
#27433 = DIRECTION ( 'NONE',  ( -1.000000000000000000, 0.000000000000000000, -0.000000000000000000 ) ) ;
#27434 = FACE_OUTER_BOUND ( 'NONE', #12897, .T. ) ;
#27435 = ORIENTED_EDGE ( 'NONE', *, *, #26508, .T. ) ;
#27436 = DIRECTION ( 'NONE',  ( -1.586032892321652482E-16, 0.000000000000000000, -1.000000000000000000 ) ) ;
#27437 = DIRECTION ( 'NONE',  ( -0.000000000000000000, -0.000000000000000000, -1.000000000000000000 ) ) ;
#27438 = CARTESIAN_POINT ( 'NONE',  ( -88.44597344681497475, 0.000000000000000000, -77.43171244307198720 ) ) ;
#27439 = EDGE_CURVE ( 'NONE', #38609, #31704, #14489, .T. ) ;
#27440 = ADVANCED_FACE ( 'NONE', ( #39588 ), #27533, .F. ) ;
#27441 = AXIS2_PLACEMENT_3D ( 'NONE', #4005, #43251, #23768 ) ;
#27442 = CARTESIAN_POINT ( 'NONE',  ( -17.23491422248386584, 0.5912720620001978844, 8.727788335465566760 ) ) ;
#27444 = ORIENTED_EDGE ( 'NONE', *, *, #43825, .F. ) ;
#27443 = ADVANCED_FACE ( 'NONE', ( #39337 ), #35998, .F. ) ;
#27445 = DIRECTION ( 'NONE',  ( 0.000000000000000000, 0.000000000000000000, 1.000000000000000000 ) ) ;
#27446 = ADVANCED_FACE ( 'NONE', ( #8283 ), #4175, .T. ) ;
#27447 = ORIENTED_EDGE ( 'NONE', *, *, #13284, .T. ) ;
#27448 = CARTESIAN_POINT ( 'NONE',  ( 44.25629667545849344, 0.000000000000000000, 790.0000000000000000 ) ) ;
#27449 = ORIENTED_EDGE ( 'NONE', *, *, #13638, .T. ) ;
#27450 = EDGE_CURVE ( 'NONE', #12217, #28949, #19812, .T. ) ;
#27451 = CYLINDRICAL_SURFACE ( 'NONE', #19718, 1.750000000000015543 ) ;
#27452 = DIRECTION ( 'NONE',  ( -0.000000000000000000, -0.000000000000000000, -1.000000000000000000 ) ) ;
#27453 = EDGE_CURVE ( 'NONE', #35686, #15022, #20071, .T. ) ;
#27454 = B_SPLINE_CURVE_WITH_KNOTS ( 'NONE', 3,
 ( #41438, #48585, #9382, #21177, #17081, #1689 ),
 .UNSPECIFIED., .F., .F.,
 ( 4, 2, 4 ),
 ( 4.683753385137379155E-17, 0.009882509389272372408, 0.01976501877854469624 ),
 .UNSPECIFIED. ) ;
#27455 = ORIENTED_EDGE ( 'NONE', *, *, #22940, .T. ) ;
#27456 = CARTESIAN_POINT ( 'NONE',  ( -331.7552636306689919, -248.6897383013407250, 297.1446280767822259 ) ) ;
#27457 = ORIENTED_EDGE ( 'NONE', *, *, #41675, .F. ) ;
#27458 = VECTOR ( 'NONE', #13991, 1000.000000000000000 ) ;
#27459 = VERTEX_POINT ( 'NONE', #12616 ) ;
#27460 = CARTESIAN_POINT ( 'NONE',  ( 73.30402655318508209, -1.750000000000009992, 160.8182875569279702 ) ) ;
#27461 = CARTESIAN_POINT ( 'NONE',  ( -204.9459734468149463, 2.143131898507880377E-16, 122.5682875569279702 ) ) ;
#27462 = CIRCLE ( 'NONE', #2040, 4.000000000000003553 ) ;
#27463 = ORIENTED_EDGE ( 'NONE', *, *, #21594, .F. ) ;
#27464 = DIRECTION ( 'NONE',  ( -0.000000000000000000, -0.000000000000000000, -1.000000000000000000 ) ) ;
#27465 = CARTESIAN_POINT ( 'NONE',  ( -1.193089574352124149, -0.2545860991493743564, 9.963925895596188909 ) ) ;
#27466 = DIRECTION ( 'NONE',  ( 0.000000000000000000, -1.000000000000000000, 0.000000000000000000 ) ) ;
#27467 = EDGE_LOOP ( 'NONE', ( #39829, #5095, #14845, #32212 ) ) ;
#27468 = CARTESIAN_POINT ( 'NONE',  ( -33.57695195286787282, -16.69845195084869616, 8.914903342594564961 ) ) ;
#27469 = EDGE_CURVE ( 'NONE', #6749, #41585, #16485, .T. ) ;
#27470 = CARTESIAN_POINT ( 'NONE',  ( -86.69597344681494633, -1.750000000000010658, -119.1817124430720440 ) ) ;
#27471 = ADVANCED_FACE ( 'NONE', ( #31386, #28025 ), #42901, .F. ) ;
#27472 = ORIENTED_EDGE ( 'NONE', *, *, #46934, .F. ) ;
#27473 = ADVANCED_FACE ( 'NONE', ( #27775 ), #4425, .F. ) ;
#27474 = PLANE ( 'NONE',  #8717 ) ;
#27475 = VECTOR ( 'NONE', #25485, 1000.000000000000000 ) ;
#27476 = DIRECTION ( 'NONE',  ( 0.000000000000000000, 0.000000000000000000, 1.000000000000000000 ) ) ;
#27477 = EDGE_LOOP ( 'NONE', ( #37351, #42333, #48175, #26006, #37765, #15565 ) ) ;
#27478 = AXIS2_PLACEMENT_3D ( 'NONE', #38040, #2851, #35724 ) ;
#27479 = DIRECTION ( 'NONE',  ( 0.000000000000000000, -2.265761274745217480E-16, 1.000000000000000000 ) ) ;
#27480 = VERTEX_POINT ( 'NONE', #3911 ) ;
#27481 = AXIS2_PLACEMENT_3D ( 'NONE', #10066, #24973, #13663 ) ;
#27482 = CARTESIAN_POINT ( 'NONE',  ( 0.8965959638259385356, 1.582931917743541028, 9.903764339332076005 ) ) ;
#27483 = CARTESIAN_POINT ( 'NONE',  ( 0.1287570809895630941, -0.3962735484563133515, -10.00000000000000000 ) ) ;
#27484 = DIRECTION ( 'NONE',  ( -1.000000000000000000, 0.000000000000000000, -0.000000000000000000 ) ) ;
#27485 = CYLINDRICAL_SURFACE ( 'NONE', #15715, 1.750000000000015543 ) ;
#27486 = ORIENTED_EDGE ( 'NONE', *, *, #37740, .T. ) ;
#27487 = CARTESIAN_POINT ( 'NONE',  ( -13.92102703536724384, -30.85732372859812500, 8.356839323120299312 ) ) ;
#27488 = DIRECTION ( 'NONE',  ( 0.000000000000000000, 0.000000000000000000, -1.000000000000000000 ) ) ;
#27489 = EDGE_CURVE ( 'NONE', #1426, #25177, #19552, .T. ) ;
#27490 = CYLINDRICAL_SURFACE ( 'NONE', #28900, 1.749999999999973799 ) ;
#27491 = VERTEX_POINT ( 'NONE', #80 ) ;
#27492 = VERTEX_POINT ( 'NONE', #39849 ) ;
#27493 = APPLICATION_PROTOCOL_DEFINITION ( 'draft international standard', 'automotive_design', 1998, #42372 ) ;
#27494 = DIRECTION ( 'NONE',  ( -0.000000000000000000, -0.000000000000000000, -1.000000000000000000 ) ) ;
#27495 = CARTESIAN_POINT ( 'NONE',  ( 1.637465050678285294, 0.1702693745679431936, 9.936700280135958963 ) ) ;
#27496 = AXIS2_PLACEMENT_3D ( 'NONE', #12923, #48038, #1150 ) ;
#27497 = CYLINDRICAL_SURFACE ( 'NONE', #14382, 1.749999999999973799 ) ;
#27498 = DIRECTION ( 'NONE',  ( 0.000000000000000000, -1.000000000000000000, 0.000000000000000000 ) ) ;
#27499 = ADVANCED_FACE ( 'NONE', ( #4683 ), #20576, .T. ) ;
#27500 = VECTOR ( 'NONE', #16907, 1000.000000000000000 ) ;
#27501 = CARTESIAN_POINT ( 'NONE',  ( -166.6959734468149463, 1.750000000000010214, 40.81828755692798438 ) ) ;
#27502 = ORIENTED_EDGE ( 'NONE', *, *, #37460, .F. ) ;
#27503 = CARTESIAN_POINT ( 'NONE',  ( 31.28977333267368621, -11.25592690310905652, -2.408242355805840784 ) ) ;
#27504 = DIRECTION ( 'NONE',  ( -1.000000000000000000, 0.000000000000000000, 0.000000000000000000 ) ) ;
#27505 = FACE_OUTER_BOUND ( 'NONE', #21709, .T. ) ;
#27506 = CARTESIAN_POINT ( 'NONE',  ( 0.5111101921243742519, 1.175566515482123098, 9.957892297621016908 ) ) ;
#27507 = AXIS2_PLACEMENT_3D ( 'NONE', #39216, #4054, #216 ) ;
#27509 = ORIENTED_EDGE ( 'NONE', *, *, #41644, .F. ) ;
#27508 = EDGE_CURVE ( 'NONE', #42902, #39284, #25184, .T. ) ;
#27510 = CARTESIAN_POINT ( 'NONE',  ( 151.5540265531850537, 0.000000000000000000, -40.93171244307202983 ) ) ;
#27511 = ADVANCED_FACE ( 'NONE', ( #20821 ), #9034, .T. ) ;
#27512 = ORIENTED_EDGE ( 'NONE', *, *, #33461, .T. ) ;
#27513 = CARTESIAN_POINT ( 'NONE',  ( -210.0000000000000568, 2.143131898507880377E-16, -0.9317124430720331585 ) ) ;
#27514 = VECTOR ( 'NONE', #18936, 1000.000000000000000 ) ;
#27515 = ORIENTED_EDGE ( 'NONE', *, *, #40862, .T. ) ;
#27516 = CARTESIAN_POINT ( 'NONE',  ( -19.99999999999815969, 17.00000000000000000, 90.00000000000000000 ) ) ;
#27517 = LINE ( 'NONE', #47471, #19175 ) ;
#27518 = EDGE_CURVE ( 'NONE', #14142, #45927, #31891, .T. ) ;
#27519 = CARTESIAN_POINT ( 'NONE',  ( 350.0000000000000000, -184.9999999999999716, -344.0000000000001705 ) ) ;
#27520 = DIRECTION ( 'NONE',  ( -1.000000000000000000, -0.000000000000000000, -0.000000000000000000 ) ) ;
#27521 = VECTOR ( 'NONE', #14028, 1000.000000000000000 ) ;
#27522 = VERTEX_POINT ( 'NONE', #5424 ) ;
#27523 = VECTOR ( 'NONE', #49850, 1000.000000000000000 ) ;
#27524 = EDGE_CURVE ( 'NONE', #13193, #27616, #29035, .T. ) ;
#27525 = EDGE_CURVE ( 'NONE', #48817, #9702, #16144, .T. ) ;
#27526 =( BOUNDED_CURVE ( )  B_SPLINE_CURVE ( 3, ( #12358, #40329, #24183, #36498 ),
 .UNSPECIFIED., .F., .F. ) 
 B_SPLINE_CURVE_WITH_KNOTS ( ( 4, 4 ),
 ( 0.000000000000000000, 1.570796326794896780 ),
 .UNSPECIFIED. ) 
 CURVE ( )  GEOMETRIC_REPRESENTATION_ITEM ( )  RATIONAL_B_SPLINE_CURVE ( ( 1.000000000000000000, 0.8047378541243649375, 0.8047378541243649375, 1.000000000000000000 ) ) 
 REPRESENTATION_ITEM ( '' )  );
#27527 = DIRECTION ( 'NONE',  ( 0.000000000000000000, -1.000000000000000000, 0.000000000000000000 ) ) ;
#27528 = DIRECTION ( 'NONE',  ( 0.000000000000000000, -1.000000000000000000, -1.544785076050074834E-48 ) ) ;
#27529 = ORIENTED_EDGE ( 'NONE', *, *, #999, .T. ) ;
#27530 = CARTESIAN_POINT ( 'NONE',  ( 181.0000000000000000, -95.49999999999997158, -115.0000000000001563 ) ) ;
#27531 = FACE_OUTER_BOUND ( 'NONE', #17097, .T. ) ;
#27532 = PLANE ( 'NONE',  #15594 ) ;
#27533 = PLANE ( 'NONE',  #11929 ) ;
#27534 =( BOUNDED_CURVE ( )  B_SPLINE_CURVE ( 3, ( #22489, #17629, #34054, #33548 ),
 .UNSPECIFIED., .F., .F. ) 
 B_SPLINE_CURVE_WITH_KNOTS ( ( 4, 4 ),
 ( 3.141592653589793116, 4.712388980384689674 ),
 .UNSPECIFIED. ) 
 CURVE ( )  GEOMETRIC_REPRESENTATION_ITEM ( )  RATIONAL_B_SPLINE_CURVE ( ( 1.000000000000000000, 0.8047378541243649375, 0.8047378541243649375, 1.000000000000000000 ) ) 
 REPRESENTATION_ITEM ( '' )  );
#27535 = EDGE_CURVE ( 'NONE', #23241, #43972, #1807, .T. ) ;
#27536 = ORIENTED_EDGE ( 'NONE', *, *, #41596, .F. ) ;
#27537 = EDGE_LOOP ( 'NONE', ( #7549, #14187, #27350, #34330 ) ) ;
#27538 = CYLINDRICAL_SURFACE ( 'NONE', #3810, 1.750000000000008438 ) ;
#27539 = VECTOR ( 'NONE', #649, 1000.000000000000000 ) ;
#27540 = VERTEX_POINT ( 'NONE', #28783 ) ;
#27541 = CARTESIAN_POINT ( 'NONE',  ( 36.70770892944851482, -7.840405911381885140, 6.057468652304065060 ) ) ;
#27542 = CARTESIAN_POINT ( 'NONE',  ( -206.6959734468149463, -1.750000000000010658, -119.1817124430720440 ) ) ;
#27543 = LINE ( 'NONE', #43179, #3487 ) ;
#27544 = VECTOR ( 'NONE', #35831, 1000.000000000000000 ) ;
#27545 = VERTEX_POINT ( 'NONE', #44407 ) ;
#27546 = CARTESIAN_POINT ( 'NONE',  ( -15.73090589902298042, -29.60029367929041655, 1.847720168420772691 ) ) ;
#27547 = ORIENTED_EDGE ( 'NONE', *, *, #26805, .T. ) ;
#27548 =( BOUNDED_CURVE ( )  B_SPLINE_CURVE ( 3, ( #30330, #49772, #22876, #45941 ),
 .UNSPECIFIED., .F., .F. ) 
 B_SPLINE_CURVE_WITH_KNOTS ( ( 4, 4 ),
 ( 1.570796326794896558, 3.141592653589793116 ),
 .UNSPECIFIED. ) 
 CURVE ( )  GEOMETRIC_REPRESENTATION_ITEM ( )  RATIONAL_B_SPLINE_CURVE ( ( 1.000000000000000000, 0.8047378541243649375, 0.8047378541243649375, 1.000000000000000000 ) ) 
 REPRESENTATION_ITEM ( '' )  );
#27549 = DIRECTION ( 'NONE',  ( 0.000000000000000000, -0.000000000000000000, -1.000000000000000000 ) ) ;
#27550 = DIRECTION ( 'NONE',  ( 1.000000000000000000, 0.000000000000000000, 0.000000000000000000 ) ) ;
#27552 = AXIS2_PLACEMENT_3D ( 'NONE', #10172, #29927, #2470 ) ;
#27551 = CARTESIAN_POINT ( 'NONE',  ( -206.6959734468149463, -1.750000000000010658, 120.8182875569279702 ) ) ;
#27553 = ORIENTED_EDGE ( 'NONE', *, *, #28345, .F. ) ;
#27554 = ORIENTED_EDGE ( 'NONE', *, *, #13566, .F. ) ;
#27555 = EDGE_LOOP ( 'NONE', ( #29518, #43698, #45828, #44733, #2024, #18980 ) ) ;
#27556 = CARTESIAN_POINT ( 'NONE',  ( -7.884183412771427868, -42.26678417219198991, 893.0811050474360400 ) ) ;
#27557 = CARTESIAN_POINT ( 'NONE',  ( -84.94597344681494633, 2.143131898507880377E-16, -40.93171244307202983 ) ) ;
#27558 = CARTESIAN_POINT ( 'NONE',  ( 2.052581215100350853, -0.2042358160480859663, 9.886433018048069954 ) ) ;
#27559 = ORIENTED_EDGE ( 'NONE', *, *, #20505, .T. ) ;
#27560 = LINE ( 'NONE', #40118, #1838 ) ;
#27561 = ORIENTED_EDGE ( 'NONE', *, *, #12648, .T. ) ;
#27562 = EDGE_CURVE ( 'NONE', #16052, #40932, #40829, .T. ) ;
#27563 = VECTOR ( 'NONE', #280, 1000.000000000000000 ) ;
#27564 = CARTESIAN_POINT ( 'NONE',  ( -165.3973046169136012, -67.00570555996102939, -94.69675437945474528 ) ) ;
#27565 = ORIENTED_EDGE ( 'NONE', *, *, #31292, .F. ) ;
#27566 =( NAMED_UNIT ( * ) PLANE_ANGLE_UNIT ( ) SI_UNIT ( $, .RADIAN. ) );
#27567 = DIRECTION ( 'NONE',  ( 1.000000000000000000, -0.000000000000000000, 1.860490536778032451E-50 ) ) ;
#27568 = CARTESIAN_POINT ( 'NONE',  ( -7.721099712662037540, 1.750000000000023315, -118.1565861772249519 ) ) ;
#27569 = CARTESIAN_POINT ( 'NONE',  ( 181.0000000000000284, -174.9999999999999716, -111.0000000000001563 ) ) ;
#27570 = CARTESIAN_POINT ( 'NONE',  ( -2.538055338523177440, -50.00000000000000711, -9.367992836599954742 ) ) ;
#27571 = CARTESIAN_POINT ( 'NONE',  ( 344.0000000000000000, -165.0000000000001137, -340.0000000000003411 ) ) ;
#27572 = ORIENTED_EDGE ( 'NONE', *, *, #38408, .T. ) ;
#27573 = ORIENTED_EDGE ( 'NONE', *, *, #16369, .T. ) ;
#27574 = DIRECTION ( 'NONE',  ( 0.000000000000000000, -1.000000000000000000, 0.000000000000000000 ) ) ;
#27575 = CARTESIAN_POINT ( 'NONE',  ( 23.79193388295309219, 28.98609808355011452, -9.422646554964176246 ) ) ;
#27576 = DIRECTION ( 'NONE',  ( -1.000000000000000000, -0.000000000000000000, -0.000000000000000000 ) ) ;
#27577 = AXIS2_PLACEMENT_3D ( 'NONE', #29861, #21915, #2649 ) ;
#27578 = EDGE_CURVE ( 'NONE', #48573, #38406, #44042, .T. ) ;
#27579 = CARTESIAN_POINT ( 'NONE',  ( -33.43156050989129824, 4.370686678976795747, 8.807470649214879543 ) ) ;
#27580 = EDGE_CURVE ( 'NONE', #18060, #48199, #21077, .T. ) ;
#27581 = VECTOR ( 'NONE', #29484, 1000.000000000000000 ) ;
#27582 = CARTESIAN_POINT ( 'NONE',  ( -14.76429217231967428, -8.192625680377590314, 9.178419661560148768 ) ) ;
#27583 = ORIENTED_EDGE ( 'NONE', *, *, #36339, .F. ) ;
#27584 = CARTESIAN_POINT ( 'NONE',  ( -164.9999999999990905, 17.00000000000000000, -24.99999999999999289 ) ) ;
#27585 = DIRECTION ( 'NONE',  ( -0.1671032855531390249, 0.5142910309547715775, 0.8411784753765542133 ) ) ;
#27586 = EDGE_CURVE ( 'NONE', #6873, #37811, #33158, .T. ) ;
#27587 = EDGE_CURVE ( 'NONE', #23962, #27903, #1341, .T. ) ;
#27588 = ORIENTED_EDGE ( 'NONE', *, *, #9544, .T. ) ;
#27589 = CIRCLE ( 'NONE', #18545, 2.000000000000001776 ) ;
#27590 = CARTESIAN_POINT ( 'NONE',  ( -128.4459734468149179, 0.000000000000000000, -37.43171244307205825 ) ) ;
#27591 = VECTOR ( 'NONE', #29688, 1000.000000000000000 ) ;
#27592 = DIRECTION ( 'NONE',  ( 0.000000000000000000, -1.000000000000000000, 3.469446951953611033E-15 ) ) ;
#27593 = EDGE_CURVE ( 'NONE', #41767, #22392, #38206, .T. ) ;
#27594 = CARTESIAN_POINT ( 'NONE',  ( 9.998889670239195837, 0.1490146381531976816, 9.282506307616472441 ) ) ;
#27595 = ORIENTED_EDGE ( 'NONE', *, *, #25244, .T. ) ;
#27596 = VERTEX_POINT ( 'NONE', #10037 ) ;
#27597 = DIRECTION ( 'NONE',  ( -1.000000000000000000, 0.000000000000000000, 0.000000000000000000 ) ) ;
#27598 = VECTOR ( 'NONE', #34412, 1000.000000000000000 ) ;
#27599 = DIRECTION ( 'NONE',  ( 1.000000000000000000, 0.000000000000000000, 0.000000000000000000 ) ) ;
#27600 = ORIENTED_EDGE ( 'NONE', *, *, #9797, .T. ) ;
#27601 = ORIENTED_EDGE ( 'NONE', *, *, #3763, .F. ) ;
#27602 = CARTESIAN_POINT ( 'NONE',  ( -124.9459734468149463, 2.143131898507847836E-16, 39.06828755692798438 ) ) ;
#27603 = CARTESIAN_POINT ( 'NONE',  ( 36.08557433729230723, -35.58569447144768105, 7.455576670931136185 ) ) ;
#27604 = CARTESIAN_POINT ( 'NONE',  ( 0.9599924130074096729, -0.8495346730527926216, 9.948547179989617462 ) ) ;
#27605 = DIRECTION ( 'NONE',  ( -1.586032892321652236E-16, -1.000000000000000000, -2.288264760618012091E-48 ) ) ;
#27606 = ORIENTED_EDGE ( 'NONE', *, *, #40659, .T. ) ;
#27607 = ORIENTED_EDGE ( 'NONE', *, *, #1892, .F. ) ;
#27608 = VERTEX_POINT ( 'NONE', #32639 ) ;
#27609 = LINE ( 'NONE', #32216, #16879 ) ;
#27610 = ORIENTED_EDGE ( 'NONE', *, *, #46137, .F. ) ;
#27611 = DIRECTION ( 'NONE',  ( 0.000000000000000000, 0.000000000000000000, -1.000000000000000000 ) ) ;
#27612 = VECTOR ( 'NONE', #49693, 1000.000000000000000 ) ;
#27613 = CARTESIAN_POINT ( 'NONE',  ( 40.00000000000000000, 7.564790863224921225, 897.6604670114604687 ) ) ;
#27614 = DIRECTION ( 'NONE',  ( 0.000000000000000000, 0.000000000000000000, -1.000000000000000000 ) ) ;
#27615 = ORIENTED_EDGE ( 'NONE', *, *, #38680, .F. ) ;
#27616 = VERTEX_POINT ( 'NONE', #48231 ) ;
#27617 = CARTESIAN_POINT ( 'NONE',  ( 111.5540265531850537, 1.025126265847081442, 159.0682875569279418 ) ) ;
#27618 = ADVANCED_FACE ( 'NONE', ( #32901 ), #13375, .T. ) ;
#27619 = CARTESIAN_POINT ( 'NONE',  ( 1.962712821592840662, 1.022159834731142691, 9.881002359080275355 ) ) ;
#27620 = LINE ( 'NONE', #43248, #6020 ) ;
#27621 = ORIENTED_EDGE ( 'NONE', *, *, #14417, .T. ) ;
#27622 = EDGE_LOOP ( 'NONE', ( #32517, #19741, #15783, #50519 ) ) ;
#27623 = EDGE_CURVE ( 'NONE', #13738, #41411, #41086, .T. ) ;
#27624 = CARTESIAN_POINT ( 'NONE',  ( 165.0000000000000000, -174.9999999999999716, -115.0000000000001563 ) ) ;
#27625 = LINE ( 'NONE', #47576, #11683 ) ;
#27626 = ORIENTED_EDGE ( 'NONE', *, *, #12797, .F. ) ;
#27627 = DIRECTION ( 'NONE',  ( -1.000000000000000000, 0.000000000000000000, 0.000000000000000000 ) ) ;
#27628 = DIRECTION ( 'NONE',  ( -0.000000000000000000, -1.000000000000000000, -0.000000000000000000 ) ) ;
#27629 = DIRECTION ( 'NONE',  ( 0.1191452206184307611, 0.000000000000000000, -0.9928768384869220975 ) ) ;
#27630 =( BOUNDED_CURVE ( )  B_SPLINE_CURVE ( 3, ( #50088, #14999, #30658, #31169 ),
 .UNSPECIFIED., .F., .F. ) 
 B_SPLINE_CURVE_WITH_KNOTS ( ( 4, 4 ),
 ( 4.712388980384689674, 6.283185307179586232 ),
 .UNSPECIFIED. ) 
 CURVE ( )  GEOMETRIC_REPRESENTATION_ITEM ( )  RATIONAL_B_SPLINE_CURVE ( ( 1.000000000000000000, 0.8047378541243649375, 0.8047378541243649375, 1.000000000000000000 ) ) 
 REPRESENTATION_ITEM ( '' )  );
#27631 = DIRECTION ( 'NONE',  ( 0.000000000000000000, 0.000000000000000000, 1.000000000000000000 ) ) ;
#27632 = VERTEX_POINT ( 'NONE', #17740 ) ;
#27633 = CARTESIAN_POINT ( 'NONE',  ( 7.749480817862238524, 14.85497772329518895, 9.403735324607438884 ) ) ;
#27634 = DIRECTION ( 'NONE',  ( -1.000000000000000000, -0.000000000000000000, -0.000000000000000000 ) ) ;
#27635 = CARTESIAN_POINT ( 'NONE',  ( 152.2789002873379900, -1.750000000000009548, -38.15658617722494483 ) ) ;
#27636 = AXIS2_PLACEMENT_3D ( 'NONE', #49560, #30373, #10609 ) ;
#27637 = CARTESIAN_POINT ( 'NONE',  ( 166.9999999999999716, -272.5000000000000000, -98.99999999999874944 ) ) ;
#27638 = CARTESIAN_POINT ( 'NONE',  ( -33.86622497129646092, 3.037805405905158462, 7.906207997025717304 ) ) ;
#27639 = CARTESIAN_POINT ( 'NONE',  ( 45.64490844644690526, 21.32281559348795597, 8.807470649214879543 ) ) ;
#27640 = EDGE_LOOP ( 'NONE', ( #29764, #21553, #46348, #43712, #17685, #35564 ) ) ;
#27641 = FILL_AREA_STYLE_COLOUR ( '', #12526 ) ;
#27642 = VECTOR ( 'NONE', #9429, 1000.000000000000000 ) ;
#27643 = CARTESIAN_POINT ( 'NONE',  ( -119.9999999999981668, 17.00000000000000000, 65.00000000000000000 ) ) ;
#27644 = ORIENTED_EDGE ( 'NONE', *, *, #15135, .F. ) ;
#27645 = CARTESIAN_POINT ( 'NONE',  ( -4.999999999999997335, 204.9999999999999716, -230.2499999999999716 ) ) ;
#27646 = EDGE_CURVE ( 'NONE', #25388, #19871, #33406, .T. ) ;
#27647 = CARTESIAN_POINT ( 'NONE',  ( 339.9999999999999432, 174.9999999999996589, -344.0000000000002842 ) ) ;
#27648 = ORIENTED_EDGE ( 'NONE', *, *, #39037, .T. ) ;
#27649 = CARTESIAN_POINT ( 'NONE',  ( -165.6708471809677974, -1.750000000000009548, -118.1565861772249519 ) ) ;
#27650 = VERTEX_POINT ( 'NONE', #26948 ) ;
#27651 = ORIENTED_EDGE ( 'NONE', *, *, #23634, .T. ) ;
#27652 = CARTESIAN_POINT ( 'NONE',  ( 46.75893035013449861, 17.89420872045614885, 3.199614146704519602 ) ) ;
#27653 = CARTESIAN_POINT ( 'NONE',  ( -86.69597344681494633, -1.750000000000010214, -39.18171244307202983 ) ) ;
#27654 = EDGE_LOOP ( 'NONE', ( #21760, #42234, #7700, #43908, #9518, #5427 ) ) ;
#27655 = CARTESIAN_POINT ( 'NONE',  ( 356.0000000000001137, 165.0000000000000000, 349.9999999999998295 ) ) ;
#27656 = CARTESIAN_POINT ( 'NONE',  ( 350.0000000000000000, 183.0000000000000284, -344.0000000000001705 ) ) ;
#27657 = DIRECTION ( 'NONE',  ( 1.000000000000000000, 0.000000000000000000, 0.000000000000000000 ) ) ;
#27658 = ORIENTED_EDGE ( 'NONE', *, *, #34452, .T. ) ;
#27659 = FACE_OUTER_BOUND ( 'NONE', #11622, .T. ) ;
#27660 = FILL_AREA_STYLE_COLOUR ( '', #11941 ) ;
#27661 = ORIENTED_EDGE ( 'NONE', *, *, #42894, .F. ) ;
#27662 = CARTESIAN_POINT ( 'NONE',  ( 358.0000000000000000, -169.0000000000001137, -344.0000000000002842 ) ) ;
#27663 = FACE_OUTER_BOUND ( 'NONE', #26826, .T. ) ;
#27664 = VERTEX_POINT ( 'NONE', #14390 ) ;
#27665 = VERTEX_POINT ( 'NONE', #3592 ) ;
#27666 = VERTEX_POINT ( 'NONE', #42583 ) ;
#27667 = CARTESIAN_POINT ( 'NONE',  ( -1.249999999999999778, 0.000000000000000000, 10.00000000000000000 ) ) ;
#27668 = DIRECTION ( 'NONE',  ( 0.000000000000000000, -1.000000000000000000, -3.186989995019654210E-49 ) ) ;
#27669 = EDGE_LOOP ( 'NONE', ( #1767, #33524, #44536, #26576, #21863, #32153 ) ) ;
#27670 = CARTESIAN_POINT ( 'NONE',  ( -206.6959734468149463, -1.750000000000010658, 80.81828755692798438 ) ) ;
#27671 = CYLINDRICAL_SURFACE ( 'NONE', #33618, 2.000000000000001776 ) ;
#27672 = CARTESIAN_POINT ( 'NONE',  ( -44.99506233596265048, -23.32283626942287569, 7.455576670931136185 ) ) ;
#27673 =( BOUNDED_CURVE ( )  B_SPLINE_CURVE ( 3, ( #11442, #43243, #50392, #11694 ),
 .UNSPECIFIED., .F., .F. ) 
 B_SPLINE_CURVE_WITH_KNOTS ( ( 4, 4 ),
 ( 3.141592653589793116, 4.712388980384689674 ),
 .UNSPECIFIED. ) 
 CURVE ( )  GEOMETRIC_REPRESENTATION_ITEM ( )  RATIONAL_B_SPLINE_CURVE ( ( 1.000000000000000000, 0.8047378541243649375, 0.8047378541243649375, 1.000000000000000000 ) ) 
 REPRESENTATION_ITEM ( '' )  );
#27674 = FACE_OUTER_BOUND ( 'NONE', #24738, .T. ) ;
#27675 = CARTESIAN_POINT ( 'NONE',  ( -84.94597344681493212, 1.025126265847088991, 162.5682875569279133 ) ) ;
#27676 = AXIS2_PLACEMENT_3D ( 'NONE', #44003, #39434, #8627 ) ;
#27677 = FACE_OUTER_BOUND ( 'NONE', #8904, .T. ) ;
#27678 = CARTESIAN_POINT ( 'NONE',  ( -1.377551617740987888, 0.6025367262284248016, 9.936141075690080982 ) ) ;
#27679 = CARTESIAN_POINT ( 'NONE',  ( 41.18776771165112649, -7.147140551973409472, 8.846626183609803462 ) ) ;
#27680 = LINE ( 'NONE', #27428, #49542 ) ;
#27681 =( BOUNDED_CURVE ( )  B_SPLINE_CURVE ( 3, ( #48071, #8378, #27878, #47823 ),
 .UNSPECIFIED., .F., .F. ) 
 B_SPLINE_CURVE_WITH_KNOTS ( ( 4, 4 ),
 ( 3.141592653589793116, 4.712388980384689674 ),
 .UNSPECIFIED. ) 
 CURVE ( )  GEOMETRIC_REPRESENTATION_ITEM ( )  RATIONAL_B_SPLINE_CURVE ( ( 1.000000000000000000, 0.8047378541243649375, 0.8047378541243649375, 1.000000000000000000 ) ) 
 REPRESENTATION_ITEM ( '' )  );
#27682 = CARTESIAN_POINT ( 'NONE',  ( 36.28567981536807707, 9.465698090293649614, -9.422646554964174470 ) ) ;
#27683 = DIRECTION ( 'NONE',  ( -0.1191452206184307749, 0.000000000000000000, 0.9928768384869220975 ) ) ;
#27684 = CARTESIAN_POINT ( 'NONE',  ( 85.00000000000213163, 17.00000000000000000, 115.0000000000000142 ) ) ;
#27685 = CARTESIAN_POINT ( 'NONE',  ( -164.9459734468149463, 2.143131898507880377E-16, 165.0000000000000000 ) ) ;
#27686 = B_SPLINE_CURVE_WITH_KNOTS ( 'NONE', 3,
 ( #43497, #8367, #4507, #24273 ),
 .UNSPECIFIED., .F., .F.,
 ( 4, 4 ),
 ( 3.824391573920122509E-16, 0.009762429722931327200 ),
 .UNSPECIFIED. ) ;
#27687 = CARTESIAN_POINT ( 'NONE',  ( -10.49999999999999467, -46.01315789473684248, -5.916985404131817283 ) ) ;
#27688 = CARTESIAN_POINT ( 'NONE',  ( 350.0000000000000000, -180.9999999999999716, -358.0000000000002274 ) ) ;
#27689 = ORIENTED_EDGE ( 'NONE', *, *, #17091, .F. ) ;
#27690 = CARTESIAN_POINT ( 'NONE',  ( 168.9999999999999716, 8.000000000000062172, 339.9999999999998295 ) ) ;
#27691 = AXIS2_PLACEMENT_3D ( 'NONE', #30651, #26290, #45500 ) ;
#27692 = LINE ( 'NONE', #20242, #5646 ) ;
#27693 = CARTESIAN_POINT ( 'NONE',  ( 193.3040265531851105, -1.750000000000010658, -119.1817124430720440 ) ) ;
#27694 = FACE_OUTER_BOUND ( 'NONE', #50357, .T. ) ;
#27695 = ORIENTED_EDGE ( 'NONE', *, *, #24733, .T. ) ;
#27696 =( LENGTH_UNIT ( ) NAMED_UNIT ( * ) SI_UNIT ( .MILLI., .METRE. ) );
#27697 = ORIENTED_EDGE ( 'NONE', *, *, #34002, .F. ) ;
#27698 = ADVANCED_FACE ( 'NONE', ( #42340, #19237 ), #34407, .F. ) ;
#27699 = CARTESIAN_POINT ( 'NONE',  ( -69.99999999999783995, 17.00000000000000000, 95.00000000000000000 ) ) ;
#27700 = VERTEX_POINT ( 'NONE', #46416 ) ;
#27701 = CYLINDRICAL_SURFACE ( 'NONE', #37754, 2.000000000000001776 ) ;
#27702 = EDGE_CURVE ( 'NONE', #31054, #48005, #45908, .T. ) ;
#27703 = CARTESIAN_POINT ( 'NONE',  ( 193.3040265531851105, 1.750000000000010658, 120.8182875569279702 ) ) ;
#27704 = EDGE_LOOP ( 'NONE', ( #27202, #21903, #36580, #46091 ) ) ;
#27705 = CARTESIAN_POINT ( 'NONE',  ( -69.99999999999879208, 17.00000000000000000, 30.00000000000000000 ) ) ;
#27706 = ORIENTED_EDGE ( 'NONE', *, *, #39961, .F. ) ;
#27707 = EDGE_CURVE ( 'NONE', #41718, #44615, #22840, .T. ) ;
#27708 = EDGE_CURVE ( 'NONE', #33144, #4629, #35191, .T. ) ;
#27709 = VECTOR ( 'NONE', #4336, 1000.000000000000000 ) ;
#27710 = ORIENTED_EDGE ( 'NONE', *, *, #10135, .T. ) ;
#27711 = DIRECTION ( 'NONE',  ( -1.000000000000000000, 0.000000000000000000, 0.000000000000000000 ) ) ;
#27712 = CARTESIAN_POINT ( 'NONE',  ( 339.9999999999999432, -169.0000000000001137, -344.0000000000002842 ) ) ;
#27713 = ORIENTED_EDGE ( 'NONE', *, *, #6379, .F. ) ;
#27714 = FACE_OUTER_BOUND ( 'NONE', #24336, .T. ) ;
#27715 = DIRECTION ( 'NONE',  ( -0.000000000000000000, -0.000000000000000000, -1.000000000000000000 ) ) ;
#27716 = CARTESIAN_POINT ( 'NONE',  ( -7.822422304254325276, -2.816136035261162185, 229.0000000000000000 ) ) ;
#27717 = EDGE_CURVE ( 'NONE', #27106, #5103, #30812, .T. ) ;
#27718 = CARTESIAN_POINT ( 'NONE',  ( 1.153670525509248312, 0.4304314044324303867, 9.975326647350893694 ) ) ;
#27719 = PLANE ( 'NONE',  #49291 ) ;
#27720 = EDGE_CURVE ( 'NONE', #6739, #22212, #30299, .T. ) ;
#27721 = ORIENTED_EDGE ( 'NONE', *, *, #18115, .F. ) ;
#27722 = CARTESIAN_POINT ( 'NONE',  ( 210.0000000000000568, 0.000000000000000000, 82.56828755692799859 ) ) ;
#27723 = CARTESIAN_POINT ( 'NONE',  ( 155.0540265531850537, -1.025126265847089435, 39.06828755692797728 ) ) ;
#27724 = ORIENTED_EDGE ( 'NONE', *, *, #49624, .F. ) ;
#27725 = DIRECTION ( 'NONE',  ( -1.000000000000000000, -0.000000000000000000, -0.000000000000000000 ) ) ;
#27726 = CARTESIAN_POINT ( 'NONE',  ( 27.25836557470631760, -25.76317754842347796, 8.100132398494510610 ) ) ;
#27727 = B_SPLINE_SURFACE_WITH_KNOTS ( 'NONE', 3, 3, ( 
 ( #34903, #11022, #27190, #22821 ),
 ( #50482, #38501, #3314, #15389 ),
 ( #11542, #42818, #256, #4823 ),
 ( #12048, #4347, #36158, #16640 ) ),
 .UNSPECIFIED., .F., .F., .F.,
 ( 4, 4 ),
 ( 4, 4 ),
 ( 0.000000000000000000, 1.000000000000000000 ),
 ( 0.000000000000000000, 1.000000000000000000 ),
 .UNSPECIFIED. ) ;
#27728 = EDGE_CURVE ( 'NONE', #17801, #7259, #11046, .T. ) ;
#27729 = ORIENTED_EDGE ( 'NONE', *, *, #12107, .F. ) ;
#27730 = EDGE_CURVE ( 'NONE', #42669, #34694, #7464, .T. ) ;
#27731 = DIRECTION ( 'NONE',  ( 0.000000000000000000, 0.000000000000000000, 1.000000000000000000 ) ) ;
#27732 = DIRECTION ( 'NONE',  ( -0.000000000000000000, -1.000000000000000000, -0.000000000000000000 ) ) ;
#27733 = LINE ( 'NONE', #27981, #11484 ) ;
#27734 = EDGE_CURVE ( 'NONE', #41244, #24564, #14897, .T. ) ;
#27735 = EDGE_CURVE ( 'NONE', #40073, #34466, #26194, .T. ) ;
#27736 = ORIENTED_EDGE ( 'NONE', *, *, #14612, .T. ) ;
#27737 = CARTESIAN_POINT ( 'NONE',  ( -46.69597344681494633, 0.000000000000000000, 165.0000000000000000 ) ) ;
#27738 = EDGE_CURVE ( 'NONE', #40327, #960, #10788, .T. ) ;
#27739 = DIRECTION ( 'NONE',  ( -0.000000000000000000, -1.000000000000000000, -0.000000000000000000 ) ) ;
#27740 = EDGE_CURVE ( 'NONE', #343, #25937, #29792, .T. ) ;
#27741 = CARTESIAN_POINT ( 'NONE',  ( 14.52758583651987223, 8.922352469211173087, 8.953103998512858652 ) ) ;
#27742 = VERTEX_POINT ( 'NONE', #37760 ) ;
#27743 = ORIENTED_EDGE ( 'NONE', *, *, #21843, .T. ) ;
#27744 = DIRECTION ( 'NONE',  ( -1.754668910725352053E-14, 9.050558009225903070E-17, -1.000000000000000000 ) ) ;
#27745 = DIRECTION ( 'NONE',  ( 1.000000000000000000, 1.156482317317870492E-16, -0.000000000000000000 ) ) ;
#27746 = CARTESIAN_POINT ( 'NONE',  ( 14.49999999999999822, -46.01315789473684248, -5.916985404131817283 ) ) ;
#27747 = VECTOR ( 'NONE', #10133, 1000.000000000000000 ) ;
#27748 = CARTESIAN_POINT ( 'NONE',  ( -1.011271242968693862, 0.7347315653655780432, -3.333333333333333481 ) ) ;
#27749 = ORIENTED_EDGE ( 'NONE', *, *, #37839, .F. ) ;
#27750 = CARTESIAN_POINT ( 'NONE',  ( -119.9999999999987921, 17.00000000000000000, 30.00000000000000000 ) ) ;
#27751 = DIRECTION ( 'NONE',  ( -0.000000000000000000, -0.000000000000000000, -1.000000000000000000 ) ) ;
#27752 = FACE_OUTER_BOUND ( 'NONE', #5990, .T. ) ;
#27753 = VECTOR ( 'NONE', #6218, 1000.000000000000000 ) ;
#27754 = EDGE_CURVE ( 'NONE', #4028, #17487, #2577, .T. ) ;
#27755 = DIRECTION ( 'NONE',  ( -1.000000000000000000, -0.000000000000000000, -0.000000000000000000 ) ) ;
#27756 = ORIENTED_EDGE ( 'NONE', *, *, #15031, .F. ) ;
#27757 = EDGE_CURVE ( 'NONE', #45661, #33640, #28576, .T. ) ;
#27758 = CARTESIAN_POINT ( 'NONE',  ( -84.94597344681494633, 2.143131898507880377E-16, 2.568287556927978166 ) ) ;
#27759 = VERTEX_POINT ( 'NONE', #45658 ) ;
#27760 = EDGE_CURVE ( 'NONE', #36434, #47506, #15266, .T. ) ;
#27761 = DIRECTION ( 'NONE',  ( -1.000000000000000000, 0.000000000000000000, 0.000000000000000000 ) ) ;
#27762 = ORIENTED_EDGE ( 'NONE', *, *, #3410, .T. ) ;
#27763 = CARTESIAN_POINT ( 'NONE',  ( 1.011271242968688311, -0.7347315653655855927, 10.00000000000000000 ) ) ;
#27764 = DIRECTION ( 'NONE',  ( 0.000000000000000000, 0.000000000000000000, -1.000000000000000000 ) ) ;
#27765 = DIRECTION ( 'NONE',  ( -1.000000000000000000, -0.000000000000000000, -0.000000000000000000 ) ) ;
#27766 = CARTESIAN_POINT ( 'NONE',  ( 193.3040265531851105, 1.750000000000010214, 40.81828755692798438 ) ) ;
#27767 = ORIENTED_EDGE ( 'NONE', *, *, #40945, .T. ) ;
#27768 = EDGE_CURVE ( 'NONE', #47057, #45409, #19431, .T. ) ;
#27769 = DIRECTION ( 'NONE',  ( 0.000000000000000000, 0.000000000000000000, -1.000000000000000000 ) ) ;
#27770 = CARTESIAN_POINT ( 'NONE',  ( 152.2789002873379900, 1.750000000000009548, -78.15658617722490931 ) ) ;
#27771 = ORIENTED_EDGE ( 'NONE', *, *, #33730, .F. ) ;
#27772 = CARTESIAN_POINT ( 'NONE',  ( 80.00000000000092371, 16.00000000000000000, 0.000000000000000000 ) ) ;
#27773 = DIRECTION ( 'NONE',  ( -0.000000000000000000, -1.000000000000000000, -0.000000000000000000 ) ) ;
#27774 = CARTESIAN_POINT ( 'NONE',  ( 210.0000000000000568, 2.143131898507880377E-16, 159.0682875569279702 ) ) ;
#27775 = FACE_OUTER_BOUND ( 'NONE', #49450, .T. ) ;
#27776 = ORIENTED_EDGE ( 'NONE', *, *, #4611, .F. ) ;
#27777 = ORIENTED_EDGE ( 'NONE', *, *, #14535, .F. ) ;
#27778 = DIRECTION ( 'NONE',  ( 0.6904757466825007794, 0.7233555441435720601, -0.000000000000000000 ) ) ;
#27779 = EDGE_CURVE ( 'NONE', #41040, #12195, #15894, .T. ) ;
#27780 = AXIS2_PLACEMENT_3D ( 'NONE', #3229, #18877, #34558 ) ;
#27781 = ORIENTED_EDGE ( 'NONE', *, *, #47915, .T. ) ;
#27782 = CARTESIAN_POINT ( 'NONE',  ( -45.67084718096785423, -1.750000000000009548, -78.15658617722490931 ) ) ;
#27783 = LINE ( 'NONE', #39595, #1061 ) ;
#27784 = ADVANCED_FACE ( 'NONE', ( #3082 ), #47666, .T. ) ;
#27785 = ORIENTED_EDGE ( 'NONE', *, *, #48139, .F. ) ;
#27787 = AXIS2_PLACEMENT_3D ( 'NONE', #12845, #47953, #25160 ) ;
#27786 = CARTESIAN_POINT ( 'NONE',  ( -12.78770032058971395, -31.68259716188267916, 7.455576670931136185 ) ) ;
#27788 = VERTEX_POINT ( 'NONE', #31583 ) ;
#27789 = ORIENTED_EDGE ( 'NONE', *, *, #14067, .F. ) ;
#27790 = CARTESIAN_POINT ( 'NONE',  ( 240.0000000000000000, -164.9999999999999716, 444.9999999999998295 ) ) ;
#27791 = VECTOR ( 'NONE', #2027, 1000.000000000000000 ) ;
#27792 = CARTESIAN_POINT ( 'NONE',  ( -6.880036658038867436, 222.4999999999999716, -228.6347188485896140 ) ) ;
#27793 = ADVANCED_FACE ( 'NONE', ( #35692 ), #11816, .F. ) ;
#27795 = EDGE_LOOP ( 'NONE', ( #37408, #33898, #30368, #36828 ) ) ;
#27794 = EDGE_CURVE ( 'NONE', #43115, #43496, #20008, .T. ) ;
#27796 = VERTEX_POINT ( 'NONE', #8221 ) ;
#27797 = VERTEX_POINT ( 'NONE', #42837 ) ;
#27798 = FACE_OUTER_BOUND ( 'NONE', #40436, .T. ) ;
#27799 = CYLINDRICAL_SURFACE ( 'NONE', #491, 1.750000000000001554 ) ;
#27800 = DIRECTION ( 'NONE',  ( -1.000000000000000000, 0.000000000000000000, 0.000000000000000000 ) ) ;
#27801 = EDGE_CURVE ( 'NONE', #35970, #4444, #2928, .T. ) ;
#27802 = B_SPLINE_CURVE_WITH_KNOTS ( 'NONE', 3,
 ( #11831, #23881, #19771, #35711 ),
 .UNSPECIFIED., .F., .F.,
 ( 4, 4 ),
 ( 0.000000000000000000, 0.0001252128669263212913 ),
 .UNSPECIFIED. ) ;
#27803 = PRODUCT_DEFINITION_CONTEXT ( 'detailed design', #10904, 'design' ) ;
#27804 = EDGE_LOOP ( 'NONE', ( #38017, #39969, #38834, #13911 ) ) ;
#27805 = CARTESIAN_POINT ( 'NONE',  ( -7.721099712662037540, -1.750000000000023315, -0.2068387089191201234 ) ) ;
#27806 = ORIENTED_EDGE ( 'NONE', *, *, #37334, .F. ) ;
#27807 = EDGE_CURVE ( 'NONE', #48103, #37518, #42648, .T. ) ;
#27808 = CARTESIAN_POINT ( 'NONE',  ( -31.28234235046239320, -11.28615439405757392, -3.760136334089591248 ) ) ;
#27809 = ORIENTED_EDGE ( 'NONE', *, *, #14067, .T. ) ;
#27810 = EDGE_CURVE ( 'NONE', #26042, #16866, #8475, .T. ) ;
#27811 = DIRECTION ( 'NONE',  ( 1.860490536778032451E-50, 0.000000000000000000, -1.000000000000000000 ) ) ;
#27812 = FACE_OUTER_BOUND ( 'NONE', #10779, .T. ) ;
#27813 = CARTESIAN_POINT ( 'NONE',  ( 33.30402655318503946, -1.750000000000009992, 160.8182875569279702 ) ) ;
#27814 = CARTESIAN_POINT ( 'NONE',  ( -0.5000000000000000000, 0.5000000000000000000, 1000.000000000000000 ) ) ;
#27815 = CARTESIAN_POINT ( 'NONE',  ( 358.0000000000000000, -169.0000000000001137, 344.0000000000000000 ) ) ;
#27816 = CARTESIAN_POINT ( 'NONE',  ( 168.9999999999999716, 175.0000000000000284, -344.0000000000001137 ) ) ;
#27817 = EDGE_LOOP ( 'NONE', ( #20846, #40412, #22879, #12688, #36637, #15153 ) ) ;
#27818 = VERTEX_POINT ( 'NONE', #276 ) ;
#27819 = CARTESIAN_POINT ( 'NONE',  ( -48.44597344681496054, -1.025126265847089435, 2.568287556927986159 ) ) ;
#27820 = PLANE ( 'NONE',  #35965 ) ;
#27821 = CARTESIAN_POINT ( 'NONE',  ( -42.99990394833793061, 47.95759300784327905, -5.000000000000000000 ) ) ;
#27822 = AXIS2_PLACEMENT_3D ( 'NONE', #29389, #45008, #36621 ) ;
#27823 =( BOUNDED_CURVE ( )  B_SPLINE_CURVE ( 3, ( #36252, #24444, #48235, #40093 ),
 .UNSPECIFIED., .F., .F. ) 
 B_SPLINE_CURVE_WITH_KNOTS ( ( 4, 4 ),
 ( 1.570796326794896558, 3.141592653589793116 ),
 .UNSPECIFIED. ) 
 CURVE ( )  GEOMETRIC_REPRESENTATION_ITEM ( )  RATIONAL_B_SPLINE_CURVE ( ( 1.000000000000000000, 0.8047378541243649375, 0.8047378541243649375, 1.000000000000000000 ) ) 
 REPRESENTATION_ITEM ( '' )  );
#27824 = AXIS2_PLACEMENT_3D ( 'NONE', #5225, #20875, #29086 ) ;
#27825 = PLANE ( 'NONE',  #29787 ) ;
#27826 = EDGE_CURVE ( 'NONE', #15345, #3809, #39528, .T. ) ;
#27827 = CARTESIAN_POINT ( 'NONE',  ( 33.30402655318503946, -1.750000000000010214, 40.81828755692798438 ) ) ;
#27828 = MECHANICAL_DESIGN_GEOMETRIC_PRESENTATION_REPRESENTATION (  '', ( #14697 ), #48350 ) ;
#27829 = ORIENTED_EDGE ( 'NONE', *, *, #19007, .T. ) ;
#27830 = VECTOR ( 'NONE', #16143, 1000.000000000000000 ) ;
#27831 = CARTESIAN_POINT ( 'NONE',  ( -208.4459734468149463, 0.000000000000000000, 165.0000000000000000 ) ) ;
#27832 =( BOUNDED_CURVE ( )  B_SPLINE_CURVE ( 3, ( #4408, #20055, #36484, #1068 ),
 .UNSPECIFIED., .F., .F. ) 
 B_SPLINE_CURVE_WITH_KNOTS ( ( 4, 4 ),
 ( 0.000000000000000000, 1.570796326794896558 ),
 .UNSPECIFIED. ) 
 CURVE ( )  GEOMETRIC_REPRESENTATION_ITEM ( )  RATIONAL_B_SPLINE_CURVE ( ( 1.000000000000000000, 0.8047378541243649375, 0.8047378541243649375, 1.000000000000000000 ) ) 
 REPRESENTATION_ITEM ( '' )  );
#27833 = CARTESIAN_POINT ( 'NONE',  ( 7.499999999999944045, -224.9999999999999716, -240.0000000000000000 ) ) ;
#27834 = ORIENTED_EDGE ( 'NONE', *, *, #12596, .F. ) ;
#27835 = CARTESIAN_POINT ( 'NONE',  ( 1.158497635116737312, -16.61944452314319420, -3.546734833711462365 ) ) ;
#27836 = DIRECTION ( 'NONE',  ( 0.000000000000000000, 0.000000000000000000, -1.000000000000000000 ) ) ;
#27837 = CARTESIAN_POINT ( 'NONE',  ( 35.00000000000028422, 16.00000000000000000, -84.99999999999998579 ) ) ;
#27838 = B_SPLINE_CURVE_WITH_KNOTS ( 'NONE', 3,
 ( #27558, #23450, #43194, #16755 ),
 .UNSPECIFIED., .F., .F.,
 ( 4, 4 ),
 ( 0.001937412222931639630, 0.003978261222106106373 ),
 .UNSPECIFIED. ) ;
#27839 =( BOUNDED_CURVE ( )  B_SPLINE_CURVE ( 3, ( #23112, #14654, #41605, #41856 ),
 .UNSPECIFIED., .F., .F. ) 
 B_SPLINE_CURVE_WITH_KNOTS ( ( 4, 4 ),
 ( 3.141592653589793116, 4.712388980384689674 ),
 .UNSPECIFIED. ) 
 CURVE ( )  GEOMETRIC_REPRESENTATION_ITEM ( )  RATIONAL_B_SPLINE_CURVE ( ( 1.000000000000000000, 0.8047378541243649375, 0.8047378541243649375, 1.000000000000000000 ) ) 
 REPRESENTATION_ITEM ( '' )  );
#27840 = ORIENTED_EDGE ( 'NONE', *, *, #12171, .T. ) ;
#27841 = PRODUCT_DEFINITION_SHAPE ( 'NONE', 'NONE',  #50737 ) ;
#27842 = ORIENTED_EDGE ( 'NONE', *, *, #46011, .F. ) ;
#27843 = CARTESIAN_POINT ( 'NONE',  ( 195.0540265531851105, 2.143131898507880377E-16, -77.43171244307204404 ) ) ;
#27844 = B_SPLINE_CURVE_WITH_KNOTS ( 'NONE', 3,
 ( #39913, #24503, #40409, #4743 ),
 .UNSPECIFIED., .F., .F.,
 ( 4, 4 ),
 ( 0.000000000000000000, 0.2637263876330695478 ),
 .UNSPECIFIED. ) ;
#27845 = CARTESIAN_POINT ( 'NONE',  ( -46.69597344681494633, 1.750000000000009992, -159.1817124430720298 ) ) ;
#27846 = ORIENTED_EDGE ( 'NONE', *, *, #19605, .F. ) ;
#27847 = VERTEX_POINT ( 'NONE', #35180 ) ;
#27848 = LINE ( 'NONE', #35824, #44968 ) ;
#27849 = CARTESIAN_POINT ( 'NONE',  ( -0.3862712429686977478, 1.188820645368937390, 10.00000000000000000 ) ) ;
#27850 = CARTESIAN_POINT ( 'NONE',  ( 193.3040265531851105, 0.000000000000000000, 165.0000000000000000 ) ) ;
#27851 = CARTESIAN_POINT ( 'NONE',  ( 0.3896797354184660667, -1.262193838292004155, 9.943883492372872723 ) ) ;
#27852 = FACE_OUTER_BOUND ( 'NONE', #44595, .T. ) ;
#27853 = ORIENTED_EDGE ( 'NONE', *, *, #25511, .F. ) ;
#27854 = ORIENTED_EDGE ( 'NONE', *, *, #47110, .F. ) ;
#27855 = EDGE_LOOP ( 'NONE', ( #36604, #17802 ) ) ;
#27856 = VECTOR ( 'NONE', #1834, 1000.000000000000000 ) ;
#27857 = CARTESIAN_POINT ( 'NONE',  ( 344.0000000000000568, 183.0000000000000284, 349.9999999999998863 ) ) ;
#27858 = AXIS2_PLACEMENT_3D ( 'NONE', #32516, #36109, #48094 ) ;
#27859 = ORIENTED_EDGE ( 'NONE', *, *, #44865, .T. ) ;
#27860 = EDGE_CURVE ( 'NONE', #12051, #7897, #32445, .T. ) ;
#27861 = ADVANCED_FACE ( 'NONE', ( #4622 ), #23355, .T. ) ;
#27862 = CARTESIAN_POINT ( 'NONE',  ( 1.114871695981101585, -0.4953159757246433093, 9.963925895596188909 ) ) ;
#27863 = ORIENTED_EDGE ( 'NONE', *, *, #24019, .T. ) ;
#27864 = ORIENTED_EDGE ( 'NONE', *, *, #16150, .F. ) ;
#27865 = CARTESIAN_POINT ( 'NONE',  ( -8.445973446814962315, -1.025126265847096985, -160.9317124430720014 ) ) ;
#27866 = VECTOR ( 'NONE', #32343, 1000.000000000000000 ) ;
#27867 = CARTESIAN_POINT ( 'NONE',  ( 6.174150299305392053, -33.14591993373988998, 8.807470649214879543 ) ) ;
#27868 = DIRECTION ( 'NONE',  ( 0.5407575913134975432, 0.000000000000000000, 0.8411784753765542133 ) ) ;
#27869 = EDGE_CURVE ( 'NONE', #7708, #19185, #15408, .T. ) ;
#27870 = ORIENTED_EDGE ( 'NONE', *, *, #24635, .F. ) ;
#27871 = ORIENTED_EDGE ( 'NONE', *, *, #943, .T. ) ;
#27872 = EDGE_CURVE ( 'NONE', #1058, #27141, #28167, .T. ) ;
#27873 = CARTESIAN_POINT ( 'NONE',  ( 1.377636575563020438, -0.6021164824561170414, 9.953784399990622589 ) ) ;
#27874 = SURFACE_STYLE_USAGE ( .BOTH. , #420 ) ;
#27875 = ORIENTED_EDGE ( 'NONE', *, *, #4635, .F. ) ;
#27876 = EDGE_CURVE ( 'NONE', #24506, #7778, #26330, .T. ) ;
#27877 = CARTESIAN_POINT ( 'NONE',  ( -64.99999999999971578, 17.00000000000000000, -84.99999999999998579 ) ) ;
#27878 = CARTESIAN_POINT ( 'NONE',  ( 152.2789002873379900, 1.750000000000009548, 121.8434138227750623 ) ) ;
#27879 = DIRECTION ( 'NONE',  ( 0.000000000000000000, 0.2791762785758810650, -0.9602398687205827565 ) ) ;
#27880 = DIRECTION ( 'NONE',  ( -1.000000000000000000, 0.000000000000000000, 0.000000000000000000 ) ) ;
#27881 = ORIENTED_EDGE ( 'NONE', *, *, #18964, .T. ) ;
#27882 = CARTESIAN_POINT ( 'NONE',  ( 2.143303323993648313, -0.2858885274053867276, 9.882710035074774524 ) ) ;
#27883 = CARTESIAN_POINT ( 'NONE',  ( 192.2789002873380184, 1.750000000000010436, -120.2068387089191219 ) ) ;
#27884 = EDGE_CURVE ( 'NONE', #14400, #47608, #27964, .T. ) ;
#27885 = DIRECTION ( 'NONE',  ( -1.000000000000000000, -0.000000000000000000, -0.000000000000000000 ) ) ;
#27886 = LINE ( 'NONE', #28388, #48389 ) ;
#27887 = B_SPLINE_CURVE_WITH_KNOTS ( 'NONE', 3,
 ( #50253, #15164, #30824, #3605 ),
 .UNSPECIFIED., .F., .F.,
 ( 4, 4 ),
 ( 0.0001265805828163032185, 0.0005567784772122129572 ),
 .UNSPECIFIED. ) ;
#27888 = CARTESIAN_POINT ( 'NONE',  ( 349.9999999999999432, -184.9999999999999716, 355.9999999999997726 ) ) ;
#27889 = FACE_OUTER_BOUND ( 'NONE', #24789, .T. ) ;
#27890 = CIRCLE ( 'NONE', #49946, 1.750000000000001554 ) ;
#27891 = CARTESIAN_POINT ( 'NONE',  ( -0.3862712429686809279, -1.188820645368943163, 10.00000000000000000 ) ) ;
#27892 = VECTOR ( 'NONE', #28636, 1000.000000000000000 ) ;
#27893 = ORIENTED_EDGE ( 'NONE', *, *, #30285, .F. ) ;
#27894 = LINE ( 'NONE', #8885, #19074 ) ;
#27895 = AXIS2_PLACEMENT_3D ( 'NONE', #8267, #7769, #8023 ) ;
#27896 = CARTESIAN_POINT ( 'NONE',  ( 185.0000000000000000, -9.999999999999953815, -111.0000000000001563 ) ) ;
#27897 = ORIENTED_EDGE ( 'NONE', *, *, #8643, .F. ) ;
#27898 = PLANE ( 'NONE',  #34389 ) ;
#27899 = DIRECTION ( 'NONE',  ( 0.000000000000000000, -0.000000000000000000, 1.000000000000000000 ) ) ;
#27900 = AXIS2_PLACEMENT_3D ( 'NONE', #7347, #23761, #15310 ) ;
#27901 = LINE ( 'NONE', #4293, #45438 ) ;
#27902 = AXIS2_PLACEMENT_3D ( 'NONE', #16127, #35395, #12268 ) ;
#27903 = VERTEX_POINT ( 'NONE', #31324 ) ;
#27904 = CARTESIAN_POINT ( 'NONE',  ( -164.9459734468149463, 2.143131898507880377E-16, -117.4317124430720725 ) ) ;
#27905 = EDGE_LOOP ( 'NONE', ( #23123, #24016, #15549, #11201 ) ) ;
#27906 = VERTEX_POINT ( 'NONE', #4853 ) ;
#27907 = CARTESIAN_POINT ( 'NONE',  ( 194.9999999999999432, -172.9999999999999716, 252.0000000000000568 ) ) ;
#27908 = EDGE_CURVE ( 'NONE', #25084, #37811, #9497, .T. ) ;
#27909 = DIRECTION ( 'NONE',  ( 1.000000000000000000, 0.000000000000000000, 0.000000000000000000 ) ) ;
#27910 = ORIENTED_EDGE ( 'NONE', *, *, #33383, .F. ) ;
#27911 = CARTESIAN_POINT ( 'NONE',  ( 2.816440797479290659, -7.430518950464442440, 9.432811472610140413 ) ) ;
#27912 = CARTESIAN_POINT ( 'NONE',  ( 175.0000000000000000, 15.00000000000000000, 122.5000000000000142 ) ) ;
#27913 = ORIENTED_EDGE ( 'NONE', *, *, #10239, .T. ) ;
#27914 = CARTESIAN_POINT ( 'NONE',  ( 75.05402655318509630, 2.143131898507880377E-16, 82.56828755692799859 ) ) ;
#27915 = ORIENTED_EDGE ( 'NONE', *, *, #28018, .T. ) ;
#27916 = CARTESIAN_POINT ( 'NONE',  ( 339.9999999999999432, 171.9999999999999432, -347.0000000000000568 ) ) ;
#27917 = SURFACE_STYLE_FILL_AREA ( #43552 ) ;
#27918 = ORIENTED_EDGE ( 'NONE', *, *, #39438, .F. ) ;
#27919 = FACE_OUTER_BOUND ( 'NONE', #22155, .T. ) ;
#27920 = CARTESIAN_POINT ( 'NONE',  ( 0.000000000000000000, 0.000000000000000000, 900.0000000000000000 ) ) ;
#27921 = ORIENTED_EDGE ( 'NONE', *, *, #37480, .T. ) ;
#27922 = EDGE_LOOP ( 'NONE', ( #50565, #32385, #19877, #6635 ) ) ;
#27923 = ORIENTED_EDGE ( 'NONE', *, *, #23813, .F. ) ;
#27924 = CARTESIAN_POINT ( 'NONE',  ( -8.445973446814976526, 0.000000000000000000, 159.0682875569279418 ) ) ;
#27925 = DIRECTION ( 'NONE',  ( 1.000000000000000000, 0.000000000000000000, 0.000000000000000000 ) ) ;
#27926 = VERTEX_POINT ( 'NONE', #36958 ) ;
#27927 = VECTOR ( 'NONE', #28906, 1000.000000000000000 ) ;
#27928 = LINE ( 'NONE', #39737, #25440 ) ;
#27929 = DIRECTION ( 'NONE',  ( 0.4740998230350172427, -0.3386427307392981256, -0.8127425537743157014 ) ) ;
#27930 = CARTESIAN_POINT ( 'NONE',  ( 30.00000000000217781, 17.00000000000000000, 95.00000000000000000 ) ) ;
#27931 = CARTESIAN_POINT ( 'NONE',  ( -88.44597344681494633, -1.025126265847089213, 159.0682875569279418 ) ) ;
#27932 = CARTESIAN_POINT ( 'NONE',  ( -7.216980890441389462, 6.922079660550276792, 0.000000000000000000 ) ) ;
#27933 = LINE ( 'NONE', #20231, #21624 ) ;
#27935 = EDGE_CURVE ( 'NONE', #33351, #17600, #29229, .T. ) ;
#27934 = CARTESIAN_POINT ( 'NONE',  ( 31.44259251615245176, 38.95901822126168668, -9.367992836599951190 ) ) ;
#27936 = CARTESIAN_POINT ( 'NONE',  ( 1.565984505217804967, -1.491012526244388292, 9.885585981620945262 ) ) ;
#27937 = CARTESIAN_POINT ( 'NONE',  ( 34.10310225234744763, 15.68274378628490773, 1.982731392810414661 ) ) ;
#27938 = CIRCLE ( 'NONE', #35319, 2.000000000000001776 ) ;
#27939 = DIRECTION ( 'NONE',  ( 0.9928768384869219865, 0.000000000000000000, 0.1191452206184307611 ) ) ;
#27940 = LINE ( 'NONE', #47893, #21612 ) ;
#27941 = CARTESIAN_POINT ( 'NONE',  ( 356.0000000000000000, 185.0000000000000284, -360.0000000000002274 ) ) ;
#27942 = DIRECTION ( 'NONE',  ( -0.000000000000000000, -0.000000000000000000, -1.000000000000000000 ) ) ;
#27943 = ORIENTED_EDGE ( 'NONE', *, *, #10378, .T. ) ;
#27944 = CARTESIAN_POINT ( 'NONE',  ( 356.0000000000000000, 165.0000000000001705, -340.0000000000002842 ) ) ;
#27945 = PLANE ( 'NONE',  #23677 ) ;
#27946 = CARTESIAN_POINT ( 'NONE',  ( 80.00000000000122213, 17.00000000000000000, 5.000000000000004441 ) ) ;
#27947 = CARTESIAN_POINT ( 'NONE',  ( 48.33712804702526000, 13.03701565032775456, -9.367992836599954742 ) ) ;
#27948 = ORIENTED_EDGE ( 'NONE', *, *, #2321, .T. ) ;
#27949 = CARTESIAN_POINT ( 'NONE',  ( 153.3040265531850537, 0.000000000000000000, 165.0000000000000000 ) ) ;
#27950 = CARTESIAN_POINT ( 'NONE',  ( -1.468713901642213493, -0.3220470327672489419, 9.927319414211227766 ) ) ;
#27951 = ORIENTED_EDGE ( 'NONE', *, *, #48358, .T. ) ;
#27952 = DIRECTION ( 'NONE',  ( -1.000000000000000000, 0.000000000000000000, -0.000000000000000000 ) ) ;
#27953 = CARTESIAN_POINT ( 'NONE',  ( 210.0000000000000568, 0.000000000000000000, 122.5682875569279844 ) ) ;
#27954 = CARTESIAN_POINT ( 'NONE',  ( -46.69597344681494633, 1.750000000000009992, 0.8182875569279768335 ) ) ;
#27955 = ORIENTED_EDGE ( 'NONE', *, *, #39944, .F. ) ;
#27956 = CARTESIAN_POINT ( 'NONE',  ( -207.7210997126620384, 1.750000000000009548, 159.7931612910809065 ) ) ;
#27957 = EDGE_LOOP ( 'NONE', ( #9672, #25137, #5603, #26800 ) ) ;
#27958 = EDGE_CURVE ( 'NONE', #46160, #42683, #28375, .T. ) ;
#27959 = VECTOR ( 'NONE', #34124, 1000.000000000000000 ) ;
#27960 = ORIENTED_EDGE ( 'NONE', *, *, #8270, .T. ) ;
#27961 = DIRECTION ( 'NONE',  ( 1.000000000000000000, -4.758098676964956461E-16, -8.975803739141899931E-48 ) ) ;
#27962 = ORIENTED_EDGE ( 'NONE', *, *, #42189, .T. ) ;
#27963 = CARTESIAN_POINT ( 'NONE',  ( -22.82242230425432439, -2.816136035261162185, 226.0000000000000000 ) ) ;
#27964 = LINE ( 'NONE', #24382, #34950 ) ;
#27965 = VECTOR ( 'NONE', #8137, 1000.000000000000000 ) ;
#27966 = CARTESIAN_POINT ( 'NONE',  ( 85.00000000000213163, 16.00000000000000000, 95.00000000000000000 ) ) ;
#27967 = VECTOR ( 'NONE', #8834, 1000.000000000000000 ) ;
#27968 = CARTESIAN_POINT ( 'NONE',  ( -164.9459734468149463, 2.143131898507880377E-16, -117.4317124430720725 ) ) ;
#27969 = EDGE_LOOP ( 'NONE', ( #38945, #26705, #33332, #22966, #7954 ) ) ;
#27970 = DIRECTION ( 'NONE',  ( 1.000000000000000000, 0.000000000000000000, 0.000000000000000000 ) ) ;
#27971 = VERTEX_POINT ( 'NONE', #28477 ) ;
#27972 = FACE_OUTER_BOUND ( 'NONE', #18546, .T. ) ;
#27973 = CARTESIAN_POINT ( 'NONE',  ( 356.0000000000001137, 183.0000000000000284, 349.9999999999998295 ) ) ;
#27974 = ORIENTED_EDGE ( 'NONE', *, *, #46763, .F. ) ;
#27975 = FACE_OUTER_BOUND ( 'NONE', #46581, .T. ) ;
#27976 =( BOUNDED_CURVE ( )  B_SPLINE_CURVE ( 3, ( #1688, #28623, #35852, #43513 ),
 .UNSPECIFIED., .F., .F. ) 
 B_SPLINE_CURVE_WITH_KNOTS ( ( 4, 4 ),
 ( 4.712388980384689674, 6.283185307179586232 ),
 .UNSPECIFIED. ) 
 CURVE ( )  GEOMETRIC_REPRESENTATION_ITEM ( )  RATIONAL_B_SPLINE_CURVE ( ( 1.000000000000000000, 0.8047378541243649375, 0.8047378541243649375, 1.000000000000000000 ) ) 
 REPRESENTATION_ITEM ( '' )  );
#27977 = CARTESIAN_POINT ( 'NONE',  ( -88.44597344681497475, 0.000000000000000000, 119.0682875569279418 ) ) ;
#27978 = ORIENTED_EDGE ( 'NONE', *, *, #44046, .T. ) ;
#27979 = CARTESIAN_POINT ( 'NONE',  ( 42.07173315646062406, -18.54977254542396636, -8.016098858316205167 ) ) ;
#27980 = CARTESIAN_POINT ( 'NONE',  ( 169.0000000000000000, -174.9999999999999716, -95.00000000000014211 ) ) ;
#27981 = CARTESIAN_POINT ( 'NONE',  ( -8.445973446814976526, 0.000000000000000000, 165.0000000000000000 ) ) ;
#27982 = ORIENTED_EDGE ( 'NONE', *, *, #9507, .T. ) ;
#27983 = DIRECTION ( 'NONE',  ( 0.000000000000000000, -1.000000000000000000, 0.000000000000000000 ) ) ;
#27985 = EDGE_CURVE ( 'NONE', #28555, #24870, #48671, .T. ) ;
#27984 = CARTESIAN_POINT ( 'NONE',  ( 358.0000000000000000, 175.0000000000000284, -106.0000000000001990 ) ) ;
#27986 = AXIS2_PLACEMENT_3D ( 'NONE', #27026, #7798, #18804 ) ;
#27987 = CARTESIAN_POINT ( 'NONE',  ( 0.3370904143228947158, 0.2449105217885311492, 10.00000000000000000 ) ) ;
#27988 = ORIENTED_EDGE ( 'NONE', *, *, #30567, .F. ) ;
#27989 = ORIENTED_EDGE ( 'NONE', *, *, #22195, .T. ) ;
#27990 = DIRECTION ( 'NONE',  ( -1.000000000000000000, -0.000000000000000000, -0.000000000000000000 ) ) ;
#27991 = CARTESIAN_POINT ( 'NONE',  ( 355.9999999999999432, -174.9999999999999432, 355.9999999999998295 ) ) ;
#27992 = DIRECTION ( 'NONE',  ( 0.000000000000000000, 0.000000000000000000, 1.000000000000000000 ) ) ;
#27993 = CARTESIAN_POINT ( 'NONE',  ( -127.7210997126620242, -1.749999999999996891, 81.84341382277506227 ) ) ;
#27994 = LINE ( 'NONE', #23644, #17477 ) ;
#27995 = ORIENTED_EDGE ( 'NONE', *, *, #29599, .F. ) ;
#27996 = CARTESIAN_POINT ( 'NONE',  ( -120.0000000000000426, 17.00000000000000000, -114.9999999999999858 ) ) ;
#27997 = EDGE_CURVE ( 'NONE', #22310, #29971, #26923, .T. ) ;
#27998 = ADVANCED_FACE ( 'NONE', ( #36182 ), #37206, .T. ) ;
#28000 = VECTOR ( 'NONE', #15706, 1000.000000000000000 ) ;
#27999 = CARTESIAN_POINT ( 'NONE',  ( 164.9999999999999716, 16.00000000000000000, 115.0000000000000142 ) ) ;
#28001 = CARTESIAN_POINT ( 'NONE',  ( -164.9459734468149463, 2.143131898507880377E-16, 159.0682875569279702 ) ) ;
#28003 = ADVANCED_FACE ( 'NONE', ( #32840 ), #9717, .T. ) ;
#28002 = DIRECTION ( 'NONE',  ( -1.000000000000000000, -0.000000000000000000, -0.000000000000000000 ) ) ;
#28004 = ADVANCED_FACE ( 'NONE', ( #40275 ), #40776, .F. ) ;
#28005 = ORIENTED_EDGE ( 'NONE', *, *, #1126, .F. ) ;
#28006 = DIRECTION ( 'NONE',  ( 0.000000000000000000, 0.000000000000000000, 1.000000000000000000 ) ) ;
#28007 = ORIENTED_EDGE ( 'NONE', *, *, #26877, .T. ) ;
#28008 = DIRECTION ( 'NONE',  ( -0.000000000000000000, -0.000000000000000000, -1.000000000000000000 ) ) ;
#28009 = EDGE_LOOP ( 'NONE', ( #3426, #34363, #47854, #38429 ) ) ;
#28010 = DIRECTION ( 'NONE',  ( -1.000000000000000000, -0.000000000000000000, -0.000000000000000000 ) ) ;
#28011 = FACE_OUTER_BOUND ( 'NONE', #15595, .T. ) ;
#28012 = EDGE_CURVE ( 'NONE', #49667, #39568, #18353, .T. ) ;
#28013 = LINE ( 'NONE', #4415, #42878 ) ;
#28014 = CARTESIAN_POINT ( 'NONE',  ( -19.99999999999971223, 17.00000000000000000, -84.99999999999998579 ) ) ;
#28015 = EDGE_CURVE ( 'NONE', #2747, #14851, #44346, .T. ) ;
#28016 = ORIENTED_EDGE ( 'NONE', *, *, #35351, .T. ) ;
#28017 = EDGE_CURVE ( 'NONE', #2042, #41270, #29920, .T. ) ;
#28018 = EDGE_CURVE ( 'NONE', #46031, #11650, #44098, .T. ) ;
#28019 = CARTESIAN_POINT ( 'NONE',  ( 151.5540265531850537, 0.000000000000000000, -117.4317124430720725 ) ) ;
#28020 = DIRECTION ( 'NONE',  ( -0.5407575913134975432, -0.000000000000000000, 0.8411784753765542133 ) ) ;
#28021 = ORIENTED_EDGE ( 'NONE', *, *, #19643, .T. ) ;
#28022 = CARTESIAN_POINT ( 'NONE',  ( -0.8284317003875021346, -1.889026769141635587, 9.889206917020304743 ) ) ;
#28023 = CARTESIAN_POINT ( 'NONE',  ( 31.55402655318503236, 0.000000000000000000, 42.56828755692798438 ) ) ;
#28024 = CARTESIAN_POINT ( 'NONE',  ( 167.0000000000000284, 175.0000000000000284, 355.9999999999998863 ) ) ;
#28025 = FACE_OUTER_BOUND ( 'NONE', #30301, .T. ) ;
#28026 = CIRCLE ( 'NONE', #4260, 0.4999999999999996114 ) ;
#28027 = EDGE_CURVE ( 'NONE', #33254, #41585, #16661, .T. ) ;
#28028 = ORIENTED_EDGE ( 'NONE', *, *, #48983, .F. ) ;
#28029 = ORIENTED_EDGE ( 'NONE', *, *, #46279, .F. ) ;
#28030 = CARTESIAN_POINT ( 'NONE',  ( 50.00000000000000000, 50.00000000000000000, 900.0000000000000000 ) ) ;
#28031 = VERTEX_POINT ( 'NONE', #16933 ) ;
#28032 = AXIS2_PLACEMENT_3D ( 'NONE', #22941, #19083, #50348 ) ;
#28033 = CARTESIAN_POINT ( 'NONE',  ( 181.0000000000000568, -164.9999999999999432, 357.9999999999998863 ) ) ;
#28034 = CARTESIAN_POINT ( 'NONE',  ( 183.0000000000000284, -174.9999999999999716, -99.00000000000014211 ) ) ;
#28035 = CARTESIAN_POINT ( 'NONE',  ( -210.0000000000000568, 0.000000000000000000, 160.8182875569279702 ) ) ;
#28036 = ORIENTED_EDGE ( 'NONE', *, *, #28439, .T. ) ;
#28037 = B_SPLINE_CURVE_WITH_KNOTS ( 'NONE', 3,
 ( #28710, #25117, #16648, #40764 ),
 .UNSPECIFIED., .F., .F.,
 ( 4, 4 ),
 ( 0.000000000000000000, 0.2545280377015990969 ),
 .UNSPECIFIED. ) ;
#28038 = ADVANCED_FACE ( 'NONE', ( #49616 ), #8971, .T. ) ;
#28039 = CARTESIAN_POINT ( 'NONE',  ( -6.619412807845042046, 7.495556955913086128, 9.646707543097347681 ) ) ;
#28040 = CARTESIAN_POINT ( 'NONE',  ( 154.1026953830863420, -98.56198943095992604, -17.65743994998277699 ) ) ;
#28041 = ADVANCED_FACE ( 'NONE', ( #12819 ), #32257, .T. ) ;
#28042 = ORIENTED_EDGE ( 'NONE', *, *, #9209, .T. ) ;
#28043 = EDGE_CURVE ( 'NONE', #9239, #19835, #25076, .T. ) ;
#28044 = ORIENTED_EDGE ( 'NONE', *, *, #44608, .T. ) ;
#28045 = ORIENTED_EDGE ( 'NONE', *, *, #32712, .T. ) ;
#28046 = LINE ( 'NONE', #40114, #27150 ) ;
#28048 = EDGE_CURVE ( 'NONE', #40908, #32767, #3459, .T. ) ;
#28047 = CARTESIAN_POINT ( 'NONE',  ( -4.945973446814916130, -1.025126265847097207, 122.5682875569280128 ) ) ;
#28049 = CARTESIAN_POINT ( 'NONE',  ( 135.0000000000006253, 16.00000000000000000, -30.00000000000000000 ) ) ;
#28050 = AXIS2_PLACEMENT_3D ( 'NONE', #1416, #4993, #47304 ) ;
#28051 = EDGE_LOOP ( 'NONE', ( #46594, #28926, #40042, #5340 ) ) ;
#28052 = CARTESIAN_POINT ( 'NONE',  ( 358.0000000000000000, 169.0000000000001705, -344.0000000000002842 ) ) ;
#28053 = ORIENTED_EDGE ( 'NONE', *, *, #22075, .F. ) ;
#28054 = EDGE_CURVE ( 'NONE', #8236, #49488, #22613, .T. ) ;
#28055 = DIRECTION ( 'NONE',  ( -1.000000000000000000, -0.000000000000000000, 2.312964634635864737E-16 ) ) ;
#28056 = ORIENTED_EDGE ( 'NONE', *, *, #34538, .T. ) ;
#28057 = CARTESIAN_POINT ( 'NONE',  ( 1.724908962443185922, -9.880865948510580310, 9.516222621873128062 ) ) ;
#28058 = DIRECTION ( 'NONE',  ( 1.000000000000000000, 0.000000000000000000, 0.000000000000000000 ) ) ;
#28059 = LINE ( 'NONE', #4457, #14655 ) ;
#28060 = DIRECTION ( 'NONE',  ( 1.000000000000000000, 0.000000000000000000, 0.000000000000000000 ) ) ;
#28061 = FACE_OUTER_BOUND ( 'NONE', #42335, .T. ) ;
#28062 = DIRECTION ( 'NONE',  ( 0.000000000000000000, 0.000000000000000000, 1.000000000000000000 ) ) ;
#28063 = EDGE_LOOP ( 'NONE', ( #29252, #1430 ) ) ;
#28064 = ORIENTED_EDGE ( 'NONE', *, *, #44603, .T. ) ;
#28065 = FACE_OUTER_BOUND ( 'NONE', #41069, .T. ) ;
#28066 = VECTOR ( 'NONE', #16512, 1000.000000000000000 ) ;
#28067 = CARTESIAN_POINT ( 'NONE',  ( 339.9999999999998863, -168.9999999999999432, 355.9999999999997726 ) ) ;
#28068 = CARTESIAN_POINT ( 'NONE',  ( 214.9999999999999432, -317.3964497041420145, 132.2485207100591253 ) ) ;
#28069 = DIRECTION ( 'NONE',  ( -1.000000000000000000, -0.000000000000000000, -0.000000000000000000 ) ) ;
#28070 = B_SPLINE_CURVE_WITH_KNOTS ( 'NONE', 3,
 ( #34026, #45776, #38384, #14761 ),
 .UNSPECIFIED., .F., .F.,
 ( 4, 4 ),
 ( 0.9890644561681873892, 1.000000000000000000 ),
 .UNSPECIFIED. ) ;
#28071 = VECTOR ( 'NONE', #5245, 1000.000000000000000 ) ;
#28072 = ADVANCED_FACE ( 'NONE', ( #27081 ), #22965, .T. ) ;
#28073 = LINE ( 'NONE', #5471, #28615 ) ;
#28074 = ORIENTED_EDGE ( 'NONE', *, *, #30838, .T. ) ;
#28075 = CYLINDRICAL_SURFACE ( 'NONE', #35230, 4.000000000000003553 ) ;
#28076 = CARTESIAN_POINT ( 'NONE',  ( 195.0540265531851105, 2.143131898507880377E-16, -160.9317124430720014 ) ) ;
#28077 = EDGE_CURVE ( 'NONE', #37476, #2131, #47866, .T. ) ;
#28078 = B_SPLINE_CURVE_WITH_KNOTS ( 'NONE', 3,
 ( #27317, #42948, #23475, #39136, #3958, #19606 ),
 .UNSPECIFIED., .F., .F.,
 ( 4, 2, 4 ),
 ( 5.818439421673296370E-18, 0.009877169331704826680, 0.01975433866340964989 ),
 .UNSPECIFIED. ) ;
#28079 = ORIENTED_EDGE ( 'NONE', *, *, #4243, .T. ) ;
#28080 = ADVANCED_FACE ( 'NONE', ( #15780 ), #10917, .F. ) ;
#28081 = EDGE_CURVE ( 'NONE', #17600, #15132, #11681, .T. ) ;
#28082 = DIRECTION ( 'NONE',  ( 0.000000000000000000, 0.000000000000000000, -1.000000000000000000 ) ) ;
#28083 = CARTESIAN_POINT ( 'NONE',  ( -124.9459734468149321, 1.025126265847082108, 122.5682875569279702 ) ) ;
#28084 = CARTESIAN_POINT ( 'NONE',  ( -166.6959734468149463, 1.750000000000009992, -159.1817124430720298 ) ) ;
#28085 = ADVANCED_FACE ( 'NONE', ( #7081 ), #42462, .T. ) ;
#28086 = CARTESIAN_POINT ( 'NONE',  ( 37.50000000000000000, 4.592425496802574367E-15, -10.00000000000000000 ) ) ;
#28087 = AXIS2_PLACEMENT_3D ( 'NONE', #5183, #1097, #16735 ) ;
#28088 = EDGE_CURVE ( 'NONE', #17655, #4851, #38644, .T. ) ;
#28089 = ORIENTED_EDGE ( 'NONE', *, *, #41944, .T. ) ;
#28090 = ORIENTED_EDGE ( 'NONE', *, *, #9502, .F. ) ;
#28091 = DIRECTION ( 'NONE',  ( 1.000000000000000000, 0.000000000000000000, 0.000000000000000000 ) ) ;
#28092 = CARTESIAN_POINT ( 'NONE',  ( 155.0540265531850537, -1.025126265847089213, -0.9317124430720324924 ) ) ;
#28093 = ORIENTED_EDGE ( 'NONE', *, *, #37265, .F. ) ;
#28094 = ORIENTED_EDGE ( 'NONE', *, *, #11496, .F. ) ;
#28095 = LINE ( 'NONE', #4489, #32142 ) ;
#28096 = CARTESIAN_POINT ( 'NONE',  ( -205.6708471809678827, -1.750000000000010436, 79.79316129108087807 ) ) ;
#28097 = CARTESIAN_POINT ( 'NONE',  ( -8.445973446814976526, 0.000000000000000000, -80.93171244307204404 ) ) ;
#28098 = CARTESIAN_POINT ( 'NONE',  ( -164.9999999999981526, 17.00000000000000000, 90.00000000000000000 ) ) ;
#28099 = AXIS2_PLACEMENT_3D ( 'NONE', #3892, #4154, #4663 ) ;
#28100 = VERTEX_POINT ( 'NONE', #27604 ) ;
#28101 = ORIENTED_EDGE ( 'NONE', *, *, #50627, .T. ) ;
#28102 = CIRCLE ( 'NONE', #9271, 4.000000000000003553 ) ;
#28103 = ORIENTED_EDGE ( 'NONE', *, *, #12222, .T. ) ;
#28104 = VECTOR ( 'NONE', #4029, 1000.000000000000000 ) ;
#28105 = CARTESIAN_POINT ( 'NONE',  ( -6.880036658038818587, -197.4999999999999432, -228.6347188485896140 ) ) ;
#28106 = ORIENTED_EDGE ( 'NONE', *, *, #11507, .F. ) ;
#28107 = EDGE_CURVE ( 'NONE', #5706, #41541, #6820, .T. ) ;
#28108 = AXIS2_PLACEMENT_3D ( 'NONE', #49181, #18423, #37698 ) ;
#28109 = CARTESIAN_POINT ( 'NONE',  ( -6.695973446814940111, 0.000000000000000000, 165.0000000000000000 ) ) ;
#28110 = EDGE_LOOP ( 'NONE', ( #46233, #15938, #20911, #26285 ) ) ;
#28111 = ORIENTED_EDGE ( 'NONE', *, *, #29030, .F. ) ;
#28112 = DIRECTION ( 'NONE',  ( -0.000000000000000000, -0.000000000000000000, -1.000000000000000000 ) ) ;
#28113 = CARTESIAN_POINT ( 'NONE',  ( 113.3040265531850537, 1.749999999999997113, -39.18171244307202983 ) ) ;
#28114 = CARTESIAN_POINT ( 'NONE',  ( -0.3862712429686977478, 1.188820645368937390, 10.00000000000000000 ) ) ;
#28115 = EDGE_LOOP ( 'NONE', ( #44609, #43207, #27710, #40792 ) ) ;
#28116 = ORIENTED_EDGE ( 'NONE', *, *, #33245, .T. ) ;
#28117 = DIRECTION ( 'NONE',  ( 0.000000000000000000, 1.000000000000000000, -0.000000000000000000 ) ) ;
#28118 = LINE ( 'NONE', #31469, #2661 ) ;
#28119 = ORIENTED_EDGE ( 'NONE', *, *, #30306, .F. ) ;
#28120 =( BOUNDED_CURVE ( )  B_SPLINE_CURVE ( 3, ( #3274, #18919, #35122, #50176 ),
 .UNSPECIFIED., .F., .F. ) 
 B_SPLINE_CURVE_WITH_KNOTS ( ( 4, 4 ),
 ( 4.712388980384689674, 6.283185307179586232 ),
 .UNSPECIFIED. ) 
 CURVE ( )  GEOMETRIC_REPRESENTATION_ITEM ( )  RATIONAL_B_SPLINE_CURVE ( ( 1.000000000000000000, 0.8047378541243649375, 0.8047378541243649375, 1.000000000000000000 ) ) 
 REPRESENTATION_ITEM ( '' )  );
#28121 = DIRECTION ( 'NONE',  ( -1.000000000000000000, -0.000000000000000000, -0.000000000000000000 ) ) ;
#28122 = CARTESIAN_POINT ( 'NONE',  ( -84.94597344681494633, 2.143131898507880377E-16, -160.9317124430720014 ) ) ;
#28123 = CARTESIAN_POINT ( 'NONE',  ( 168.9999999999999716, -272.4999999999999432, -341.9999999999999432 ) ) ;
#28124 = CARTESIAN_POINT ( 'NONE',  ( -168.4459734468149463, 0.000000000000000000, 82.56828755692798438 ) ) ;
#28125 = ORIENTED_EDGE ( 'NONE', *, *, #36709, .T. ) ;
#28126 = EDGE_CURVE ( 'NONE', #1207, #18285, #11189, .T. ) ;
#28127 = FACE_OUTER_BOUND ( 'NONE', #6479, .T. ) ;
#28128 =( BOUNDED_CURVE ( )  B_SPLINE_CURVE ( 3, ( #9394, #37380, #17342, #48090 ),
 .UNSPECIFIED., .F., .F. ) 
 B_SPLINE_CURVE_WITH_KNOTS ( ( 4, 4 ),
 ( 3.141592653589793116, 4.712388980384689674 ),
 .UNSPECIFIED. ) 
 CURVE ( )  GEOMETRIC_REPRESENTATION_ITEM ( )  RATIONAL_B_SPLINE_CURVE ( ( 1.000000000000000000, 0.8047378541243649375, 0.8047378541243649375, 1.000000000000000000 ) ) 
 REPRESENTATION_ITEM ( '' )  );
#28129 = DIRECTION ( 'NONE',  ( 0.000000000000000000, 0.000000000000000000, 1.000000000000000000 ) ) ;
#28130 = DIRECTION ( 'NONE',  ( -1.000000000000000000, 0.000000000000000000, -3.469446951953611724E-16 ) ) ;
#28131 = DIRECTION ( 'NONE',  ( -0.000000000000000000, -0.000000000000000000, -1.000000000000000000 ) ) ;
#28132 = VECTOR ( 'NONE', #44830, 1000.000000000000000 ) ;
#28133 = EDGE_CURVE ( 'NONE', #32484, #6330, #19631, .T. ) ;
#28134 = CARTESIAN_POINT ( 'NONE',  ( 10.01251772323701772, 8.486842105263161073, 18.46084505325461578 ) ) ;
#28135 = AXIS2_PLACEMENT_3D ( 'NONE', #34307, #7109, #29952 ) ;
#28136 =( BOUNDED_CURVE ( )  B_SPLINE_CURVE ( 3, ( #27693, #35414, #15390, #18961 ),
 .UNSPECIFIED., .F., .F. ) 
 B_SPLINE_CURVE_WITH_KNOTS ( ( 4, 4 ),
 ( 4.712388980384689674, 6.283185307179586232 ),
 .UNSPECIFIED. ) 
 CURVE ( )  GEOMETRIC_REPRESENTATION_ITEM ( )  RATIONAL_B_SPLINE_CURVE ( ( 1.000000000000000000, 0.8047378541243649375, 0.8047378541243649375, 1.000000000000000000 ) ) 
 REPRESENTATION_ITEM ( '' )  );
#28137 = CARTESIAN_POINT ( 'NONE',  ( 0.5705203167769784534, 1.169354363542900010, 9.986087673579197244 ) ) ;
#28138 = AXIS2_PLACEMENT_3D ( 'NONE', #23084, #3072, #18715 ) ;
#28139 = EDGE_LOOP ( 'NONE', ( #23233, #1578, #43050, #19332 ) ) ;
#28140 = PLANE ( 'NONE',  #47724 ) ;
#28141 = EDGE_CURVE ( 'NONE', #23383, #3985, #42710, .T. ) ;
#28142 = EDGE_CURVE ( 'NONE', #30870, #42453, #42353, .T. ) ;
#28143 = AXIS2_PLACEMENT_3D ( 'NONE', #28259, #12103, #8008 ) ;
#28144 = CARTESIAN_POINT ( 'NONE',  ( 85.00000000000056843, 17.00000000000000000, -54.99999999999999289 ) ) ;
#28145 = ORIENTED_EDGE ( 'NONE', *, *, #14065, .T. ) ;
#28146 = DIRECTION ( 'NONE',  ( -0.1671032855531282835, -0.5142910309547751302, -0.8411784753765542133 ) ) ;
#28147 = CARTESIAN_POINT ( 'NONE',  ( 34.38425513258721367, -36.82177522737821107, 8.807470649214879543 ) ) ;
#28148 = FACE_OUTER_BOUND ( 'NONE', #27704, .T. ) ;
#28149 = EDGE_CURVE ( 'NONE', #43794, #16197, #2343, .T. ) ;
#28150 = ORIENTED_EDGE ( 'NONE', *, *, #29289, .T. ) ;
#28151 = CARTESIAN_POINT ( 'NONE',  ( 0.8784099037133200616, 0.8517617868932368941, 9.993783931180534097 ) ) ;
#28152 = B_SPLINE_SURFACE_WITH_KNOTS ( 'NONE', 3, 3, ( 
 ( #34771, #31164, #23461, #46754 ),
 ( #43452, #19347, #11654, #22938 ),
 ( #20105, #47012, #27308, #42938 ),
 ( #27570, #39621, #23711, #15748 ) ),
 .UNSPECIFIED., .F., .F., .F.,
 ( 4, 4 ),
 ( 4, 4 ),
 ( 0.000000000000000000, 1.000000000000000000 ),
 ( 0.000000000000000000, 1.000000000000000000 ),
 .UNSPECIFIED. ) ;
#28153 = VERTEX_POINT ( 'NONE', #24504 ) ;
#28154 = ORIENTED_EDGE ( 'NONE', *, *, #11881, .T. ) ;
#28155 = CARTESIAN_POINT ( 'NONE',  ( -7.721099712662037540, 1.750000000000022427, -158.1565861772249093 ) ) ;
#28156 = EDGE_CURVE ( 'NONE', #34169, #31607, #32206, .T. ) ;
#28157 = CARTESIAN_POINT ( 'NONE',  ( 129.9999999999999432, 16.00000000000000000, -114.9999999999999858 ) ) ;
#28158 = EDGE_CURVE ( 'NONE', #3658, #16118, #31715, .T. ) ;
#28159 = VECTOR ( 'NONE', #27868, 1000.000000000000114 ) ;
#28160 = ORIENTED_EDGE ( 'NONE', *, *, #45591, .F. ) ;
#28161 = CARTESIAN_POINT ( 'NONE',  ( -34.38425513258695077, 36.82177522737848108, 8.807470649214879543 ) ) ;
#28162 = CARTESIAN_POINT ( 'NONE',  ( -7.721099712662037540, -1.750000000000022871, 161.8434138227750907 ) ) ;
#28163 = VERTEX_POINT ( 'NONE', #20898 ) ;
#28164 = EDGE_CURVE ( 'NONE', #31704, #40007, #35492, .T. ) ;
#28165 = LINE ( 'NONE', #8670, #48043 ) ;
#28166 = ORIENTED_EDGE ( 'NONE', *, *, #33972, .T. ) ;
#28167 = B_SPLINE_CURVE_WITH_KNOTS ( 'NONE', 3,
 ( #34928, #12069, #19, #20266 ),
 .UNSPECIFIED., .F., .F.,
 ( 4, 4 ),
 ( 0.7491799374948681089, 1.000000000000000000 ),
 .UNSPECIFIED. ) ;
#28168 = DIRECTION ( 'NONE',  ( 0.000000000000000000, -1.000000000000000000, 0.000000000000000000 ) ) ;
#28169 = CARTESIAN_POINT ( 'NONE',  ( -164.9459734468149747, 0.000000000000000000, 162.5682875569279702 ) ) ;
#28170 = DIRECTION ( 'NONE',  ( -1.000000000000000000, -0.000000000000000000, -0.000000000000000000 ) ) ;
#28171 = ORIENTED_EDGE ( 'NONE', *, *, #30537, .F. ) ;
#28172 = DIRECTION ( 'NONE',  ( 0.000000000000000000, 1.000000000000000000, 3.186989995019654210E-49 ) ) ;
#28173 = DIRECTION ( 'NONE',  ( 0.000000000000000000, 0.9749645535258950613, -0.2223603367690656918 ) ) ;
#28174 = AXIS2_PLACEMENT_3D ( 'NONE', #41837, #22588, #34166 ) ;
#28175 = VERTEX_POINT ( 'NONE', #8098 ) ;
#28176 = ORIENTED_EDGE ( 'NONE', *, *, #47845, .F. ) ;
#28177 = VERTEX_POINT ( 'NONE', #28097 ) ;
#28178 = DIRECTION ( 'NONE',  ( 0.000000000000000000, 0.000000000000000000, -1.000000000000000000 ) ) ;
#28179 = AXIS2_PLACEMENT_3D ( 'NONE', #503, #16637, #27433 ) ;
#28180 = CARTESIAN_POINT ( 'NONE',  ( -5.000000000000000000, -175.0000000000000284, -350.0000000000002274 ) ) ;
#28181 = VERTEX_POINT ( 'NONE', #23998 ) ;
#28182 = AXIS2_PLACEMENT_3D ( 'NONE', #48162, #37442, #1768 ) ;
#28183 = PLANE ( 'NONE',  #36469 ) ;
#28184 = CARTESIAN_POINT ( 'NONE',  ( 194.3291528190321742, 1.750000000000010214, -80.20683870891910772 ) ) ;
#28185 = CIRCLE ( 'NONE', #41275, 1.750000000000008438 ) ;
#28186 = DIRECTION ( 'NONE',  ( 0.000000000000000000, 0.000000000000000000, 1.000000000000000000 ) ) ;
#28187 = CARTESIAN_POINT ( 'NONE',  ( 357.9999999999998863, -182.1715728752538155, 357.1715728752536734 ) ) ;
#28188 = CARTESIAN_POINT ( 'NONE',  ( -88.44597344681497475, 0.000000000000000000, 159.0682875569279418 ) ) ;
#28189 = LINE ( 'NONE', #46622, #20014 ) ;
#28190 = CARTESIAN_POINT ( 'NONE',  ( 73.30402655318508209, 0.000000000000000000, 165.0000000000000000 ) ) ;
#28191 = CARTESIAN_POINT ( 'NONE',  ( 169.0000000000000000, -174.9999999999999716, -99.00000000000014211 ) ) ;
#28192 = CARTESIAN_POINT ( 'NONE',  ( 0.3862712429686978033, -1.188820645368937834, 10.00000000000000000 ) ) ;
#28193 = EDGE_CURVE ( 'NONE', #37343, #6842, #18080, .T. ) ;
#28194 = DIRECTION ( 'NONE',  ( -1.000000000000000000, 0.000000000000000000, 0.000000000000000000 ) ) ;
#28195 = VECTOR ( 'NONE', #6850, 1000.000000000000000 ) ;
#28196 = DIRECTION ( 'NONE',  ( 0.000000000000000000, 0.000000000000000000, -1.000000000000000000 ) ) ;
#28197 = ORIENTED_EDGE ( 'NONE', *, *, #9544, .F. ) ;
#28198 = CARTESIAN_POINT ( 'NONE',  ( -119.9999999999994174, 16.00000000000000000, -54.99999999999999289 ) ) ;
#28199 = LINE ( 'NONE', #32309, #1560 ) ;
#28200 = DIRECTION ( 'NONE',  ( -2.958228394578793832E-31, 0.000000000000000000, -1.000000000000000000 ) ) ;
#28201 = CARTESIAN_POINT ( 'NONE',  ( 210.0000000000000568, 2.143131898507881116E-16, -40.93171244307203693 ) ) ;
#28202 = VERTEX_POINT ( 'NONE', #20386 ) ;
#28203 = CARTESIAN_POINT ( 'NONE',  ( 210.0000000000000568, 0.000000000000000000, -79.18171244307201562 ) ) ;
#28204 = EDGE_CURVE ( 'NONE', #12891, #26731, #24763, .T. ) ;
#28205 = EDGE_CURVE ( 'NONE', #49797, #47427, #38780, .T. ) ;
#28206 = VECTOR ( 'NONE', #13806, 1000.000000000000000 ) ;
#28207 = CYLINDRICAL_SURFACE ( 'NONE', #41754, 2.000000000000001776 ) ;
#28208 = VECTOR ( 'NONE', #37394, 1000.000000000000000 ) ;
#28209 = VERTEX_POINT ( 'NONE', #27851 ) ;
#28210 = CARTESIAN_POINT ( 'NONE',  ( 30.87089393895375267, -12.69923079256617449, -9.367992836599954742 ) ) ;
#28211 = AXIS2_PLACEMENT_3D ( 'NONE', #21836, #13853, #9272 ) ;
#28212 = DIRECTION ( 'NONE',  ( 0.000000000000000000, 0.000000000000000000, 1.000000000000000000 ) ) ;
#28213 = CARTESIAN_POINT ( 'NONE',  ( -46.69597344681494633, 1.750000000000009992, 0.8182875569279768335 ) ) ;
#28214 = VERTEX_POINT ( 'NONE', #4992 ) ;
#28215 = CARTESIAN_POINT ( 'NONE',  ( 85.00000000000123634, 16.00000000000000000, 5.000000000000004441 ) ) ;
#28216 = ORIENTED_EDGE ( 'NONE', *, *, #45706, .F. ) ;
#28217 = ORIENTED_EDGE ( 'NONE', *, *, #23613, .T. ) ;
#28218 = VECTOR ( 'NONE', #48439, 1000.000000000000000 ) ;
#28219 = ADVANCED_FACE ( 'NONE', ( #32706 ), #401, .T. ) ;
#28220 = EDGE_CURVE ( 'NONE', #45172, #22827, #16802, .T. ) ;
#28221 = EDGE_LOOP ( 'NONE', ( #36827, #44500, #26897, #28911 ) ) ;
#28222 = DIRECTION ( 'NONE',  ( 0.000000000000000000, 0.000000000000000000, 1.000000000000000000 ) ) ;
#28223 = CARTESIAN_POINT ( 'NONE',  ( -4.945973446814938335, 0.000000000000000000, 162.5682875569279702 ) ) ;
#28224 = ORIENTED_EDGE ( 'NONE', *, *, #27738, .F. ) ;
#28225 = CARTESIAN_POINT ( 'NONE',  ( 0.000000000000000000, -250.0000000000000000, -224.9999999999999716 ) ) ;
#28226 = ADVANCED_FACE ( 'NONE', ( #36584 ), #4379, .T. ) ;
#28227 = PLANE ( 'NONE',  #38879 ) ;
#28228 = CARTESIAN_POINT ( 'NONE',  ( 10.00000000000000000, 1.224646799147353256E-15, 10.00000000000000000 ) ) ;
#28229 = VERTEX_POINT ( 'NONE', #12691 ) ;
#28230 = LINE ( 'NONE', #3599, #47650 ) ;
#28231 = CIRCLE ( 'NONE', #396, 4.250000000000000000 ) ;
#28232 = ORIENTED_EDGE ( 'NONE', *, *, #42774, .T. ) ;
#28233 = DIRECTION ( 'NONE',  ( -1.000000000000000000, 0.000000000000000000, -0.000000000000000000 ) ) ;
#28234 = DIRECTION ( 'NONE',  ( 1.000000000000000000, -0.000000000000000000, -0.000000000000000000 ) ) ;
#28235 = VECTOR ( 'NONE', #18698, 1000.000000000000000 ) ;
#28236 = ORIENTED_EDGE ( 'NONE', *, *, #30104, .T. ) ;
#28237 = LINE ( 'NONE', #24394, #20444 ) ;
#28238 = B_SPLINE_CURVE_WITH_KNOTS ( 'NONE', 3,
 ( #14743, #7051, #2439, #22691 ),
 .UNSPECIFIED., .F., .F.,
 ( 4, 4 ),
 ( 0.0006669682284780878911, 0.0007799402130920262462 ),
 .UNSPECIFIED. ) ;
#28239 = CARTESIAN_POINT ( 'NONE',  ( 26.25702031264353664, -26.77347351953840615, 8.914903342594564961 ) ) ;
#28240 = ORIENTED_EDGE ( 'NONE', *, *, #15775, .T. ) ;
#28241 = FACE_OUTER_BOUND ( 'NONE', #39730, .T. ) ;
#28242 = CARTESIAN_POINT ( 'NONE',  ( 224.9999999999999716, -164.9999999999999716, 474.9999999999998863 ) ) ;
#28243 = DIRECTION ( 'NONE',  ( -1.000000000000000000, 0.000000000000000000, -0.000000000000000000 ) ) ;
#28244 = DIRECTION ( 'NONE',  ( 0.000000000000000000, 0.000000000000000000, 1.000000000000000000 ) ) ;
#28245 = ORIENTED_EDGE ( 'NONE', *, *, #44390, .F. ) ;
#28246 = CIRCLE ( 'NONE', #6105, 10.00000000000000000 ) ;
#28247 = DIRECTION ( 'NONE',  ( -0.000000000000000000, -0.000000000000000000, -1.000000000000000000 ) ) ;
#28248 = DIRECTION ( 'NONE',  ( -1.000000000000000000, 1.586032892321652236E-16, 1.586032892321651989E-16 ) ) ;
#28249 = CARTESIAN_POINT ( 'NONE',  ( 0.000000000000000000, 17.00000000000000000, 0.000000000000000000 ) ) ;
#28250 = ORIENTED_EDGE ( 'NONE', *, *, #28393, .T. ) ;
#28251 = VECTOR ( 'NONE', #31733, 1000.000000000000000 ) ;
#28252 = EDGE_CURVE ( 'NONE', #15011, #34763, #12935, .T. ) ;
#28253 = ORIENTED_EDGE ( 'NONE', *, *, #13029, .F. ) ;
#28254 = SHAPE_DEFINITION_REPRESENTATION ( #23300, #15926 ) ;
#28255 = CARTESIAN_POINT ( 'NONE',  ( 210.0000000000000568, 2.143131898507881856E-16, -80.93171244307202983 ) ) ;
#28256 = CARTESIAN_POINT ( 'NONE',  ( -5.000000000000000000, -175.0000000000000284, 350.0000000000002274 ) ) ;
#28257 = CARTESIAN_POINT ( 'NONE',  ( 40.00000000000000000, 4.898587196589413026E-15, 897.6604670114603550 ) ) ;
#28258 = DIRECTION ( 'NONE',  ( 0.000000000000000000, 0.000000000000000000, -1.000000000000000000 ) ) ;
#28259 = CARTESIAN_POINT ( 'NONE',  ( 181.0000000000000000, -268.5000000000000000, -114.9999999999999147 ) ) ;
#28260 = ORIENTED_EDGE ( 'NONE', *, *, #5449, .T. ) ;
#28261 = LINE ( 'NONE', #39564, #32960 ) ;
#28262 = DIRECTION ( 'NONE',  ( 1.000000000000000000, -0.000000000000000000, -0.000000000000000000 ) ) ;
#28263 = DIRECTION ( 'NONE',  ( -0.000000000000000000, -1.000000000000000000, 2.537652627714643577E-15 ) ) ;
#28264 = CARTESIAN_POINT ( 'NONE',  ( -44.94597344681493922, 2.143131898507880377E-16, 79.06828755692797017 ) ) ;
#28265 = ORIENTED_EDGE ( 'NONE', *, *, #3045, .T. ) ;
#28266 = VECTOR ( 'NONE', #7130, 1000.000000000000000 ) ;
#28267 = EDGE_LOOP ( 'NONE', ( #8002, #7148, #1730, #463 ) ) ;
#28268 = DIRECTION ( 'NONE',  ( 1.000000000000000000, 0.000000000000000000, 0.000000000000000000 ) ) ;
#28269 = VECTOR ( 'NONE', #9755, 1000.000000000000000 ) ;
#28270 = ORIENTED_EDGE ( 'NONE', *, *, #27801, .F. ) ;
#28271 = CARTESIAN_POINT ( 'NONE',  ( -205.6708471809678827, 1.750000000000009548, 159.7931612910809065 ) ) ;
#28272 = CARTESIAN_POINT ( 'NONE',  ( 8.831420117243668599, 14.12636088103192655, -3.546734833711462365 ) ) ;
#28273 = DIRECTION ( 'NONE',  ( 0.7233555441435721711, 0.6904757466825005574, -0.000000000000000000 ) ) ;
#28274 = LINE ( 'NONE', #36493, #15692 ) ;
#28275 = ORIENTED_EDGE ( 'NONE', *, *, #1607, .F. ) ;
#28276 = DIRECTION ( 'NONE',  ( -0.000000000000000000, -0.000000000000000000, -1.000000000000000000 ) ) ;
#28277 = VERTEX_POINT ( 'NONE', #25763 ) ;
#28278 = VECTOR ( 'NONE', #28833, 1000.000000000000000 ) ;
#28279 = DIRECTION ( 'NONE',  ( -0.000000000000000000, -0.000000000000000000, -1.000000000000000000 ) ) ;
#28280 = CARTESIAN_POINT ( 'NONE',  ( -0.3862712429686729343, -1.188820645368946050, 10.00000000000000000 ) ) ;
#28281 = CARTESIAN_POINT ( 'NONE',  ( 210.0000000000000568, 0.000000000000000000, 80.81828755692798438 ) ) ;
#28282 = ADVANCED_FACE ( 'NONE', ( #37833 ), #26019, .F. ) ;
#28283 =( BOUNDED_CURVE ( )  B_SPLINE_CURVE ( 3, ( #29, #28484, #12827, #31840 ),
 .UNSPECIFIED., .F., .F. ) 
 B_SPLINE_CURVE_WITH_KNOTS ( ( 4, 4 ),
 ( 3.141592653589793116, 4.712388980384689674 ),
 .UNSPECIFIED. ) 
 CURVE ( )  GEOMETRIC_REPRESENTATION_ITEM ( )  RATIONAL_B_SPLINE_CURVE ( ( 1.000000000000000000, 0.8047378541243649375, 0.8047378541243649375, 1.000000000000000000 ) ) 
 REPRESENTATION_ITEM ( '' )  );
#28284 = ORIENTED_EDGE ( 'NONE', *, *, #46065, .T. ) ;
#28285 = ORIENTED_EDGE ( 'NONE', *, *, #34749, .F. ) ;
#28286 = CARTESIAN_POINT ( 'NONE',  ( -5.000000000000000000, 184.8000000000000114, 359.7999999999997840 ) ) ;
#28287 = VECTOR ( 'NONE', #50719, 1000.000000000000000 ) ;
#28288 = ORIENTED_EDGE ( 'NONE', *, *, #35058, .F. ) ;
#28289 = CARTESIAN_POINT ( 'NONE',  ( 168.9999999999999716, -168.9999999999999432, -350.0000000000001705 ) ) ;
#28290 = LINE ( 'NONE', #35765, #44756 ) ;
#28291 = LINE ( 'NONE', #20334, #39565 ) ;
#28292 = ORIENTED_EDGE ( 'NONE', *, *, #50341, .T. ) ;
#28293 = DIRECTION ( 'NONE',  ( 1.000000000000000000, 0.000000000000000000, 0.000000000000000000 ) ) ;
#28294 = FACE_OUTER_BOUND ( 'NONE', #50219, .T. ) ;
#28295 = LINE ( 'NONE', #4442, #16533 ) ;
#28296 = VECTOR ( 'NONE', #23732, 1000.000000000000000 ) ;
#28297 = ORIENTED_EDGE ( 'NONE', *, *, #34413, .T. ) ;
#28298 = ORIENTED_EDGE ( 'NONE', *, *, #7839, .F. ) ;
#28299 = ORIENTED_EDGE ( 'NONE', *, *, #50101, .F. ) ;
#28300 = VECTOR ( 'NONE', #39948, 1000.000000000000000 ) ;
#28301 = CARTESIAN_POINT ( 'NONE',  ( -0.1425549192113998442, 1.238581250503548059, 9.981352469109934233 ) ) ;
#28302 = CARTESIAN_POINT ( 'NONE',  ( -14.99999999999782041, 17.00000000000000000, 95.00000000000000000 ) ) ;
#28303 = CARTESIAN_POINT ( 'NONE',  ( -5.505322767148756569, 37.09368438467003415, 8.914903342594564961 ) ) ;
#28304 = VECTOR ( 'NONE', #5213, 1000.000000000000000 ) ;
#28305 = ORIENTED_EDGE ( 'NONE', *, *, #21121, .T. ) ;
#28306 = CARTESIAN_POINT ( 'NONE',  ( 210.0000000000000568, 0.000000000000000000, 120.8182875569279702 ) ) ;
#28307 = ORIENTED_EDGE ( 'NONE', *, *, #38137, .F. ) ;
#28308 = CARTESIAN_POINT ( 'NONE',  ( 135.0000000000015632, 17.00000000000000000, 35.00000000000000000 ) ) ;
#28309 = VERTEX_POINT ( 'NONE', #29108 ) ;
#28310 = CARTESIAN_POINT ( 'NONE',  ( -6.174150299305392053, 50.00000000000000711, 8.807470649214879543 ) ) ;
#28311 = AXIS2_PLACEMENT_3D ( 'NONE', #6978, #26981, #31356 ) ;
#28312 = FACE_BOUND ( 'NONE', #11506, .T. ) ;
#28313 = PLANE ( 'NONE',  #42251 ) ;
#28314 = CARTESIAN_POINT ( 'NONE',  ( 79.99999999999997158, 17.00000000000000000, -90.00000000000000000 ) ) ;
#28315 = CARTESIAN_POINT ( 'NONE',  ( 35.05402655318504657, 2.143131898507880377E-16, -160.9317124430720582 ) ) ;
#28316 = VECTOR ( 'NONE', #4323, 1000.000000000000000 ) ;
#28317 = FACE_OUTER_BOUND ( 'NONE', #40421, .T. ) ;
#28318 = ORIENTED_EDGE ( 'NONE', *, *, #34611, .F. ) ;
#28319 = LINE ( 'NONE', #47530, #35421 ) ;
#28320 = EDGE_CURVE ( 'NONE', #30554, #13154, #34764, .T. ) ;
#28321 = DIRECTION ( 'NONE',  ( -1.000000000000000000, 0.000000000000000000, 0.000000000000000000 ) ) ;
#28322 = CARTESIAN_POINT ( 'NONE',  ( -7.200076171898729172, 4.082484168683569496E-15, -33.33601305720110020 ) ) ;
#28323 = VECTOR ( 'NONE', #30778, 1000.000000000000000 ) ;
#28324 = DIRECTION ( 'NONE',  ( 0.1346615698592613930, 0.000000000000000000, -0.9908916497796513845 ) ) ;
#28325 = ORIENTED_EDGE ( 'NONE', *, *, #28927, .F. ) ;
#28326 = DIRECTION ( 'NONE',  ( 0.000000000000000000, 0.000000000000000000, -1.000000000000000000 ) ) ;
#28327 = EDGE_LOOP ( 'NONE', ( #40102, #8022, #43622, #1466, #46479 ) ) ;
#28328 = DIRECTION ( 'NONE',  ( -1.000000000000000000, -0.000000000000000000, 4.625929269271687073E-16 ) ) ;
#28329 = CARTESIAN_POINT ( 'NONE',  ( 1.540662627795932105, -1.371465786296032441, 9.894754715216729224 ) ) ;
#28330 = EDGE_LOOP ( 'NONE', ( #50155, #29058, #15329, #2975 ) ) ;
#28331 = VECTOR ( 'NONE', #18840, 1000.000000000000114 ) ;
#28332 = EDGE_CURVE ( 'NONE', #375, #19127, #2404, .T. ) ;
#28333 = CARTESIAN_POINT ( 'NONE',  ( -128.4459734468149463, 1.025126265847081664, -37.43171244307203693 ) ) ;
#28334 = CARTESIAN_POINT ( 'NONE',  ( -8.445973446814976526, 0.000000000000000000, 159.0682875569279418 ) ) ;
#28335 = AXIS2_PLACEMENT_3D ( 'NONE', #2410, #6279, #1423 ) ;
#28336 = CARTESIAN_POINT ( 'NONE',  ( 164.9999999999999716, -268.5000000000002842, -114.9999999999999147 ) ) ;
#28337 = CARTESIAN_POINT ( 'NONE',  ( 33.43156050989131955, -4.370686678976570150, 8.807470649214879543 ) ) ;
#28338 = EDGE_CURVE ( 'NONE', #33571, #49500, #17805, .T. ) ;
#28339 = AXIS2_PLACEMENT_3D ( 'NONE', #16526, #12412, #20112 ) ;
#28340 = EDGE_LOOP ( 'NONE', ( #10495, #26340 ) ) ;
#28341 = ORIENTED_EDGE ( 'NONE', *, *, #15123, .F. ) ;
#28342 = FACE_OUTER_BOUND ( 'NONE', #36074, .T. ) ;
#28343 = ADVANCED_FACE ( 'NONE', ( #9354 ), #14189, .T. ) ;
#28344 = CARTESIAN_POINT ( 'NONE',  ( 32.36066692128250821, -7.813306791042813337, 3.199614146704519602 ) ) ;
#28345 = EDGE_CURVE ( 'NONE', #40611, #24906, #47568, .T. ) ;
#28346 = AXIS2_PLACEMENT_3D ( 'NONE', #33347, #30491, #21782 ) ;
#28347 = ORIENTED_EDGE ( 'NONE', *, *, #41707, .F. ) ;
#28348 = B_SPLINE_CURVE_WITH_KNOTS ( 'NONE', 3,
 ( #15749, #8322, #31420, #1130 ),
 .UNSPECIFIED., .F., .F.,
 ( 4, 4 ),
 ( 0.000000000000000000, 0.002458791966311101550 ),
 .UNSPECIFIED. ) ;
#28349 = VERTEX_POINT ( 'NONE', #37340 ) ;
#28350 = CARTESIAN_POINT ( 'NONE',  ( 14.29087950072012170, 9.652079258044652832, 8.727788335465566760 ) ) ;
#28351 = CARTESIAN_POINT ( 'NONE',  ( 73.30402655318508209, 1.750000000000010658, 80.81828755692798438 ) ) ;
#28352 = CARTESIAN_POINT ( 'NONE',  ( 29.61572577327002520, 16.11461842845735859, 8.807470649214879543 ) ) ;
#28353 = CARTESIAN_POINT ( 'NONE',  ( 166.9999999999999716, -184.9999999999999716, -344.0000000000001137 ) ) ;
#28354 = AXIS2_PLACEMENT_3D ( 'NONE', #32929, #21099, #33430 ) ;
#28355 = ORIENTED_EDGE ( 'NONE', *, *, #20906, .T. ) ;
#28356 = VERTEX_POINT ( 'NONE', #18048 ) ;
#28357 = VERTEX_POINT ( 'NONE', #6271 ) ;
#28358 = AXIS2_PLACEMENT_3D ( 'NONE', #44579, #9462, #25127 ) ;
#28359 = VECTOR ( 'NONE', #17850, 1000.000000000000000 ) ;
#28360 = DIRECTION ( 'NONE',  ( -1.586032880504786307E-16, 1.654361225106055350E-24, -1.000000000000000000 ) ) ;
#28361 = CARTESIAN_POINT ( 'NONE',  ( 0.000000000000000000, 33.89193117067290473, 910.0000000000000000 ) ) ;
#28362 = EDGE_LOOP ( 'NONE', ( #15296, #1977, #28021, #14063, #39887, #10919 ) ) ;
#28363 =( BOUNDED_CURVE ( )  B_SPLINE_CURVE ( 3, ( #40707, #36883, #8889, #24546 ),
 .UNSPECIFIED., .F., .F. ) 
 B_SPLINE_CURVE_WITH_KNOTS ( ( 4, 4 ),
 ( 4.712388980384689674, 6.283185307179586232 ),
 .UNSPECIFIED. ) 
 CURVE ( )  GEOMETRIC_REPRESENTATION_ITEM ( )  RATIONAL_B_SPLINE_CURVE ( ( 1.000000000000000000, 0.8047378541243649375, 0.8047378541243649375, 1.000000000000000000 ) ) 
 REPRESENTATION_ITEM ( '' )  );
#28364 = EDGE_LOOP ( 'NONE', ( #37945, #46989 ) ) ;
#28365 = CARTESIAN_POINT ( 'NONE',  ( -1.142975459103954705, -16.61830776097024653, -2.870787844569587133 ) ) ;
#28366 = DIRECTION ( 'NONE',  ( -1.000000000000000000, -0.000000000000000000, -0.000000000000000000 ) ) ;
#28367 = ORIENTED_EDGE ( 'NONE', *, *, #5895, .T. ) ;
#28368 = ADVANCED_FACE ( 'NONE', ( #44475 ), #21651, .F. ) ;
#28369 = EDGE_CURVE ( 'NONE', #11925, #19313, #14953, .T. ) ;
#28370 = ORIENTED_EDGE ( 'NONE', *, *, #11567, .F. ) ;
#28371 = CARTESIAN_POINT ( 'NONE',  ( 0.000000000000000000, 249.9999999999999716, 225.0000000000000000 ) ) ;
#28372 = CARTESIAN_POINT ( 'NONE',  ( 167.0000000000000000, 2.775557561562891351E-14, -99.00000000000014211 ) ) ;
#28373 = VERTEX_POINT ( 'NONE', #33228 ) ;
#28374 = EDGE_CURVE ( 'NONE', #7223, #22379, #31597, .T. ) ;
#28375 = CIRCLE ( 'NONE', #44711, 1.749999999999987566 ) ;
#28376 = DIRECTION ( 'NONE',  ( 1.000000000000000000, 0.000000000000000000, -0.000000000000000000 ) ) ;
#28377 = CARTESIAN_POINT ( 'NONE',  ( -86.69597344681496054, 0.000000000000000000, 165.0000000000000000 ) ) ;
#28378 = LINE ( 'NONE', #17072, #28579 ) ;
#28379 = EDGE_CURVE ( 'NONE', #31866, #29044, #3699, .T. ) ;
#28380 = VECTOR ( 'NONE', #6136, 1000.000000000000000 ) ;
#28381 = LINE ( 'NONE', #9126, #46238 ) ;
#28382 = EDGE_LOOP ( 'NONE', ( #49116, #24254, #2253, #15968 ) ) ;
#28383 = EDGE_CURVE ( 'NONE', #8172, #36234, #34137, .T. ) ;
#28384 = CARTESIAN_POINT ( 'NONE',  ( 0.000000000000000000, 0.000000000000000000, 0.000000000000000000 ) ) ;
#28385 = EDGE_CURVE ( 'NONE', #28730, #40964, #13697, .T. ) ;
#28386 = DIRECTION ( 'NONE',  ( -1.000000000000000000, -0.000000000000000000, -0.000000000000000000 ) ) ;
#28387 = PLANE ( 'NONE',  #30188 ) ;
#28388 = CARTESIAN_POINT ( 'NONE',  ( 31.55402655318503236, 0.000000000000000000, 165.0000000000000000 ) ) ;
#28389 = AXIS2_PLACEMENT_3D ( 'NONE', #47871, #13250, #24330 ) ;
#28390 = AXIS2_PLACEMENT_3D ( 'NONE', #26354, #37919, #33555 ) ;
#28391 = CARTESIAN_POINT ( 'NONE',  ( 196.8526953830863135, -154.8119894309599260, 22.84256005001721945 ) ) ;
#28392 = CARTESIAN_POINT ( 'NONE',  ( -86.69597344681494633, 1.750000000000010658, 120.8182875569279702 ) ) ;
#28393 = EDGE_CURVE ( 'NONE', #5041, #40908, #7603, .T. ) ;
#28394 = CARTESIAN_POINT ( 'NONE',  ( -69.99999999999879208, 17.00000000000000000, 5.000000000000004441 ) ) ;
#28395 = AXIS2_PLACEMENT_3D ( 'NONE', #22090, #2581, #41090 ) ;
#28396 = ORIENTED_EDGE ( 'NONE', *, *, #39469, .T. ) ;
#28397 = DIRECTION ( 'NONE',  ( 1.000000000000000000, 0.000000000000000000, -4.625929269271584521E-16 ) ) ;
#28398 = EDGE_CURVE ( 'NONE', #49373, #5769, #12840, .T. ) ;
#28399 = EDGE_CURVE ( 'NONE', #36023, #25392, #37081, .T. ) ;
#28400 = CYLINDRICAL_SURFACE ( 'NONE', #18846, 1.750000000000015543 ) ;
#28401 = ORIENTED_EDGE ( 'NONE', *, *, #23346, .T. ) ;
#28402 = DIRECTION ( 'NONE',  ( 0.000000000000000000, 0.000000000000000000, 1.000000000000000000 ) ) ;
#28403 = CARTESIAN_POINT ( 'NONE',  ( 359.9999999999999432, -174.9999999999999432, 355.9999999999998295 ) ) ;
#28404 = LINE ( 'NONE', #39957, #37335 ) ;
#28405 = VERTEX_POINT ( 'NONE', #46474 ) ;
#28406 = FACE_OUTER_BOUND ( 'NONE', #9678, .T. ) ;
#28407 = VERTEX_POINT ( 'NONE', #11366 ) ;
#28408 = ORIENTED_EDGE ( 'NONE', *, *, #8052, .T. ) ;
#28409 = CARTESIAN_POINT ( 'NONE',  ( -0.5270093351535434234, 0.6444734225979527054, 9.985686052694763504 ) ) ;
#28410 = CIRCLE ( 'NONE', #24318, 2.000000000000001776 ) ;
#28411 = ORIENTED_EDGE ( 'NONE', *, *, #38074, .F. ) ;
#28412 = DIRECTION ( 'NONE',  ( -1.000000000000000000, -0.000000000000000000, -0.000000000000000000 ) ) ;
#28413 = DIRECTION ( 'NONE',  ( -1.000000000000000000, -0.000000000000000000, -0.000000000000000000 ) ) ;
#28414 = AXIS2_PLACEMENT_3D ( 'NONE', #37092, #17813, #10379 ) ;
#28415 = ORIENTED_EDGE ( 'NONE', *, *, #48672, .T. ) ;
#28416 = ORIENTED_EDGE ( 'NONE', *, *, #29778, .F. ) ;
#28417 = EDGE_CURVE ( 'NONE', #49373, #43794, #3147, .T. ) ;
#28418 = CARTESIAN_POINT ( 'NONE',  ( 181.0000000000000853, -164.9999999999999432, -115.0000000000001990 ) ) ;
#28419 = VERTEX_POINT ( 'NONE', #11630 ) ;
#28420 = CARTESIAN_POINT ( 'NONE',  ( -34.08406891383351933, 15.63733501198486309, -8.192531242611266862 ) ) ;
#28421 = LINE ( 'NONE', #35632, #20123 ) ;
#28422 = DIRECTION ( 'NONE',  ( -0.000000000000000000, -0.000000000000000000, -1.000000000000000000 ) ) ;
#28423 =( BOUNDED_CURVE ( )  B_SPLINE_CURVE ( 3, ( #48956, #13845, #12854, #47964 ),
 .UNSPECIFIED., .F., .F. ) 
 B_SPLINE_CURVE_WITH_KNOTS ( ( 4, 4 ),
 ( 4.712388980384689674, 6.283185307179586232 ),
 .UNSPECIFIED. ) 
 CURVE ( )  GEOMETRIC_REPRESENTATION_ITEM ( )  RATIONAL_B_SPLINE_CURVE ( ( 1.000000000000000000, 0.8047378541243649375, 0.8047378541243649375, 1.000000000000000000 ) ) 
 REPRESENTATION_ITEM ( '' )  );
#28424 = ORIENTED_EDGE ( 'NONE', *, *, #3400, .T. ) ;
#28425 = CARTESIAN_POINT ( 'NONE',  ( 164.9999999999999716, -256.4999999999999432, -349.9999999999999432 ) ) ;
#28426 = CARTESIAN_POINT ( 'NONE',  ( 7.129058724844953510, 15.30620660340485095, 9.178419661560148768 ) ) ;
#28427 = EDGE_LOOP ( 'NONE', ( #145, #10179, #24176, #36255, #40396, #37362 ) ) ;
#28428 = ADVANCED_FACE ( 'NONE', ( #14711 ), #34227, .T. ) ;
#28429 = ORIENTED_EDGE ( 'NONE', *, *, #8906, .T. ) ;
#28430 = ORIENTED_EDGE ( 'NONE', *, *, #20226, .F. ) ;
#28431 = CARTESIAN_POINT ( 'NONE',  ( -69.99999999999879208, 17.00000000000000000, 30.00000000000000000 ) ) ;
#28432 =( BOUNDED_CURVE ( )  B_SPLINE_CURVE ( 3, ( #46156, #11051, #22846, #38524 ),
 .UNSPECIFIED., .F., .F. ) 
 B_SPLINE_CURVE_WITH_KNOTS ( ( 4, 4 ),
 ( 3.141592653589793116, 4.712388980384689674 ),
 .UNSPECIFIED. ) 
 CURVE ( )  GEOMETRIC_REPRESENTATION_ITEM ( )  RATIONAL_B_SPLINE_CURVE ( ( 1.000000000000000000, 0.8047378541243649375, 0.8047378541243649375, 1.000000000000000000 ) ) 
 REPRESENTATION_ITEM ( '' )  );
#28433 = DIRECTION ( 'NONE',  ( 1.000000000000000000, 0.000000000000000000, 0.000000000000000000 ) ) ;
#28434 = ORIENTED_EDGE ( 'NONE', *, *, #28081, .F. ) ;
#28435 = VECTOR ( 'NONE', #23554, 1000.000000000000000 ) ;
#28436 = CARTESIAN_POINT ( 'NONE',  ( 153.3040265531850537, 1.750000000000010214, 40.81828755692798438 ) ) ;
#28437 = CARTESIAN_POINT ( 'NONE',  ( -34.08406891383351933, 15.63733501198486309, -8.192531242611266862 ) ) ;
#28438 = CYLINDRICAL_SURFACE ( 'NONE', #25606, 1.750000000000001554 ) ;
#28439 = EDGE_CURVE ( 'NONE', #24182, #38545, #30115, .T. ) ;
#28440 = LINE ( 'NONE', #16373, #12870 ) ;
#28441 = CARTESIAN_POINT ( 'NONE',  ( -167.7210997126620384, -1.750000000000009548, -158.1565861772249377 ) ) ;
#28442 = ADVANCED_FACE ( 'NONE', ( #27281 ), #49804, .F. ) ;
#28443 = CARTESIAN_POINT ( 'NONE',  ( 36.28567981536807707, 9.465698090293649614, -9.422646554964174470 ) ) ;
#28444 = DIRECTION ( 'NONE',  ( 0.000000000000000000, -1.000000000000000000, 0.000000000000000000 ) ) ;
#28445 = CARTESIAN_POINT ( 'NONE',  ( -87.72109971266203843, 1.750000000000009548, -118.1565861772249519 ) ) ;
#28446 = ADVANCED_FACE ( 'NONE', ( #22405 ), #7531, .T. ) ;
#28447 = CARTESIAN_POINT ( 'NONE',  ( 164.9999999999999716, -81.49999999999997158, -350.0000000000001705 ) ) ;
#28448 = LINE ( 'NONE', #16633, #13773 ) ;
#28449 = EDGE_CURVE ( 'NONE', #17284, #9063, #36605, .T. ) ;
#28450 = EDGE_CURVE ( 'NONE', #39659, #2507, #18548, .T. ) ;
#28451 = DIRECTION ( 'NONE',  ( -1.000000000000000000, -0.000000000000000000, 2.312964634635864737E-16 ) ) ;
#28452 = VECTOR ( 'NONE', #14023, 1000.000000000000000 ) ;
#28453 = DIRECTION ( 'NONE',  ( -0.000000000000000000, -1.000000000000000000, -0.000000000000000000 ) ) ;
#28454 = ORIENTED_EDGE ( 'NONE', *, *, #5477, .T. ) ;
#28455 = CARTESIAN_POINT ( 'NONE',  ( -128.4459734468149179, 0.000000000000000000, 165.0000000000000000 ) ) ;
#28456 = EDGE_CURVE ( 'NONE', #44740, #45613, #7266, .T. ) ;
#28457 = CARTESIAN_POINT ( 'NONE',  ( 115.0540265531850395, 2.143131898507847836E-16, 159.0682875569279702 ) ) ;
#28458 = LINE ( 'NONE', #40251, #11080 ) ;
#28459 = CARTESIAN_POINT ( 'NONE',  ( 135.0000000000009663, 17.00000000000000000, -24.99999999999999289 ) ) ;
#28460 = ORIENTED_EDGE ( 'NONE', *, *, #9578, .T. ) ;
#28461 = CYLINDRICAL_SURFACE ( 'NONE', #37932, 1.750000000000015543 ) ;
#28462 = EDGE_CURVE ( 'NONE', #3211, #5210, #15469, .T. ) ;
#28463 = DIRECTION ( 'NONE',  ( 6.938893903907233900E-15, 0.000000000000000000, -1.000000000000000000 ) ) ;
#28464 = ORIENTED_EDGE ( 'NONE', *, *, #27122, .F. ) ;
#28465 = CARTESIAN_POINT ( 'NONE',  ( 0.3862712429686727678, 1.188820645368945605, -10.00000000000000000 ) ) ;
#28466 = CARTESIAN_POINT ( 'NONE',  ( 181.0000000000000000, 6.000000000000060396, -350.0000000000001705 ) ) ;
#28467 = ORIENTED_EDGE ( 'NONE', *, *, #9208, .T. ) ;
#28468 = DIRECTION ( 'NONE',  ( -1.000000000000000000, 3.172065784643302499E-16, 1.942330104924128867E-32 ) ) ;
#28469 = B_SPLINE_SURFACE_WITH_KNOTS ( 'NONE', 3, 3, ( 
 ( #39226, #19711, #35390, #10998 ),
 ( #31531, #47117, #42299, #38473 ),
 ( #3285, #18933, #43807, #36137 ),
 ( #20981, #17124, #40224, #36912 ) ),
 .UNSPECIFIED., .F., .F., .F.,
 ( 4, 4 ),
 ( 4, 4 ),
 ( 0.000000000000000000, 1.000000000000000000 ),
 ( 0.000000000000000000, 1.000000000000000000 ),
 .UNSPECIFIED. ) ;
#28470 = VERTEX_POINT ( 'NONE', #30890 ) ;
#28471 = VERTEX_POINT ( 'NONE', #38842 ) ;
#28472 = ORIENTED_EDGE ( 'NONE', *, *, #29293, .F. ) ;
#28473 = CARTESIAN_POINT ( 'NONE',  ( 210.0000000000000568, 0.000000000000000000, 40.81828755692798438 ) ) ;
#28474 = CARTESIAN_POINT ( 'NONE',  ( -168.4459734468149747, 0.000000000000000000, 162.5682875569279702 ) ) ;
#28475 = ORIENTED_EDGE ( 'NONE', *, *, #32022, .T. ) ;
#28476 = LINE ( 'NONE', #47923, #14747 ) ;
#28477 = CARTESIAN_POINT ( 'NONE',  ( 5.551115123125782702E-14, -180.9999999999999716, 357.9999999999997726 ) ) ;
#28478 = DIRECTION ( 'NONE',  ( -1.000000000000000000, -0.000000000000000000, -0.000000000000000000 ) ) ;
#28479 = DIRECTION ( 'NONE',  ( 0.000000000000000000, 2.537652627714642000E-15, 1.000000000000000000 ) ) ;
#28480 = VERTEX_POINT ( 'NONE', #7016 ) ;
#28481 = DIRECTION ( 'NONE',  ( 0.000000000000000000, 0.000000000000000000, 1.000000000000000000 ) ) ;
#28482 = EDGE_LOOP ( 'NONE', ( #5818, #18709 ) ) ;
#28483 = AXIS2_PLACEMENT_3D ( 'NONE', #22430, #3429, #7815 ) ;
#28484 = CARTESIAN_POINT ( 'NONE',  ( 155.0540265531850537, -1.025126265847089213, -37.43171244307202272 ) ) ;
#28485 = DIRECTION ( 'NONE',  ( -0.000000000000000000, -0.000000000000000000, -1.000000000000000000 ) ) ;
#28486 = VERTEX_POINT ( 'NONE', #38590 ) ;
#28487 = DIRECTION ( 'NONE',  ( 1.000000000000000000, 0.000000000000000000, 0.000000000000000000 ) ) ;
#28488 = CARTESIAN_POINT ( 'NONE',  ( -48.44597344681496054, 1.025126265847089435, 39.06828755692797728 ) ) ;
#28489 = ORIENTED_EDGE ( 'NONE', *, *, #740, .F. ) ;
#28490 = CARTESIAN_POINT ( 'NONE',  ( -4.945973446814917018, -1.025126265847097207, -40.93171244307204404 ) ) ;
#28491 = PLANE ( 'NONE',  #3622 ) ;
#28492 = PLANE ( 'NONE',  #49120 ) ;
#28493 = DIRECTION ( 'NONE',  ( 0.000000000000000000, 0.000000000000000000, 1.000000000000000000 ) ) ;
#28494 = EDGE_CURVE ( 'NONE', #7807, #25713, #45628, .T. ) ;
#28495 = EDGE_CURVE ( 'NONE', #16448, #26090, #35004, .T. ) ;
#28496 = ORIENTED_EDGE ( 'NONE', *, *, #21120, .T. ) ;
#28497 = CARTESIAN_POINT ( 'NONE',  ( 166.9999999999999716, -268.5000000000000000, -114.9999999999999289 ) ) ;
#28498 = CYLINDRICAL_SURFACE ( 'NONE', #13577, 3.750000000000000000 ) ;
#28499 = EDGE_CURVE ( 'NONE', #26133, #12204, #49629, .T. ) ;
#28500 = CARTESIAN_POINT ( 'NONE',  ( -25.61277432017861955, 22.36370378792854297, 7.906207997025717304 ) ) ;
#28501 = ORIENTED_EDGE ( 'NONE', *, *, #43669, .F. ) ;
#28502 = ORIENTED_EDGE ( 'NONE', *, *, #31661, .T. ) ;
#28503 = EDGE_CURVE ( 'NONE', #23001, #14108, #38336, .T. ) ;
#28504 = PRODUCT_CONTEXT ( 'NONE', #7939, 'mechanical' ) ;
#28505 = EDGE_CURVE ( 'NONE', #47505, #41166, #18796, .T. ) ;
#28506 = PLANE ( 'NONE',  #5650 ) ;
#28507 = CARTESIAN_POINT ( 'NONE',  ( 192.2789002873380184, -1.750000000000010214, -120.2068387089191219 ) ) ;
#28508 = DIRECTION ( 'NONE',  ( -0.000000000000000000, -0.000000000000000000, -1.000000000000000000 ) ) ;
#28509 = CARTESIAN_POINT ( 'NONE',  ( 0.000000000000000000, 17.00000000000000000, 0.000000000000000000 ) ) ;
#28510 = VERTEX_POINT ( 'NONE', #50058 ) ;
#28511 = EDGE_CURVE ( 'NONE', #25029, #47386, #122, .T. ) ;
#28512 = DIRECTION ( 'NONE',  ( -0.000000000000000000, -0.000000000000000000, -1.000000000000000000 ) ) ;
#28513 = EDGE_CURVE ( 'NONE', #25177, #45390, #42657, .T. ) ;
#28514 = CARTESIAN_POINT ( 'NONE',  ( 356.0000000000000000, -165.0000000000001137, -340.0000000000002842 ) ) ;
#28515 = DIRECTION ( 'NONE',  ( -2.312964634635843537E-16, 0.000000000000000000, -1.000000000000000000 ) ) ;
#28516 = CARTESIAN_POINT ( 'NONE',  ( 210.0000000000000568, 2.143131898507881856E-16, 119.0682875569279560 ) ) ;
#28517 = ORIENTED_EDGE ( 'NONE', *, *, #31296, .F. ) ;
#28518 = LINE ( 'NONE', #23905, #245 ) ;
#28520 = VERTEX_POINT ( 'NONE', #32144 ) ;
#28519 = AXIS2_PLACEMENT_3D ( 'NONE', #10447, #18137, #49651 ) ;
#28521 = CARTESIAN_POINT ( 'NONE',  ( 356.0000000000001137, 181.0000000000000284, 349.9999999999998863 ) ) ;
#28522 = ORIENTED_EDGE ( 'NONE', *, *, #40565, .F. ) ;
#28523 = CARTESIAN_POINT ( 'NONE',  ( 194.3291528190321742, -1.750000000000010436, -80.20683870891910772 ) ) ;
#28524 = DIRECTION ( 'NONE',  ( -0.000000000000000000, -1.000000000000000000, -0.000000000000000000 ) ) ;
#28525 = CYLINDRICAL_SURFACE ( 'NONE', #18297, 4.000000000000003553 ) ;
#28526 = CARTESIAN_POINT ( 'NONE',  ( -124.9459734468149463, 2.143131898507847836E-16, -117.4317124430720725 ) ) ;
#28527 = ORIENTED_EDGE ( 'NONE', *, *, #13, .T. ) ;
#28528 = CARTESIAN_POINT ( 'NONE',  ( -8.445973446814964092, 1.025126265847097207, -77.43171244307197298 ) ) ;
#28529 = ORIENTED_EDGE ( 'NONE', *, *, #10486, .T. ) ;
#28530 = CARTESIAN_POINT ( 'NONE',  ( -85.67084718096784002, 1.750000000000009548, -0.2068387089191121020 ) ) ;
#28531 = PLANE ( 'NONE',  #32282 ) ;
#28532 = DIRECTION ( 'NONE',  ( -1.586032892321652236E-16, -1.000000000000000000, -6.853681917100419162E-49 ) ) ;
#28533 = CARTESIAN_POINT ( 'NONE',  ( 339.9999999999998863, -185.0000000000001421, -349.9999999999998863 ) ) ;
#28534 = ORIENTED_EDGE ( 'NONE', *, *, #46925, .F. ) ;
#28535 = VERTEX_POINT ( 'NONE', #9046 ) ;
#28536 = CARTESIAN_POINT ( 'NONE',  ( -0.3093295598751883979, 2.058753478587400654, 9.888794896520666455 ) ) ;
#28537 = EDGE_CURVE ( 'NONE', #19596, #34874, #28290, .T. ) ;
#28538 = EDGE_LOOP ( 'NONE', ( #37043, #23518, #6048, #50062 ) ) ;
#28539 = CARTESIAN_POINT ( 'NONE',  ( 185.0000000000000000, 165.0000000000000000, -344.0000000000001137 ) ) ;
#28540 = CARTESIAN_POINT ( 'NONE',  ( -208.4459734468149463, 0.000000000000000000, -120.9317124430720156 ) ) ;
#28541 = CARTESIAN_POINT ( 'NONE',  ( 193.3040265531851105, 1.750000000000009992, 160.8182875569279702 ) ) ;
#28542 = ORIENTED_EDGE ( 'NONE', *, *, #50551, .T. ) ;
#28543 = CARTESIAN_POINT ( 'NONE',  ( 73.30402655318508209, 1.750000000000009992, -159.1817124430720298 ) ) ;
#28544 = DIRECTION ( 'NONE',  ( -1.000000000000000000, 0.000000000000000000, 0.000000000000000000 ) ) ;
#28545 = DIRECTION ( 'NONE',  ( 1.000000000000000000, -3.172065745548403743E-16, 1.587271980518778491E-16 ) ) ;
#28546 = CARTESIAN_POINT ( 'NONE',  ( 210.0000000000000568, 0.000000000000000000, -159.1817124430720298 ) ) ;
#28547 = DIRECTION ( 'NONE',  ( 0.000000000000000000, 1.000000000000000000, 0.000000000000000000 ) ) ;
#28548 = ORIENTED_EDGE ( 'NONE', *, *, #3586, .T. ) ;
#28549 = VECTOR ( 'NONE', #32947, 1000.000000000000000 ) ;
#28550 = VERTEX_POINT ( 'NONE', #8799 ) ;
#28551 = ORIENTED_EDGE ( 'NONE', *, *, #9316, .T. ) ;
#28552 = DIRECTION ( 'NONE',  ( -1.000000000000000000, 0.000000000000000000, 0.000000000000000000 ) ) ;
#28553 = FILL_AREA_STYLE_COLOUR ( '', #8694 ) ;
#28554 = CARTESIAN_POINT ( 'NONE',  ( 35.00000000000152767, 17.00000000000000000, 35.00000000000000000 ) ) ;
#28555 = VERTEX_POINT ( 'NONE', #23680 ) ;
#28556 = CARTESIAN_POINT ( 'NONE',  ( -47.22310614333779455, -16.46562252335923660, -3.760136334089591248 ) ) ;
#28557 = ORIENTED_EDGE ( 'NONE', *, *, #19975, .F. ) ;
#28558 = SHAPE_REPRESENTATION_RELATIONSHIP ( 'NONE' , 'NONE' ,  #8438, #6301 ) ;
#28559 =( BOUNDED_CURVE ( )  B_SPLINE_CURVE ( 3, ( #25864, #41512, #37679, #15336 ),
 .UNSPECIFIED., .F., .F. ) 
 B_SPLINE_CURVE_WITH_KNOTS ( ( 4, 4 ),
 ( 1.570796326794896558, 3.141592653589793116 ),
 .UNSPECIFIED. ) 
 CURVE ( )  GEOMETRIC_REPRESENTATION_ITEM ( )  RATIONAL_B_SPLINE_CURVE ( ( 1.000000000000000000, 0.8047378541243649375, 0.8047378541243649375, 1.000000000000000000 ) ) 
 REPRESENTATION_ITEM ( '' )  );
#28560 = DIRECTION ( 'NONE',  ( 0.000000000000000000, 0.000000000000000000, 1.000000000000000000 ) ) ;
#28561 = CARTESIAN_POINT ( 'NONE',  ( -88.44597344681491791, 2.143131898507880377E-16, -160.9317124430720298 ) ) ;
#28562 = CARTESIAN_POINT ( 'NONE',  ( 0.000000000000000000, -182.9999999999999716, -344.0000000000001705 ) ) ;
#28563 = CARTESIAN_POINT ( 'NONE',  ( -47.72109971266203132, 1.750000000000009548, 81.84341382277507648 ) ) ;
#28564 = CYLINDRICAL_SURFACE ( 'NONE', #38088, 1.749999999999973799 ) ;
#28565 = CARTESIAN_POINT ( 'NONE',  ( -127.7210997126620242, -1.749999999999996891, 79.79316129108087807 ) ) ;
#28566 = ORIENTED_EDGE ( 'NONE', *, *, #46563, .F. ) ;
#28567 = EDGE_CURVE ( 'NONE', #35690, #11870, #16492, .T. ) ;
#28568 = CARTESIAN_POINT ( 'NONE',  ( 356.0000000000000000, 165.0000000000000000, -340.0000000000001137 ) ) ;
#28569 = B_SPLINE_SURFACE_WITH_KNOTS ( 'NONE', 3, 3, ( 
 ( #18169, #49438, #14325, #45607 ),
 ( #29992, #10481, #26128, #40378 ),
 ( #48020, #47527, #12408, #11914 ),
 ( #12906, #43453, #5216, #4461 ) ),
 .UNSPECIFIED., .F., .F., .F.,
 ( 4, 4 ),
 ( 4, 4 ),
 ( 0.000000000000000000, 1.000000000000000000 ),
 ( 0.000000000000000000, 1.000000000000000000 ),
 .UNSPECIFIED. ) ;
#28570 = DIRECTION ( 'NONE',  ( 0.000000000000000000, 0.000000000000000000, 1.000000000000000000 ) ) ;
#28571 = DIRECTION ( 'NONE',  ( 1.000000000000000000, 0.000000000000000000, 0.000000000000000000 ) ) ;
#28572 = VERTEX_POINT ( 'NONE', #15985 ) ;
#28573 = PLANE ( 'NONE',  #6488 ) ;
#28574 = ORIENTED_EDGE ( 'NONE', *, *, #39520, .F. ) ;
#28575 = CARTESIAN_POINT ( 'NONE',  ( 350.0000000000000000, -180.9999999999999716, -340.0000000000001705 ) ) ;
#28576 =( BOUNDED_CURVE ( )  B_SPLINE_CURVE ( 3, ( #15149, #22333, #38010, #2826 ),
 .UNSPECIFIED., .F., .F. ) 
 B_SPLINE_CURVE_WITH_KNOTS ( ( 4, 4 ),
 ( 1.570796326794896558, 3.141592653589793116 ),
 .UNSPECIFIED. ) 
 CURVE ( )  GEOMETRIC_REPRESENTATION_ITEM ( )  RATIONAL_B_SPLINE_CURVE ( ( 1.000000000000000000, 0.8047378541243649375, 0.8047378541243649375, 1.000000000000000000 ) ) 
 REPRESENTATION_ITEM ( '' )  );
#28577 = DIRECTION ( 'NONE',  ( 1.000000000000000000, 0.000000000000000000, 0.000000000000000000 ) ) ;
#28578 = ORIENTED_EDGE ( 'NONE', *, *, #35773, .F. ) ;
#28579 = VECTOR ( 'NONE', #8867, 1000.000000000000000 ) ;
#28580 = ORIENTED_EDGE ( 'NONE', *, *, #5268, .F. ) ;
#28581 = AXIS2_PLACEMENT_3D ( 'NONE', #41063, #21821, #21057 ) ;
#28582 = LINE ( 'NONE', #8587, #44235 ) ;
#28583 = CARTESIAN_POINT ( 'NONE',  ( -206.6959734468149463, -1.750000000000010214, 40.81828755692798438 ) ) ;
#28584 = CARTESIAN_POINT ( 'NONE',  ( 181.0000000000000000, -272.4999999999999432, -349.9999999999999432 ) ) ;
#28585 = EDGE_LOOP ( 'NONE', ( #3163, #50687, #39722, #38387, #5696 ) ) ;
#28586 = VERTEX_POINT ( 'NONE', #28034 ) ;
#28587 = CARTESIAN_POINT ( 'NONE',  ( -4.641001526964561918, -50.00000000000000711, -8.016098858316205167 ) ) ;
#28588 = CARTESIAN_POINT ( 'NONE',  ( -164.9999999999994031, 17.00000000000000000, -54.99999999999999289 ) ) ;
#28589 = ADVANCED_FACE ( 'NONE', ( #12377 ), #43178, .T. ) ;
#28590 = VECTOR ( 'NONE', #22200, 1000.000000000000000 ) ;
#28591 = ORIENTED_EDGE ( 'NONE', *, *, #4921, .T. ) ;
#28592 = ORIENTED_EDGE ( 'NONE', *, *, #50581, .T. ) ;
#28593 = CARTESIAN_POINT ( 'NONE',  ( -0.5953091869874307385, -3.900377600830043257, 6.494306115488110542 ) ) ;
#28594 = CARTESIAN_POINT ( 'NONE',  ( 85.00000000000123634, 17.00000000000000000, 5.000000000000004441 ) ) ;
#28595 = CARTESIAN_POINT ( 'NONE',  ( 350.0000000000000000, 169.0000000000000000, -358.0000000000002274 ) ) ;
#28596 = CARTESIAN_POINT ( 'NONE',  ( 113.3040265531850537, -1.749999999999997335, -119.1817124430720440 ) ) ;
#28597 = ORIENTED_EDGE ( 'NONE', *, *, #27578, .T. ) ;
#28598 = EDGE_LOOP ( 'NONE', ( #36612, #39570, #31015, #3575, #601, #4982 ) ) ;
#28599 = ORIENTED_EDGE ( 'NONE', *, *, #20206, .T. ) ;
#28600 = LINE ( 'NONE', #35567, #21773 ) ;
#28601 = PLANE ( 'NONE',  #27085 ) ;
#28602 = EDGE_LOOP ( 'NONE', ( #31129, #40571, #49415, #40117, #46075, #5882 ) ) ;
#28603 = ORIENTED_EDGE ( 'NONE', *, *, #23969, .F. ) ;
#28604 = CARTESIAN_POINT ( 'NONE',  ( -4.641001526964560142, -33.28196331604080171, -8.016098858316199838 ) ) ;
#28605 = CARTESIAN_POINT ( 'NONE',  ( 29.39982726364966581, 16.78152490921169360, 8.356839323120299312 ) ) ;
#28606 = ORIENTED_EDGE ( 'NONE', *, *, #37535, .T. ) ;
#28607 = ORIENTED_EDGE ( 'NONE', *, *, #20609, .T. ) ;
#28608 = FACE_OUTER_BOUND ( 'NONE', #28382, .T. ) ;
#28609 = DIRECTION ( 'NONE',  ( 6.203854594147707562E-25, -2.067951531382569187E-25, 1.000000000000000000 ) ) ;
#28611 = ORIENTED_EDGE ( 'NONE', *, *, #48191, .T. ) ;
#28610 = AXIS2_PLACEMENT_3D ( 'NONE', #24427, #36486, #32626 ) ;
#28612 = CARTESIAN_POINT ( 'NONE',  ( 7.608425291889091113, -36.72004717559254772, 7.697694107796188234 ) ) ;
#28613 = FACE_BOUND ( 'NONE', #23046, .T. ) ;
#28614 = LINE ( 'NONE', #24525, #15463 ) ;
#28615 = VECTOR ( 'NONE', #17025, 1000.000000000000000 ) ;
#28616 = DIRECTION ( 'NONE',  ( -2.874857526315639190E-31, 1.000000000000000000, -2.537652627714642000E-15 ) ) ;
#28617 = ORIENTED_EDGE ( 'NONE', *, *, #33672, .T. ) ;
#28618 = AXIS2_PLACEMENT_3D ( 'NONE', #42037, #46367, #26135 ) ;
#28619 = EDGE_CURVE ( 'NONE', #39109, #5029, #36007, .T. ) ;
#28621 = VECTOR ( 'NONE', #48897, 1000.000000000000000 ) ;
#28620 = CARTESIAN_POINT ( 'NONE',  ( -47.88254548617756967, 14.43607691413558669, -3.760136334089591248 ) ) ;
#28622 = CARTESIAN_POINT ( 'NONE',  ( 113.3040265531850537, 0.000000000000000000, -165.0000000000000000 ) ) ;
#28623 = CARTESIAN_POINT ( 'NONE',  ( 342.0000000000000000, -167.8284271247462414, -342.8284271247464972 ) ) ;
#28624 = DIRECTION ( 'NONE',  ( -1.000000000000000000, -0.000000000000000000, -0.000000000000000000 ) ) ;
#28625 = EDGE_CURVE ( 'NONE', #34290, #48865, #33833, .T. ) ;
#28626 = AXIS2_PLACEMENT_3D ( 'NONE', #1208, #29157, #13490 ) ;
#28627 = LINE ( 'NONE', #31489, #16347 ) ;
#28628 = EDGE_CURVE ( 'NONE', #33142, #15045, #40100, .T. ) ;
#28629 = DIRECTION ( 'NONE',  ( 1.000000000000000000, 0.000000000000000000, 0.000000000000000000 ) ) ;
#28630 = EDGE_CURVE ( 'NONE', #50033, #38220, #4000, .T. ) ;
#28631 = CARTESIAN_POINT ( 'NONE',  ( 73.30402655318508209, 0.000000000000000000, -165.0000000000000000 ) ) ;
#28632 = CARTESIAN_POINT ( 'NONE',  ( 1.540617191852273526, -1.371546265746151017, 9.891980816076527461 ) ) ;
#28633 = EDGE_CURVE ( 'NONE', #8236, #16307, #20079, .T. ) ;
#28634 = VERTEX_POINT ( 'NONE', #16732 ) ;
#28635 = FACE_OUTER_BOUND ( 'NONE', #46702, .T. ) ;
#28636 = DIRECTION ( 'NONE',  ( -0.000000000000000000, -1.000000000000000000, -0.000000000000000000 ) ) ;
#28637 = ORIENTED_EDGE ( 'NONE', *, *, #27578, .F. ) ;
#28638 = CARTESIAN_POINT ( 'NONE',  ( 210.0000000000000568, 0.000000000000000000, 80.81828755692798438 ) ) ;
#28639 = CARTESIAN_POINT ( 'NONE',  ( 1.448406091252584238, -0.9360325558322883932, 9.928159647716132241 ) ) ;
#28640 = CARTESIAN_POINT ( 'NONE',  ( 164.9999999999999716, -272.4999999999999432, -344.0000000000001137 ) ) ;
#28641 = ORIENTED_EDGE ( 'NONE', *, *, #40242, .F. ) ;
#28642 = CARTESIAN_POINT ( 'NONE',  ( -1.540526284687967706, 1.371707213411501147, 9.886433018048069954 ) ) ;
#28643 = EDGE_CURVE ( 'NONE', #9127, #2518, #40722, .T. ) ;
#28645 = VERTEX_POINT ( 'NONE', #47242 ) ;
#28644 = ADVANCED_FACE ( 'NONE', ( #46983, #19820 ), #39346, .T. ) ;
#28646 = VECTOR ( 'NONE', #26635, 1000.000000000000000 ) ;
#28647 = CARTESIAN_POINT ( 'NONE',  ( -33.64889274059387958, 3.704246042440976439, 8.356839323120299312 ) ) ;
#28648 = CARTESIAN_POINT ( 'NONE',  ( 1.337801958641917199, 1.088266084286984015, 9.928159647716135794 ) ) ;
#28649 = VECTOR ( 'NONE', #39764, 1000.000000000000000 ) ;
#28650 = EDGE_CURVE ( 'NONE', #16704, #11488, #45920, .T. ) ;
#28651 = ADVANCED_FACE ( 'NONE', ( #43664 ), #43421, .F. ) ;
#28652 = VECTOR ( 'NONE', #4228, 1000.000000000000000 ) ;
#28653 = ORIENTED_EDGE ( 'NONE', *, *, #49759, .T. ) ;
#28654 = LINE ( 'NONE', #28909, #6559 ) ;
#28655 = CARTESIAN_POINT ( 'NONE',  ( 210.0000000000000568, 0.000000000000000000, -159.1817124430720298 ) ) ;
#28656 =( BOUNDED_CURVE ( )  B_SPLINE_CURVE ( 3, ( #11118, #7265, #42399, #22912 ),
 .UNSPECIFIED., .F., .F. ) 
 B_SPLINE_CURVE_WITH_KNOTS ( ( 4, 4 ),
 ( 0.000000000000000000, 1.570796326794896780 ),
 .UNSPECIFIED. ) 
 CURVE ( )  GEOMETRIC_REPRESENTATION_ITEM ( )  RATIONAL_B_SPLINE_CURVE ( ( 1.000000000000000000, 0.8047378541243649375, 0.8047378541243649375, 1.000000000000000000 ) ) 
 REPRESENTATION_ITEM ( '' )  );
#28657 = ORIENTED_EDGE ( 'NONE', *, *, #25545, .T. ) ;
#28658 = ORIENTED_EDGE ( 'NONE', *, *, #26929, .F. ) ;
#28659 = VECTOR ( 'NONE', #12829, 1000.000000000000000 ) ;
#28660 = EDGE_CURVE ( 'NONE', #6936, #24694, #47495, .T. ) ;
#28661 = CARTESIAN_POINT ( 'NONE',  ( 0.7606162131530698201, -1.296876929034913140, 9.953784399990620813 ) ) ;
#28662 = ORIENTED_EDGE ( 'NONE', *, *, #14868, .F. ) ;
#28663 = CARTESIAN_POINT ( 'NONE',  ( -4.672045878990125800, 50.00000000000000711, 1.847720168420772691 ) ) ;
#28664 = DIRECTION ( 'NONE',  ( -0.000000000000000000, -0.000000000000000000, -1.000000000000000000 ) ) ;
#28665 = CARTESIAN_POINT ( 'NONE',  ( 0.2050626648100478400, -1.807624707196173519, 9.903764339332001398 ) ) ;
#28666 = ORIENTED_EDGE ( 'NONE', *, *, #43268, .T. ) ;
#28667 = CARTESIAN_POINT ( 'NONE',  ( 0.000000000000000000, 17.00000000000000000, 0.000000000000000000 ) ) ;
#28668 = FACE_OUTER_BOUND ( 'NONE', #2653, .T. ) ;
#28669 = VERTEX_POINT ( 'NONE', #5936 ) ;
#28670 = ORIENTED_EDGE ( 'NONE', *, *, #49121, .T. ) ;
#28671 = ORIENTED_EDGE ( 'NONE', *, *, #32837, .T. ) ;
#28672 = CARTESIAN_POINT ( 'NONE',  ( -1.275971930252334019, 0.1228246474626440710, 9.957892297621013356 ) ) ;
#28673 = VERTEX_POINT ( 'NONE', #29798 ) ;
#28674 = EDGE_CURVE ( 'NONE', #37527, #46181, #45157, .T. ) ;
#28675 = CARTESIAN_POINT ( 'NONE',  ( 0.9601844228325747688, -0.8491947203466810867, 9.967237415621763574 ) ) ;
#28676 = CARTESIAN_POINT ( 'NONE',  ( 75.05402655318508209, 0.000000000000000000, 162.5682875569279702 ) ) ;
#28677 = PLANE ( 'NONE',  #19851 ) ;
#28678 = EDGE_CURVE ( 'NONE', #23532, #16113, #41474, .T. ) ;
#28679 = DIRECTION ( 'NONE',  ( 0.000000000000000000, 1.000000000000000000, 0.000000000000000000 ) ) ;
#28680 = DIRECTION ( 'NONE',  ( -0.000000000000000000, 1.000000000000000000, 0.000000000000000000 ) ) ;
#28681 = EDGE_CURVE ( 'NONE', #29172, #16166, #415, .T. ) ;
#28682 = DIRECTION ( 'NONE',  ( -0.000000000000000000, -0.000000000000000000, -1.000000000000000000 ) ) ;
#28683 = DIRECTION ( 'NONE',  ( 0.000000000000000000, 0.000000000000000000, -1.000000000000000000 ) ) ;
#28684 = ADVANCED_FACE ( 'NONE', ( #44904 ), #36767, .T. ) ;
#28685 = CARTESIAN_POINT ( 'NONE',  ( 194.9999999999999432, 173.0000000000000000, 132.0000000000000000 ) ) ;
#28686 = LINE ( 'NONE', #13530, #22373 ) ;
#28687 = CARTESIAN_POINT ( 'NONE',  ( 169.0000000000000284, 165.0000000000000000, 343.9999999999998863 ) ) ;
#28688 = EDGE_CURVE ( 'NONE', #48047, #35576, #17981, .T. ) ;
#28689 = VECTOR ( 'NONE', #49292, 1000.000000000000000 ) ;
#28690 = DIRECTION ( 'NONE',  ( 1.000000000000000000, 0.000000000000000000, 0.000000000000000000 ) ) ;
#28691 = UNCERTAINTY_MEASURE_WITH_UNIT (LENGTH_MEASURE( 1.000000000000000082E-05 ), #22748, 'distance_accuracy_value', 'NONE');
#28692 = VECTOR ( 'NONE', #10898, 1000.000000000000000 ) ;
#28693 = VECTOR ( 'NONE', #17574, 1000.000000000000000 ) ;
#28694 = CARTESIAN_POINT ( 'NONE',  ( 191.5540265531851105, 0.000000000000000000, 159.0682875569279702 ) ) ;
#28695 = ORIENTED_EDGE ( 'NONE', *, *, #33122, .T. ) ;
#28696 = CIRCLE ( 'NONE', #32007, 4.000000000000003553 ) ;
#28697 = DIRECTION ( 'NONE',  ( -1.000000000000000000, -0.000000000000000000, -0.000000000000000000 ) ) ;
#28698 =( GEOMETRIC_REPRESENTATION_CONTEXT ( 3 ) GLOBAL_UNCERTAINTY_ASSIGNED_CONTEXT ( ( #42772 ) ) GLOBAL_UNIT_ASSIGNED_CONTEXT ( ( #21041, #22296, #46109 ) ) REPRESENTATION_CONTEXT ( 'NONE', 'WORKASPACE' ) );
#28699 = CARTESIAN_POINT ( 'NONE',  ( -40.00000000000000000, 0.000000000000000000, 897.6604670114603550 ) ) ;
#28700 = CARTESIAN_POINT ( 'NONE',  ( 166.9999999999999716, -180.9999999999999716, -350.0000000000001705 ) ) ;
#28701 = CARTESIAN_POINT ( 'NONE',  ( -164.9459734468149463, 2.143131898507880377E-16, 159.0682875569279702 ) ) ;
#28702 = EDGE_CURVE ( 'NONE', #2436, #11997, #5637, .T. ) ;
#28703 = VECTOR ( 'NONE', #45094, 1000.000000000000114 ) ;
#28704 = ORIENTED_EDGE ( 'NONE', *, *, #18249, .F. ) ;
#28705 = FACE_OUTER_BOUND ( 'NONE', #40679, .T. ) ;
#28706 = CARTESIAN_POINT ( 'NONE',  ( -47.72109971266203132, 1.750000000000009548, -160.2068387089191219 ) ) ;
#28707 = ADVANCED_FACE ( 'NONE', ( #13382 ), #48493, .T. ) ;
#28708 = ORIENTED_EDGE ( 'NONE', *, *, #15297, .F. ) ;
#28709 = CARTESIAN_POINT ( 'NONE',  ( 0.3862712429686727678, 1.188820645368945605, 10.00000000000000000 ) ) ;
#28710 = CARTESIAN_POINT ( 'NONE',  ( 25.63461350838963071, -43.17876197216376255, -8.016098858316205167 ) ) ;
#28711 = CARTESIAN_POINT ( 'NONE',  ( -47.72109971266203132, 1.750000000000009326, 1.843413822775066269 ) ) ;
#28712 = VERTEX_POINT ( 'NONE', #25701 ) ;
#28713 = CARTESIAN_POINT ( 'NONE',  ( -194.9999999999999432, 164.9999999999999716, 500.0000000000000000 ) ) ;
#28714 = ORIENTED_EDGE ( 'NONE', *, *, #9041, .F. ) ;
#28715 = EDGE_LOOP ( 'NONE', ( #48715, #45222, #48757, #9548, #12508 ) ) ;
#28716 =( BOUNDED_CURVE ( )  B_SPLINE_CURVE ( 3, ( #48599, #4779, #954, #20691 ),
 .UNSPECIFIED., .F., .F. ) 
 B_SPLINE_CURVE_WITH_KNOTS ( ( 4, 4 ),
 ( 1.570796326794899667, 1.795031077903997518 ),
 .UNSPECIFIED. ) 
 CURVE ( )  GEOMETRIC_REPRESENTATION_ITEM ( )  RATIONAL_B_SPLINE_CURVE ( ( 1.000000000000000000, 0.9958142854328206894, 0.9958142854328206894, 1.000000000000000000 ) ) 
 REPRESENTATION_ITEM ( '' )  );
#28717 = ADVANCED_FACE ( 'NONE', ( #21857 ), #21082, .T. ) ;
#28718 = ADVANCED_FACE ( 'NONE', ( #41597 ), #1349, .F. ) ;
#28719 = ORIENTED_EDGE ( 'NONE', *, *, #24034, .F. ) ;
#28720 = DIRECTION ( 'NONE',  ( -1.000000000000000000, 0.000000000000000000, -2.958228394578794270E-31 ) ) ;
#28721 = CARTESIAN_POINT ( 'NONE',  ( -4.945973446814916130, -1.025126265847097429, -80.93171244307204404 ) ) ;
#28722 = ORIENTED_EDGE ( 'NONE', *, *, #338, .F. ) ;
#28723 = DIRECTION ( 'NONE',  ( -1.000000000000000000, -0.000000000000000000, -0.000000000000000000 ) ) ;
#28724 = CARTESIAN_POINT ( 'NONE',  ( 168.9999999999999716, -270.4999999999999432, -349.9999999999999432 ) ) ;
#28725 = EDGE_CURVE ( 'NONE', #16599, #19221, #33655, .T. ) ;
#28726 = FACE_OUTER_BOUND ( 'NONE', #5921, .T. ) ;
#28727 =( BOUNDED_CURVE ( )  B_SPLINE_CURVE ( 3, ( #22330, #22587, #41586, #38270 ),
 .UNSPECIFIED., .F., .F. ) 
 B_SPLINE_CURVE_WITH_KNOTS ( ( 4, 4 ),
 ( 1.570796326794896558, 3.141592653589793116 ),
 .UNSPECIFIED. ) 
 CURVE ( )  GEOMETRIC_REPRESENTATION_ITEM ( )  RATIONAL_B_SPLINE_CURVE ( ( 1.000000000000000000, 0.8047378541243649375, 0.8047378541243649375, 1.000000000000000000 ) ) 
 REPRESENTATION_ITEM ( '' )  );
#28728 = EDGE_CURVE ( 'NONE', #14882, #42480, #10892, .T. ) ;
#28729 = PLANE ( 'NONE',  #34190 ) ;
#28730 = VERTEX_POINT ( 'NONE', #32909 ) ;
#28731 = EDGE_CURVE ( 'NONE', #3643, #19789, #29041, .T. ) ;
#28732 = CARTESIAN_POINT ( 'NONE',  ( 191.5540265531851105, 0.000000000000000000, 42.56828755692798438 ) ) ;
#28733 = AXIS2_PLACEMENT_3D ( 'NONE', #26995, #23411, #3647 ) ;
#28734 = ORIENTED_EDGE ( 'NONE', *, *, #3891, .T. ) ;
#28735 = LINE ( 'NONE', #33597, #584 ) ;
#28736 = DIRECTION ( 'NONE',  ( -3.172065784643302499E-16, -1.000000000000000000, 2.537652627714642000E-15 ) ) ;
#28737 = VERTEX_POINT ( 'NONE', #40835 ) ;
#28738 = ORIENTED_EDGE ( 'NONE', *, *, #41507, .T. ) ;
#28739 = ORIENTED_EDGE ( 'NONE', *, *, #22995, .F. ) ;
#28740 = DIRECTION ( 'NONE',  ( 0.000000000000000000, 0.000000000000000000, 1.000000000000000000 ) ) ;
#28741 = VECTOR ( 'NONE', #26722, 1000.000000000000000 ) ;
#28742 = DIRECTION ( 'NONE',  ( 1.000000000000000000, 0.000000000000000000, 0.000000000000000000 ) ) ;
#28743 = VECTOR ( 'NONE', #48714, 1000.000000000000000 ) ;
#28744 = ORIENTED_EDGE ( 'NONE', *, *, #23501, .T. ) ;
#28745 = FACE_OUTER_BOUND ( 'NONE', #3187, .T. ) ;
#28746 = CARTESIAN_POINT ( 'NONE',  ( 0.000000000000000000, 167.0000000000000000, -344.0000000000001705 ) ) ;
#28747 = CARTESIAN_POINT ( 'NONE',  ( -208.4459734468149463, 0.000000000000000000, -157.4317124430720582 ) ) ;
#28748 = EDGE_CURVE ( 'NONE', #28277, #24712, #12001, .T. ) ;
#28749 = ORIENTED_EDGE ( 'NONE', *, *, #23703, .F. ) ;
#28750 = CARTESIAN_POINT ( 'NONE',  ( -44.94597344681493922, 1.025126265847089657, 119.0682875569279560 ) ) ;
#28751 = CARTESIAN_POINT ( 'NONE',  ( -88.44597344681497475, 0.000000000000000000, -80.93171244307204404 ) ) ;
#28752 = PLANE ( 'NONE',  #18260 ) ;
#28753 = ORIENTED_EDGE ( 'NONE', *, *, #26501, .T. ) ;
#28754 = ORIENTED_EDGE ( 'NONE', *, *, #28081, .T. ) ;
#28755 = CARTESIAN_POINT ( 'NONE',  ( -1.011271242968687867, 0.7347315653655861478, 9.972675548442463622 ) ) ;
#28756 = DIRECTION ( 'NONE',  ( 0.000000000000000000, -1.000000000000000000, 0.000000000000000000 ) ) ;
#28757 = CARTESIAN_POINT ( 'NONE',  ( 9.358026734184097251, 0.000000000000000000, -5.000000000000000000 ) ) ;
#28758 = DIRECTION ( 'NONE',  ( 0.000000000000000000, 0.000000000000000000, 1.000000000000000000 ) ) ;
#28759 = ORIENTED_EDGE ( 'NONE', *, *, #12214, .T. ) ;
#28760 = DIRECTION ( 'NONE',  ( 1.000000000000000000, 0.000000000000000000, 0.000000000000000000 ) ) ;
#28761 = EDGE_CURVE ( 'NONE', #10360, #45145, #18032, .T. ) ;
#28762 = CARTESIAN_POINT ( 'NONE',  ( 9.907356528111447957, -1.358045148324435347, 0.000000000000000000 ) ) ;
#28763 = CARTESIAN_POINT ( 'NONE',  ( -85.67084718096784002, 1.750000000000010214, 79.79316129108087807 ) ) ;
#28764 = DIRECTION ( 'NONE',  ( -0.000000000000000000, -0.000000000000000000, -1.000000000000000000 ) ) ;
#28765 = AXIS2_PLACEMENT_3D ( 'NONE', #15221, #11361, #26507 ) ;
#28766 = ORIENTED_EDGE ( 'NONE', *, *, #13644, .T. ) ;
#28767 = CARTESIAN_POINT ( 'NONE',  ( 210.0000000000000568, 0.000000000000000000, 42.56828755692799149 ) ) ;
#28768 = ORIENTED_EDGE ( 'NONE', *, *, #14278, .T. ) ;
#28769 = CARTESIAN_POINT ( 'NONE',  ( 25.61277432017878297, -22.36370378792834757, 7.906207997025717304 ) ) ;
#28770 = ORIENTED_EDGE ( 'NONE', *, *, #31005, .F. ) ;
#28771 = CARTESIAN_POINT ( 'NONE',  ( 168.9999999999999716, -256.5000000000000000, -114.9999999999999574 ) ) ;
#28772 = CARTESIAN_POINT ( 'NONE',  ( 15.00000000000000000, 8.875661936878623592, 18.94832733001756253 ) ) ;
#28773 = VECTOR ( 'NONE', #30406, 1000.000000000000000 ) ;
#28774 = CARTESIAN_POINT ( 'NONE',  ( -37.50000000000000000, 0.000000000000000000, -10.00000000000000000 ) ) ;
#28775 = ORIENTED_EDGE ( 'NONE', *, *, #45637, .F. ) ;
#28776 = ADVANCED_FACE ( 'NONE', ( #38018 ), #23102, .T. ) ;
#28777 = CARTESIAN_POINT ( 'NONE',  ( -164.4973046169135955, 53.53801056904001854, -17.65743994998277699 ) ) ;
#28778 = EDGE_CURVE ( 'NONE', #21304, #1914, #35804, .T. ) ;
#28779 = ORIENTED_EDGE ( 'NONE', *, *, #8948, .T. ) ;
#28780 = CARTESIAN_POINT ( 'NONE',  ( 0.9925179869589159098, 0.000000000000000000, 14.00000000000000355 ) ) ;
#28781 = DIRECTION ( 'NONE',  ( -1.000000000000000000, 0.000000000000000000, 0.000000000000000000 ) ) ;
#28782 = CARTESIAN_POINT ( 'NONE',  ( -0.1287570809895576818, -0.3962735484563154609, 10.00000000000000000 ) ) ;
#28783 = CARTESIAN_POINT ( 'NONE',  ( 166.9999999999999716, -164.9999999999999432, -344.0000000000001137 ) ) ;
#28784 = EDGE_CURVE ( 'NONE', #29991, #3878, #23014, .T. ) ;
#28785 = FACE_OUTER_BOUND ( 'NONE', #17287, .T. ) ;
#28786 = ORIENTED_EDGE ( 'NONE', *, *, #21086, .F. ) ;
#28787 = EDGE_CURVE ( 'NONE', #16006, #41417, #30821, .T. ) ;
#28788 = ORIENTED_EDGE ( 'NONE', *, *, #29928, .T. ) ;
#28789 = CARTESIAN_POINT ( 'NONE',  ( 3.566525152641073504, -1.569997364302916809, 9.741991644047246268 ) ) ;
#28790 = EDGE_CURVE ( 'NONE', #46654, #50635, #26955, .T. ) ;
#28791 = EDGE_CURVE ( 'NONE', #1717, #24673, #7474, .T. ) ;
#28792 = ORIENTED_EDGE ( 'NONE', *, *, #26859, .F. ) ;
#28793 = CARTESIAN_POINT ( 'NONE',  ( 168.9999999999999716, -184.9999999999999716, -356.0000000000001705 ) ) ;
#28794 = CARTESIAN_POINT ( 'NONE',  ( -10.49999999999999467, -46.51315789473684248, -6.315789473684215949 ) ) ;
#28795 = CARTESIAN_POINT ( 'NONE',  ( 2.500000000000000444, 224.9999999999999716, -224.9999999999999716 ) ) ;
#28796 = ORIENTED_EDGE ( 'NONE', *, *, #12158, .F. ) ;
#28797 = FACE_OUTER_BOUND ( 'NONE', #39563, .T. ) ;
#28798 = VECTOR ( 'NONE', #7539, 1000.000000000000000 ) ;
#28799 = EDGE_CURVE ( 'NONE', #42832, #29402, #30561, .T. ) ;
#28800 = DIRECTION ( 'NONE',  ( -0.000000000000000000, -1.000000000000000000, 2.537652627714643577E-15 ) ) ;
#28801 = PLANE ( 'NONE',  #14510 ) ;
#28802 = CARTESIAN_POINT ( 'NONE',  ( 35.00000000000152767, 17.00000000000000000, 60.00000000000000000 ) ) ;
#28803 = VECTOR ( 'NONE', #1494, 1000.000000000000000 ) ;
#28804 = FACE_BOUND ( 'NONE', #25060, .T. ) ;
#28805 = DIRECTION ( 'NONE',  ( -1.000000000000000000, -0.000000000000000000, -0.000000000000000000 ) ) ;
#28806 = ORIENTED_EDGE ( 'NONE', *, *, #29577, .F. ) ;
#28807 = ORIENTED_EDGE ( 'NONE', *, *, #27525, .F. ) ;
#28808 = VERTEX_POINT ( 'NONE', #50250 ) ;
#28809 = DIRECTION ( 'NONE',  ( 0.000000000000000000, 0.000000000000000000, -1.000000000000000000 ) ) ;
#28810 = DIRECTION ( 'NONE',  ( -6.938893903907227392E-16, 1.000000000000000000, 0.000000000000000000 ) ) ;
#28811 = LINE ( 'NONE', #43941, #35571 ) ;
#28812 = VECTOR ( 'NONE', #16781, 1000.000000000000000 ) ;
#28813 = VERTEX_POINT ( 'NONE', #49501 ) ;
#28814 = CARTESIAN_POINT ( 'NONE',  ( 30.00000000000153833, 16.00000000000000000, 35.00000000000000000 ) ) ;
#28815 = ORIENTED_EDGE ( 'NONE', *, *, #16786, .T. ) ;
#28816 = CARTESIAN_POINT ( 'NONE',  ( -7.576114424932982594, 33.14742743729794938, 7.906207997025717304 ) ) ;
#28817 = LINE ( 'NONE', #24976, #46523 ) ;
#28818 = FACE_OUTER_BOUND ( 'NONE', #12388, .T. ) ;
#28819 = FACE_OUTER_BOUND ( 'NONE', #35178, .T. ) ;
#28820 = PLANE ( 'NONE',  #3641 ) ;
#28821 = LINE ( 'NONE', #40867, #38735 ) ;
#28822 = ORIENTED_EDGE ( 'NONE', *, *, #8634, .T. ) ;
#28823 = CARTESIAN_POINT ( 'NONE',  ( 210.0000000000000568, 0.000000000000000000, -119.1817124430720440 ) ) ;
#28824 = DIRECTION ( 'NONE',  ( 0.000000000000000000, 0.000000000000000000, 1.000000000000000000 ) ) ;
#28825 = FACE_OUTER_BOUND ( 'NONE', #18105, .T. ) ;
#28826 = EDGE_CURVE ( 'NONE', #14950, #41788, #26205, .T. ) ;
#28827 = DIRECTION ( 'NONE',  ( 0.000000000000000000, -1.000000000000000000, 0.000000000000000000 ) ) ;
#28828 = ORIENTED_EDGE ( 'NONE', *, *, #45075, .F. ) ;
#28829 = CYLINDRICAL_SURFACE ( 'NONE', #14691, 2.000000000000001776 ) ;
#28830 = ORIENTED_EDGE ( 'NONE', *, *, #2693, .F. ) ;
#28831 = DIRECTION ( 'NONE',  ( 1.000000000000000000, -0.000000000000000000, -0.000000000000000000 ) ) ;
#28832 = VECTOR ( 'NONE', #36204, 1000.000000000000000 ) ;
#28833 = DIRECTION ( 'NONE',  ( -0.000000000000000000, -1.000000000000000000, -0.000000000000000000 ) ) ;
#28834 = CARTESIAN_POINT ( 'NONE',  ( -44.94597344681493922, 2.143131898507880377E-16, -117.4317124430720156 ) ) ;
#28835 = ORIENTED_EDGE ( 'NONE', *, *, #35539, .T. ) ;
#28836 = EDGE_CURVE ( 'NONE', #5029, #43960, #17708, .T. ) ;
#28837 = VECTOR ( 'NONE', #17275, 1000.000000000000000 ) ;
#28838 = CARTESIAN_POINT ( 'NONE',  ( 46.33529284216721322, -19.19803090445725502, -8.466730184410787174 ) ) ;
#28839 = DIRECTION ( 'NONE',  ( -1.000000000000000000, 0.000000000000000000, 0.000000000000000000 ) ) ;
#28840 = FACE_OUTER_BOUND ( 'NONE', #34958, .T. ) ;
#28841 = CARTESIAN_POINT ( 'NONE',  ( 34.08355720199905647, -2.371364769369109116, 7.455576670931136185 ) ) ;
#28842 = EDGE_LOOP ( 'NONE', ( #11326, #40909, #5682, #16495 ) ) ;
#28843 = ORIENTED_EDGE ( 'NONE', *, *, #44165, .F. ) ;
#28844 = LINE ( 'NONE', #13443, #24266 ) ;
#28845 = CARTESIAN_POINT ( 'NONE',  ( 1.249999999999999778, 0.000000000000000000, 10.00000000000000000 ) ) ;
#28846 = EDGE_CURVE ( 'NONE', #33857, #5897, #31510, .T. ) ;
#28847 = EDGE_CURVE ( 'NONE', #13654, #25400, #2833, .T. ) ;
#28848 = ORIENTED_EDGE ( 'NONE', *, *, #5933, .T. ) ;
#28849 = EDGE_LOOP ( 'NONE', ( #5861, #33580, #46739, #31662 ) ) ;
#28850 = CARTESIAN_POINT ( 'NONE',  ( 228.9999999999999716, -169.9999999999999716, 32.29650858650035161 ) ) ;
#28851 = CARTESIAN_POINT ( 'NONE',  ( 181.0000000000000284, -174.9999999999999716, -115.0000000000001563 ) ) ;
#28852 = DIRECTION ( 'NONE',  ( 1.000000000000000000, 0.000000000000000000, 0.000000000000000000 ) ) ;
#28853 = DIRECTION ( 'NONE',  ( 0.000000000000000000, 0.000000000000000000, -1.000000000000000000 ) ) ;
#28854 = ORIENTED_EDGE ( 'NONE', *, *, #42364, .F. ) ;
#28855 = VERTEX_POINT ( 'NONE', #2583 ) ;
#28856 = EDGE_CURVE ( 'NONE', #21132, #29819, #16140, .T. ) ;
#28857 = ORIENTED_EDGE ( 'NONE', *, *, #46352, .T. ) ;
#28858 = CARTESIAN_POINT ( 'NONE',  ( -215.0000000000000568, -175.0000000000000000, 500.0000000000000000 ) ) ;
#28859 =( BOUNDED_CURVE ( )  B_SPLINE_CURVE ( 3, ( #3546, #34884, #37295, #38234 ),
 .UNSPECIFIED., .F., .F. ) 
 B_SPLINE_CURVE_WITH_KNOTS ( ( 4, 4 ),
 ( 3.141592653589793116, 4.712388980384689674 ),
 .UNSPECIFIED. ) 
 CURVE ( )  GEOMETRIC_REPRESENTATION_ITEM ( )  RATIONAL_B_SPLINE_CURVE ( ( 1.000000000000000000, 0.8047378541243649375, 0.8047378541243649375, 1.000000000000000000 ) ) 
 REPRESENTATION_ITEM ( '' )  );
#28860 = DIRECTION ( 'NONE',  ( 0.000000000000000000, -1.000000000000000000, 0.000000000000000000 ) ) ;
#28861 = CARTESIAN_POINT ( 'NONE',  ( 1.011271242968683648, 0.7347315653655930312, 10.00000000000000000 ) ) ;
#28862 = ORIENTED_EDGE ( 'NONE', *, *, #464, .T. ) ;
#28863 = VECTOR ( 'NONE', #18875, 1000.000000000000000 ) ;
#28864 = VERTEX_POINT ( 'NONE', #18493 ) ;
#28866 = CARTESIAN_POINT ( 'NONE',  ( -8.445973446814976526, 0.000000000000000000, -77.43171244307198720 ) ) ;
#28865 =( BOUNDED_CURVE ( )  B_SPLINE_CURVE ( 3, ( #17829, #10132, #22194, #34509 ),
 .UNSPECIFIED., .F., .F. ) 
 B_SPLINE_CURVE_WITH_KNOTS ( ( 4, 4 ),
 ( 0.000000000000000000, 1.570796326794896558 ),
 .UNSPECIFIED. ) 
 CURVE ( )  GEOMETRIC_REPRESENTATION_ITEM ( )  RATIONAL_B_SPLINE_CURVE ( ( 1.000000000000000000, 0.8047378541243649375, 0.8047378541243649375, 1.000000000000000000 ) ) 
 REPRESENTATION_ITEM ( '' )  );
#28867 = AXIS2_PLACEMENT_3D ( 'NONE', #2362, #48511, #45428 ) ;
#28868 = DIRECTION ( 'NONE',  ( -0.5407575913134976542, 0.000000000000000000, -0.8411784753765542133 ) ) ;
#28869 = EDGE_LOOP ( 'NONE', ( #9981, #22652, #19330, #9986, #47109, #31673 ) ) ;
#28870 = EDGE_LOOP ( 'NONE', ( #45984, #37066, #12808, #23446 ) ) ;
#28871 = VECTOR ( 'NONE', #30402, 1000.000000000000000 ) ;
#28872 = CARTESIAN_POINT ( 'NONE',  ( 50.11058929355270664, -7.578863168071591438, 7.455576670931136185 ) ) ;
#28873 = DIRECTION ( 'NONE',  ( -0.000000000000000000, -0.000000000000000000, -1.000000000000000000 ) ) ;
#28874 = ORIENTED_EDGE ( 'NONE', *, *, #8016, .T. ) ;
#28875 = DIRECTION ( 'NONE',  ( -0.9928768384869219865, 0.000000000000000000, -0.1191452206184307749 ) ) ;
#28876 = CARTESIAN_POINT ( 'NONE',  ( 183.0000000000000284, -174.9999999999999716, -99.00000000000014211 ) ) ;
#28877 = PLANE ( 'NONE',  #29416 ) ;
#28878 = VECTOR ( 'NONE', #42346, 1000.000000000000000 ) ;
#28879 = CARTESIAN_POINT ( 'NONE',  ( 31.84561714023325507, -33.32763979208104388, 8.807470649214879543 ) ) ;
#28880 = ORIENTED_EDGE ( 'NONE', *, *, #39850, .T. ) ;
#28881 = CARTESIAN_POINT ( 'NONE',  ( -17.23491422248386584, 0.5912720620001978844, 8.727788335465566760 ) ) ;
#28882 = CARTESIAN_POINT ( 'NONE',  ( 35.05402655318504657, 2.143131898507880377E-16, -117.4317124430720156 ) ) ;
#28883 =( BOUNDED_CURVE ( )  B_SPLINE_CURVE ( 3, ( #4933, #46543, #42229, #34811 ),
 .UNSPECIFIED., .F., .F. ) 
 B_SPLINE_CURVE_WITH_KNOTS ( ( 4, 4 ),
 ( 0.000000000000000000, 1.570796326794896558 ),
 .UNSPECIFIED. ) 
 CURVE ( )  GEOMETRIC_REPRESENTATION_ITEM ( )  RATIONAL_B_SPLINE_CURVE ( ( 1.000000000000000000, 0.8047378541243649375, 0.8047378541243649375, 1.000000000000000000 ) ) 
 REPRESENTATION_ITEM ( '' )  );
#28884 = B_SPLINE_SURFACE_WITH_KNOTS ( 'NONE', 3, 3, ( 
 ( #17970, #40587, #20822, #40830 ),
 ( #5676, #5425, #21578, #29036 ),
 ( #36505, #9035, #32640, #32902 ),
 ( #17741, #17483, #21332, #24691 ) ),
 .UNSPECIFIED., .F., .F., .F.,
 ( 4, 4 ),
 ( 4, 4 ),
 ( 0.000000000000000000, 1.000000000000000000 ),
 ( 0.000000000000000000, 1.000000000000000000 ),
 .UNSPECIFIED. ) ;
#28885 = CARTESIAN_POINT ( 'NONE',  ( -28.55116071645519327, 41.05976639056880373, -2.408242355805840784 ) ) ;
#28886 = FACE_OUTER_BOUND ( 'NONE', #20772, .T. ) ;
#28887 = EDGE_CURVE ( 'NONE', #41339, #38600, #18232, .T. ) ;
#28888 = CARTESIAN_POINT ( 'NONE',  ( 9.999999999999998224, -0.4417425667975402037, 5.558078895815850906 ) ) ;
#28889 = CARTESIAN_POINT ( 'NONE',  ( 168.9999999999999716, 6.000000000000060396, -350.0000000000001705 ) ) ;
#28890 = DIRECTION ( 'NONE',  ( -1.000000000000000000, 0.000000000000000000, 0.000000000000000000 ) ) ;
#28891 = AXIS2_PLACEMENT_3D ( 'NONE', #35561, #402, #16049 ) ;
#28892 = CARTESIAN_POINT ( 'NONE',  ( 191.5540265531851105, 0.000000000000000000, -80.93171244307201562 ) ) ;
#28893 = ORIENTED_EDGE ( 'NONE', *, *, #29341, .F. ) ;
#28894 = CARTESIAN_POINT ( 'NONE',  ( -5.888214538810513154, -16.20866436362413410, 8.727788335465566760 ) ) ;
#28895 = CARTESIAN_POINT ( 'NONE',  ( 343.9999999999999432, -183.0000000000002558, -358.0000000000003411 ) ) ;
#28896=STYLED_ITEM('',(#50754),#5787);
#28897 = CARTESIAN_POINT ( 'NONE',  ( -115.0000000000000284, 16.00000000000000000, -114.9999999999999858 ) ) ;
#28898 = CARTESIAN_POINT ( 'NONE',  ( 12.97493236725083676, -11.05939663306990717, 8.953103998512858652 ) ) ;
#28899 = CARTESIAN_POINT ( 'NONE',  ( 210.0000000000000568, 0.000000000000000000, 40.81828755692798438 ) ) ;
#28900 = AXIS2_PLACEMENT_3D ( 'NONE', #43133, #8000, #31610 ) ;
#28901 = ORIENTED_EDGE ( 'NONE', *, *, #723, .T. ) ;
#28902 = LINE ( 'NONE', #21442, #35598 ) ;
#28903 = ORIENTED_EDGE ( 'NONE', *, *, #13082, .F. ) ;
#28904 = LINE ( 'NONE', #44523, #10343 ) ;
#28905 = VECTOR ( 'NONE', #8455, 1000.000000000000000 ) ;
#28906 = DIRECTION ( 'NONE',  ( -0.000000000000000000, -0.000000000000000000, -1.000000000000000000 ) ) ;
#28907 = VERTEX_POINT ( 'NONE', #45916 ) ;
#28908 = VECTOR ( 'NONE', #37956, 1000.000000000000000 ) ;
#28909 = CARTESIAN_POINT ( 'NONE',  ( 55.00000000000002132, -52.50000000000000711, -5.000000000000000000 ) ) ;
#28910 = CARTESIAN_POINT ( 'NONE',  ( 210.0000000000000568, 0.000000000000000000, -157.4317124430720298 ) ) ;
#28911 = ORIENTED_EDGE ( 'NONE', *, *, #34999, .F. ) ;
#28912 = ORIENTED_EDGE ( 'NONE', *, *, #46065, .F. ) ;
#28913 = ADVANCED_FACE ( 'NONE', ( #3091 ), #18992, .F. ) ;
#28914 = B_SPLINE_CURVE_WITH_KNOTS ( 'NONE', 3,
 ( #29375, #9625, #25524, #27932 ),
 .UNSPECIFIED., .F., .F.,
 ( 4, 4 ),
 ( 0.000000000000000000, 0.009404495247862304161 ),
 .UNSPECIFIED. ) ;
#28915 = CARTESIAN_POINT ( 'NONE',  ( -8.277096487746778308, 50.00000000000000711, 7.455576670931136185 ) ) ;
#28916 = CARTESIAN_POINT ( 'NONE',  ( -28.52604530808686079, -41.07801380285659576, -3.760136334089591248 ) ) ;
#28917 = ORIENTED_EDGE ( 'NONE', *, *, #15005, .F. ) ;
#28918 = CARTESIAN_POINT ( 'NONE',  ( 115.0540265531850395, -1.025126265847081886, 79.06828755692797017 ) ) ;
#28919 = AXIS2_PLACEMENT_3D ( 'NONE', #27877, #34827, #35339 ) ;
#28920 = PLANE ( 'NONE',  #40933 ) ;
#28921 = ORIENTED_EDGE ( 'NONE', *, *, #44461, .F. ) ;
#28922 = ORIENTED_EDGE ( 'NONE', *, *, #30649, .T. ) ;
#28923 = EDGE_LOOP ( 'NONE', ( #25255, #40786, #5263, #9867 ) ) ;
#28924 = CARTESIAN_POINT ( 'NONE',  ( -204.9459734468148895, -1.025126265847089435, 122.5682875569280128 ) ) ;
#28925 = CARTESIAN_POINT ( 'NONE',  ( 341.9999999999999432, -182.1715728752539860, -357.1715728752541281 ) ) ;
#28926 = ORIENTED_EDGE ( 'NONE', *, *, #33383, .T. ) ;
#28927 = EDGE_CURVE ( 'NONE', #42445, #49554, #6953, .T. ) ;
#28928 = CARTESIAN_POINT ( 'NONE',  ( 151.5540265531850537, 1.025126265847089213, 42.56828755692799149 ) ) ;
#28929 = LINE ( 'NONE', #9930, #8395 ) ;
#28930 = DIRECTION ( 'NONE',  ( 0.000000000000000000, -0.9602398687205827565, -0.2791762785758810650 ) ) ;
#28931 = FACE_BOUND ( 'NONE', #359, .T. ) ;
#28932 = AXIS2_PLACEMENT_3D ( 'NONE', #23339, #3840, #23596 ) ;
#28933 = LINE ( 'NONE', #13526, #18347 ) ;
#28934 = CARTESIAN_POINT ( 'NONE',  ( -1.011271242968677875, -0.7347315653656004697, -3.333333333333333481 ) ) ;
#28935 = AXIS2_PLACEMENT_3D ( 'NONE', #19464, #39496, #16135 ) ;
#28936 = DIRECTION ( 'NONE',  ( 0.000000000000000000, -1.000000000000000000, 2.969158215481698263E-48 ) ) ;
#28937 = CARTESIAN_POINT ( 'NONE',  ( -88.44597344681497475, 0.000000000000000000, -157.4317124430720014 ) ) ;
#28938 = EDGE_CURVE ( 'NONE', #13304, #11040, #11053, .T. ) ;
#28939 = DIRECTION ( 'NONE',  ( 0.000000000000000000, -1.000000000000000000, 1.604368532695312981E-16 ) ) ;
#28940 = VECTOR ( 'NONE', #39448, 1000.000000000000000 ) ;
#28941 = CARTESIAN_POINT ( 'NONE',  ( -36.08557433729205144, 35.58569447144795816, 7.455576670931136185 ) ) ;
#28942 = ADVANCED_FACE ( 'NONE', ( #38530 ), #32339, .T. ) ;
#28943 = AXIS2_PLACEMENT_3D ( 'NONE', #39819, #12588, #7750 ) ;
#28944 = CARTESIAN_POINT ( 'NONE',  ( 1.011271242968683648, 0.7347315653655930312, -10.00000000000000000 ) ) ;
#28945 = ORIENTED_EDGE ( 'NONE', *, *, #47434, .F. ) ;
#28946 = PLANE ( 'NONE',  #12249 ) ;
#28947 = CARTESIAN_POINT ( 'NONE',  ( 358.0000000000000000, 169.0000000000001705, -344.0000000000002842 ) ) ;
#28948 = DIRECTION ( 'NONE',  ( 0.000000000000000000, 0.000000000000000000, -1.000000000000000000 ) ) ;
#28949 = VERTEX_POINT ( 'NONE', #16181 ) ;
#28950 = FACE_OUTER_BOUND ( 'NONE', #35418, .T. ) ;
#28951 = LINE ( 'NONE', #13041, #22092 ) ;
#28952 =( BOUNDED_CURVE ( )  B_SPLINE_CURVE ( 3, ( #4079, #32300, #31548, #12782 ),
 .UNSPECIFIED., .F., .F. ) 
 B_SPLINE_CURVE_WITH_KNOTS ( ( 4, 4 ),
 ( 0.000000000000000000, 1.570796326794896558 ),
 .UNSPECIFIED. ) 
 CURVE ( )  GEOMETRIC_REPRESENTATION_ITEM ( )  RATIONAL_B_SPLINE_CURVE ( ( 1.000000000000000000, 0.8047378541243649375, 0.8047378541243649375, 1.000000000000000000 ) ) 
 REPRESENTATION_ITEM ( '' )  );
#28953 = ORIENTED_EDGE ( 'NONE', *, *, #44640, .T. ) ;
#28954 = CARTESIAN_POINT ( 'NONE',  ( -45.67084718096785423, -1.750000000000009548, -118.1565861772249519 ) ) ;
#28955 = CARTESIAN_POINT ( 'NONE',  ( 151.5540265531850537, 0.000000000000000000, -120.9317124430720156 ) ) ;
#28956 = DIRECTION ( 'NONE',  ( 1.132880637372608740E-16, 4.718402560806925739E-50, 1.000000000000000000 ) ) ;
#28957 = ORIENTED_EDGE ( 'NONE', *, *, #11170, .F. ) ;
#28958 = FILL_AREA_STYLE_COLOUR ( '', #42919 ) ;
#28959 = EDGE_LOOP ( 'NONE', ( #31367, #15927 ) ) ;
#28960 = ORIENTED_EDGE ( 'NONE', *, *, #6840, .F. ) ;
#28961 = EDGE_CURVE ( 'NONE', #38646, #20559, #28283, .T. ) ;
#28962 = EDGE_CURVE ( 'NONE', #26731, #32176, #1031, .T. ) ;
#28963 = EDGE_LOOP ( 'NONE', ( #6351, #10459 ) ) ;
#28964 = CYLINDRICAL_SURFACE ( 'NONE', #28358, 0.5000000000000004441 ) ;
#28965 = FACE_OUTER_BOUND ( 'NONE', #38713, .T. ) ;
#28966 = CIRCLE ( 'NONE', #2733, 4.000000000000003553 ) ;
#28967 = ORIENTED_EDGE ( 'NONE', *, *, #14993, .T. ) ;
#28968 = CARTESIAN_POINT ( 'NONE',  ( 45.42829307628542779, 21.98948915213303579, 8.356839323120299312 ) ) ;
#28969 = ADVANCED_FACE ( 'NONE', ( #27972 ), #27474, .F. ) ;
#28970 = AXIS2_PLACEMENT_3D ( 'NONE', #25281, #28386, #44008 ) ;
#28971 = CARTESIAN_POINT ( 'NONE',  ( 113.3040265531850537, 0.000000000000000000, 165.0000000000000000 ) ) ;
#28972 = CARTESIAN_POINT ( 'NONE',  ( 0.5386300094813488704, -1.098626330213929636, 9.993783931180535873 ) ) ;
#28973 = ORIENTED_EDGE ( 'NONE', *, *, #41692, .F. ) ;
#28974 = VECTOR ( 'NONE', #28273, 1000.000000000000114 ) ;
#28975 = ADVANCED_FACE ( 'NONE', ( #4862 ), #8485, .T. ) ;
#28976 = DIRECTION ( 'NONE',  ( 0.000000000000000000, 1.000000000000000000, 0.000000000000000000 ) ) ;
#28977 = ORIENTED_EDGE ( 'NONE', *, *, #42773, .T. ) ;
#28978 = LINE ( 'NONE', #2037, #45582 ) ;
#28979 = FACE_OUTER_BOUND ( 'NONE', #26990, .T. ) ;
#28980 = ORIENTED_EDGE ( 'NONE', *, *, #31140, .T. ) ;
#28981 = ORIENTED_EDGE ( 'NONE', *, *, #34475, .T. ) ;
#28982 = ORIENTED_EDGE ( 'NONE', *, *, #33432, .T. ) ;
#28983 = DIRECTION ( 'NONE',  ( -0.000000000000000000, -1.000000000000000000, -0.000000000000000000 ) ) ;
#28984 = DIRECTION ( 'NONE',  ( -0.000000000000000000, -1.000000000000000000, -0.000000000000000000 ) ) ;
#28985 = B_SPLINE_SURFACE_WITH_KNOTS ( 'NONE', 3, 3, ( 
 ( #14932, #30332, #45944, #3369 ),
 ( #50279, #30851, #46445, #8511 ),
 ( #16202, #16455, #47959, #27748 ),
 ( #4398, #20046, #19524, #35212 ) ),
 .UNSPECIFIED., .F., .F., .F.,
 ( 4, 4 ),
 ( 4, 4 ),
 ( 0.000000000000000000, 1.000000000000000000 ),
 ( 0.000000000000000000, 1.000000000000000000 ),
 .UNSPECIFIED. ) ;
#28986 = ORIENTED_EDGE ( 'NONE', *, *, #25967, .F. ) ;
#28987 = DIRECTION ( 'NONE',  ( -0.000000000000000000, -0.000000000000000000, -1.000000000000000000 ) ) ;
#28988 = CARTESIAN_POINT ( 'NONE',  ( -69.99999999999909051, 17.00000000000000000, -24.99999999999999289 ) ) ;
#28989 = FACE_OUTER_BOUND ( 'NONE', #40465, .T. ) ;
#28990 = AXIS2_PLACEMENT_3D ( 'NONE', #43997, #48061, #32986 ) ;
#28991 = VERTEX_POINT ( 'NONE', #39032 ) ;
#28992 = LINE ( 'NONE', #44611, #8458 ) ;
#28993 = CARTESIAN_POINT ( 'NONE',  ( -0.2778388845795317086, 1.251314014313103851, 9.976582533991678048 ) ) ;
#28994 = DIRECTION ( 'NONE',  ( 0.000000000000000000, 0.000000000000000000, -1.000000000000000000 ) ) ;
#28995 = EDGE_CURVE ( 'NONE', #47564, #27344, #3862, .T. ) ;
#28996 = ORIENTED_EDGE ( 'NONE', *, *, #7999, .T. ) ;
#28997 = ADVANCED_FACE ( 'NONE', ( #31591 ), #35700, .T. ) ;
#28998 = ORIENTED_EDGE ( 'NONE', *, *, #17772, .F. ) ;
#28999 = PRODUCT_CONTEXT ( 'NONE', #5289, 'mechanical' ) ;
#29000 = DIRECTION ( 'NONE',  ( 0.000000000000000000, 0.000000000000000000, -1.000000000000000000 ) ) ;
#29001 = FACE_OUTER_BOUND ( 'NONE', #31573, .T. ) ;
#29002 = ADVANCED_FACE ( 'NONE', ( #20523 ), #46507, .T. ) ;
#29003 = EDGE_CURVE ( 'NONE', #13632, #37343, #26030, .T. ) ;
#29004 = AXIS2_PLACEMENT_3D ( 'NONE', #3594, #30813, #34929 ) ;
#29005 = VECTOR ( 'NONE', #3017, 1000.000000000000000 ) ;
#29006 = CARTESIAN_POINT ( 'NONE',  ( -29.18392875402943432, -17.44843138996582965, 7.906207997025717304 ) ) ;
#29007 = CARTESIAN_POINT ( 'NONE',  ( -166.6959734468149463, 1.750000000000010658, -119.1817124430720440 ) ) ;
#29008 = ORIENTED_EDGE ( 'NONE', *, *, #31226, .F. ) ;
#29009 = EDGE_CURVE ( 'NONE', #4194, #5590, #24391, .T. ) ;
#29010 = CARTESIAN_POINT ( 'NONE',  ( 33.14391172085757375, 37.72293746533118508, -8.016098858316205167 ) ) ;
#29011 = EDGE_CURVE ( 'NONE', #15143, #27194, #12077, .T. ) ;
#29012 = CARTESIAN_POINT ( 'NONE',  ( -16.02661358026017879, -4.530191650547607196, -9.683996418299976483 ) ) ;
#29013 = FACE_OUTER_BOUND ( 'NONE', #25077, .T. ) ;
#29014 = AXIS2_PLACEMENT_3D ( 'NONE', #29718, #13051, #33081 ) ;
#29015 = CARTESIAN_POINT ( 'NONE',  ( -165.0000000000000284, 17.00000000000000000, -114.9999999999999858 ) ) ;
#29016 =( BOUNDED_CURVE ( )  B_SPLINE_CURVE ( 3, ( #35725, #24414, #20789, #36472 ),
 .UNSPECIFIED., .F., .F. ) 
 B_SPLINE_CURVE_WITH_KNOTS ( ( 4, 4 ),
 ( 4.712388980384689674, 6.283185307179586232 ),
 .UNSPECIFIED. ) 
 CURVE ( )  GEOMETRIC_REPRESENTATION_ITEM ( )  RATIONAL_B_SPLINE_CURVE ( ( 1.000000000000000000, 0.8047378541243649375, 0.8047378541243649375, 1.000000000000000000 ) ) 
 REPRESENTATION_ITEM ( '' )  );
#29017 = VERTEX_POINT ( 'NONE', #8228 ) ;
#29018 = CARTESIAN_POINT ( 'NONE',  ( -207.2473046169136808, 159.2880105690400399, 472.5992458228020610 ) ) ;
#29019 = EDGE_LOOP ( 'NONE', ( #29232, #5864, #28670, #26597, #26933, #32597 ) ) ;
#29020 = FACE_OUTER_BOUND ( 'NONE', #7499, .T. ) ;
#29021 = ORIENTED_EDGE ( 'NONE', *, *, #3536, .F. ) ;
#29022 = CARTESIAN_POINT ( 'NONE',  ( 195.0540265531851105, -1.025126265847089657, -80.93171244307201562 ) ) ;
#29023 = CARTESIAN_POINT ( 'NONE',  ( 339.9999999999999432, -168.9999999999999432, 343.9999999999998295 ) ) ;
#29024 =( BOUNDED_CURVE ( )  B_SPLINE_CURVE ( 3, ( #46412, #31320, #11299, #7460 ),
 .UNSPECIFIED., .F., .F. ) 
 B_SPLINE_CURVE_WITH_KNOTS ( ( 4, 4 ),
 ( 1.570796326794896558, 3.141592653589793116 ),
 .UNSPECIFIED. ) 
 CURVE ( )  GEOMETRIC_REPRESENTATION_ITEM ( )  RATIONAL_B_SPLINE_CURVE ( ( 1.000000000000000000, 0.8047378541243649375, 0.8047378541243649375, 1.000000000000000000 ) ) 
 REPRESENTATION_ITEM ( '' )  );
#29025 = EDGE_CURVE ( 'NONE', #14767, #6739, #12235, .T. ) ;
#29026 = ORIENTED_EDGE ( 'NONE', *, *, #13651, .F. ) ;
#29027 = AXIS2_PLACEMENT_3D ( 'NONE', #3549, #25462, #26910 ) ;
#29028 = EDGE_CURVE ( 'NONE', #5747, #48314, #20276, .T. ) ;
#29029 = CARTESIAN_POINT ( 'NONE',  ( 210.0000000000000568, 0.000000000000000000, -119.1817124430720440 ) ) ;
#29030 = EDGE_CURVE ( 'NONE', #4778, #16264, #44356, .T. ) ;
#29031 = ORIENTED_EDGE ( 'NONE', *, *, #33777, .F. ) ;
#29032 = CARTESIAN_POINT ( 'NONE',  ( -114.9999999999987779, 17.00000000000000000, 30.00000000000000000 ) ) ;
#29033 = DIRECTION ( 'NONE',  ( -1.000000000000000000, 0.000000000000000000, 0.000000000000000000 ) ) ;
#29034 = CARTESIAN_POINT ( 'NONE',  ( 49.67735855322978011, -8.912210285361751971, 8.356839323120299312 ) ) ;
#29035 = LINE ( 'NONE', #21849, #14371 ) ;
#29036 = CARTESIAN_POINT ( 'NONE',  ( -0.3862712429686977478, 1.188820645368937390, 3.333333333333333481 ) ) ;
#29037 = ORIENTED_EDGE ( 'NONE', *, *, #9100, .F. ) ;
#29038 = ORIENTED_EDGE ( 'NONE', *, *, #24678, .F. ) ;
#29039 = DIRECTION ( 'NONE',  ( 0.000000000000000000, 0.000000000000000000, 1.000000000000000000 ) ) ;
#29040 = ORIENTED_EDGE ( 'NONE', *, *, #12422, .F. ) ;
#29041 = LINE ( 'NONE', #17492, #32493 ) ;
#29042 = VECTOR ( 'NONE', #10102, 1000.000000000000000 ) ;
#29043 = CARTESIAN_POINT ( 'NONE',  ( 356.0000000000000568, -185.0000000000001421, 360.0000000000000000 ) ) ;
#29044 = VERTEX_POINT ( 'NONE', #41280 ) ;
#29045 = CARTESIAN_POINT ( 'NONE',  ( 0.000000000000000000, 0.000000000000000000, 0.000000000000000000 ) ) ;
#29046 = VECTOR ( 'NONE', #38059, 1000.000000000000000 ) ;
#29047 = ADVANCED_FACE ( 'NONE', ( #36717 ), #17683, .T. ) ;
#29048 = DIRECTION ( 'NONE',  ( 1.000000000000000000, 0.000000000000000000, 7.793956916774525800E-48 ) ) ;
#29049 = ORIENTED_EDGE ( 'NONE', *, *, #21139, .F. ) ;
#29050 = AXIS2_PLACEMENT_3D ( 'NONE', #5693, #17253, #36520 ) ;
#29051 = CARTESIAN_POINT ( 'NONE',  ( 8.277096487746778308, -50.00000000000000711, 7.455576670931136185 ) ) ;
#29052 = CYLINDRICAL_SURFACE ( 'NONE', #17710, 1.750000000000015543 ) ;
#29053 = DIRECTION ( 'NONE',  ( 0.000000000000000000, 1.000000000000000000, -2.406552799042969348E-16 ) ) ;
#29054 = CARTESIAN_POINT ( 'NONE',  ( -86.69597344681496054, 0.000000000000000000, 165.0000000000000000 ) ) ;
#29055 = VERTEX_POINT ( 'NONE', #21276 ) ;
#29056 = ORIENTED_EDGE ( 'NONE', *, *, #27093, .F. ) ;
#29057 = ADVANCED_FACE ( 'NONE', ( #48929 ), #8981, .F. ) ;
#29058 = ORIENTED_EDGE ( 'NONE', *, *, #42506, .F. ) ;
#29059 = CARTESIAN_POINT ( 'NONE',  ( -5.083187235775261215, -8.611690166631138510, 9.646707543097347681 ) ) ;
#29060 = CARTESIAN_POINT ( 'NONE',  ( 15.98719783915691650, -4.501063718205879916, 3.266473740018926541 ) ) ;
#29061 = DIRECTION ( 'NONE',  ( -0.000000000000000000, -1.000000000000000000, -0.000000000000000000 ) ) ;
#29062 = CARTESIAN_POINT ( 'NONE',  ( 71.55402655318505367, -1.025126265847089435, 2.568287556927986159 ) ) ;
#29063 = ORIENTED_EDGE ( 'NONE', *, *, #27717, .F. ) ;
#29064 = CARTESIAN_POINT ( 'NONE',  ( 343.9999999999999432, -165.0000000000001137, -340.0000000000002842 ) ) ;
#29065 = EDGE_LOOP ( 'NONE', ( #14643, #40273, #6063, #29812, #14115, #20255 ) ) ;
#29066 = LINE ( 'NONE', #12900, #7302 ) ;
#29067 = LINE ( 'NONE', #44691, #22788 ) ;
#29068 = DIRECTION ( 'NONE',  ( 4.758098676964956461E-16, 1.000000000000000000, 0.000000000000000000 ) ) ;
#29069 = EDGE_CURVE ( 'NONE', #38138, #43962, #44850, .T. ) ;
#29070 = VECTOR ( 'NONE', #28616, 1000.000000000000000 ) ;
#29071 = EDGE_CURVE ( 'NONE', #1528, #28645, #37463, .T. ) ;
#29072 = CYLINDRICAL_SURFACE ( 'NONE', #47931, 1.750000000000015543 ) ;
#29073 = CARTESIAN_POINT ( 'NONE',  ( -44.94597344681493922, -1.025126265847089657, 119.0682875569279560 ) ) ;
#29074 = AXIS2_PLACEMENT_3D ( 'NONE', #14104, #41567, #37739 ) ;
#29075 = LINE ( 'NONE', #44695, #46887 ) ;
#29076 = ORIENTED_EDGE ( 'NONE', *, *, #27734, .F. ) ;
#29077 = CARTESIAN_POINT ( 'NONE',  ( 195.0540265531851105, 2.143131898507880377E-16, -40.93171244307202983 ) ) ;
#29078 = EDGE_CURVE ( 'NONE', #48234, #38333, #16941, .T. ) ;
#29079 = DIRECTION ( 'NONE',  ( -0.000000000000000000, -1.000000000000000000, -0.000000000000000000 ) ) ;
#29080 = DIRECTION ( 'NONE',  ( 1.333906992743555050E-23, -1.000000000000000000, 0.000000000000000000 ) ) ;
#29081 = EDGE_CURVE ( 'NONE', #15483, #44977, #32594, .T. ) ;
#29082 = EDGE_CURVE ( 'NONE', #9162, #16655, #2280, .T. ) ;
#29083 = FACE_OUTER_BOUND ( 'NONE', #48117, .T. ) ;
#29084 = ORIENTED_EDGE ( 'NONE', *, *, #49281, .F. ) ;
#29085 = AXIS2_PLACEMENT_3D ( 'NONE', #7404, #38461, #42288 ) ;
#29086 = DIRECTION ( 'NONE',  ( 0.000000000000000000, 0.000000000000000000, 1.000000000000000000 ) ) ;
#29087 = ORIENTED_EDGE ( 'NONE', *, *, #35637, .T. ) ;
#29088 = CARTESIAN_POINT ( 'NONE',  ( -46.69597344681494633, 1.750000000000010658, 80.81828755692798438 ) ) ;
#29089 = DIRECTION ( 'NONE',  ( -1.000000000000000000, -0.000000000000000000, -0.000000000000000000 ) ) ;
#29090 = EDGE_CURVE ( 'NONE', #2228, #46883, #25962, .T. ) ;
#29091 = DIRECTION ( 'NONE',  ( 6.765175596986472868E-16, -0.9749645535258953943, 0.2223603367690637489 ) ) ;
#29092 = VECTOR ( 'NONE', #16126, 1000.000000000000000 ) ;
#29093 = ORIENTED_EDGE ( 'NONE', *, *, #48983, .T. ) ;
#29094 = ORIENTED_EDGE ( 'NONE', *, *, #15768, .T. ) ;
#29095 = FACE_OUTER_BOUND ( 'NONE', #35752, .T. ) ;
#29096 = LINE ( 'NONE', #25488, #3327 ) ;
#29097 = DIRECTION ( 'NONE',  ( 0.000000000000000000, 0.000000000000000000, 1.000000000000000000 ) ) ;
#29098 = CARTESIAN_POINT ( 'NONE',  ( -84.94597344681494633, 2.143131898507880377E-16, 82.56828755692798438 ) ) ;
#29099 = ORIENTED_EDGE ( 'NONE', *, *, #19618, .F. ) ;
#29100 = VERTEX_POINT ( 'NONE', #21787 ) ;
#29101 = CARTESIAN_POINT ( 'NONE',  ( -3.239037401336969602, -33.28348308860766025, -8.917361510505369182 ) ) ;
#29102 = CARTESIAN_POINT ( 'NONE',  ( -126.6959734468149321, 1.749999999999997113, -39.18171244307202983 ) ) ;
#29103 = VECTOR ( 'NONE', #47344, 1000.000000000000000 ) ;
#29104 = ORIENTED_EDGE ( 'NONE', *, *, #16314, .F. ) ;
#29105 = ORIENTED_EDGE ( 'NONE', *, *, #42907, .F. ) ;
#29106 = DIRECTION ( 'NONE',  ( 0.9510565162951523099, 0.3090169943749515591, 0.000000000000000000 ) ) ;
#29107 = CARTESIAN_POINT ( 'NONE',  ( 50.00000000000000000, 50.00000000000000000, 800.0000000000000000 ) ) ;
#29108 = CARTESIAN_POINT ( 'NONE',  ( 111.5540265531850679, 0.000000000000000000, 82.56828755692797017 ) ) ;
#29109 = DIRECTION ( 'NONE',  ( -1.000000000000000000, 0.000000000000000000, 0.000000000000000000 ) ) ;
#29110 = ORIENTED_EDGE ( 'NONE', *, *, #1159, .T. ) ;
#29111 = VECTOR ( 'NONE', #47335, 1000.000000000000000 ) ;
#29112 = EDGE_LOOP ( 'NONE', ( #27834, #7847, #12316, #33522 ) ) ;
#29113 = ORIENTED_EDGE ( 'NONE', *, *, #22242, .F. ) ;
#29114 = EDGE_CURVE ( 'NONE', #3719, #37462, #17431, .T. ) ;
#29115 = CARTESIAN_POINT ( 'NONE',  ( -8.445973446814976526, 0.000000000000000000, -40.93171244307205825 ) ) ;
#29117 = VECTOR ( 'NONE', #23959, 1000.000000000000114 ) ;
#29116 = CARTESIAN_POINT ( 'NONE',  ( 194.3291528190321742, 1.750000000000010214, 119.7931612910808781 ) ) ;
#29118 = ORIENTED_EDGE ( 'NONE', *, *, #47497, .T. ) ;
#29119 = VECTOR ( 'NONE', #44804, 1000.000000000000000 ) ;
#29120 = ORIENTED_EDGE ( 'NONE', *, *, #18324, .T. ) ;
#29121 = DIRECTION ( 'NONE',  ( 0.000000000000000000, 0.000000000000000000, -1.000000000000000000 ) ) ;
#29122 = DIRECTION ( 'NONE',  ( 0.000000000000000000, 0.000000000000000000, 1.000000000000000000 ) ) ;
#29123 = ORIENTED_EDGE ( 'NONE', *, *, #38548, .F. ) ;
#29124 = ORIENTED_EDGE ( 'NONE', *, *, #6531, .T. ) ;
#29125 = VECTOR ( 'NONE', #36673, 999.9999999999998863 ) ;
#29126 = CARTESIAN_POINT ( 'NONE',  ( -40.00000000000000000, 0.000000000000000000, 900.0000000000000000 ) ) ;
#29127 = CARTESIAN_POINT ( 'NONE',  ( -46.69597344681494633, 0.000000000000000000, 165.0000000000000000 ) ) ;
#29128 = ORIENTED_EDGE ( 'NONE', *, *, #15632, .T. ) ;
#29129 = CARTESIAN_POINT ( 'NONE',  ( 151.5540265531850537, -1.025126265847089879, 122.5682875569280128 ) ) ;
#29130 = CARTESIAN_POINT ( 'NONE',  ( 10.00000000000000178, -46.01315789473684248, 5.916985404131810178 ) ) ;
#29131 = DIRECTION ( 'NONE',  ( 1.132880637372608740E-16, 4.718402560806925739E-50, 1.000000000000000000 ) ) ;
#29132 = DIRECTION ( 'NONE',  ( -0.000000000000000000, -1.000000000000000000, -0.000000000000000000 ) ) ;
#29133 = EDGE_CURVE ( 'NONE', #46025, #16830, #28735, .T. ) ;
#29134 = ADVANCED_FACE ( 'NONE', ( #41036 ), #37217, .F. ) ;
#29135 = CYLINDRICAL_SURFACE ( 'NONE', #6938, 1.750000000000001554 ) ;
#29136 = EDGE_LOOP ( 'NONE', ( #38903, #2635, #6551, #2879 ) ) ;
#29137 = CARTESIAN_POINT ( 'NONE',  ( -50.11058929355266400, 7.578863168071933387, 7.455576670931136185 ) ) ;
#29138 = CYLINDRICAL_SURFACE ( 'NONE', #2737, 1.750000000000015543 ) ;
#29139 = EDGE_CURVE ( 'NONE', #24319, #41244, #9983, .T. ) ;
#29140 = CARTESIAN_POINT ( 'NONE',  ( -46.69597344681494633, 0.000000000000000000, 165.0000000000000000 ) ) ;
#29141 = CARTESIAN_POINT ( 'NONE',  ( 31.55402655318503236, 0.000000000000000000, -40.93171244307205825 ) ) ;
#29142 = EDGE_CURVE ( 'NONE', #2414, #41332, #1538, .T. ) ;
#29143 = EDGE_CURVE ( 'NONE', #18308, #11343, #46965, .T. ) ;
#29144 = CARTESIAN_POINT ( 'NONE',  ( -64.99999999999909051, 16.00000000000000000, -24.99999999999999289 ) ) ;
#29145 = AXIS2_PLACEMENT_3D ( 'NONE', #34041, #17861, #18359 ) ;
#29146 = EDGE_CURVE ( 'NONE', #9824, #33089, #28978, .T. ) ;
#29147 = CARTESIAN_POINT ( 'NONE',  ( 2.462075149652696027, -16.57295996686994499, 9.403735324607438884 ) ) ;
#29148 = CARTESIAN_POINT ( 'NONE',  ( 339.9999999999999432, 181.0000000000000568, -356.0000000000002274 ) ) ;
#29149 = VECTOR ( 'NONE', #2127, 1000.000000000000000 ) ;
#29150 = CARTESIAN_POINT ( 'NONE',  ( 0.3862712429686810944, 1.188820645368943607, 10.00000000000000000 ) ) ;
#29151 = EDGE_LOOP ( 'NONE', ( #43455, #43999, #39918, #44834, #49559 ) ) ;
#29152 = CARTESIAN_POINT ( 'NONE',  ( -48.44597344681496054, 1.025126265847089435, 122.5682875569280128 ) ) ;
#29153 = VECTOR ( 'NONE', #2777, 1000.000000000000000 ) ;
#29154 = B_SPLINE_CURVE_WITH_KNOTS ( 'NONE', 3,
 ( #30556, #27718, #46154, #11308 ),
 .UNSPECIFIED., .F., .F.,
 ( 4, 4 ),
 ( 0.000000000000000000, 0.0002708531562905854440 ),
 .UNSPECIFIED. ) ;
#29155 = CARTESIAN_POINT ( 'NONE',  ( 29.99999999999998579, 17.00000000000000000, -114.9999999999999858 ) ) ;
#29156 = MECHANICAL_DESIGN_GEOMETRIC_PRESENTATION_REPRESENTATION (  '', ( #2942 ), #43103 ) ;
#29157 = DIRECTION ( 'NONE',  ( -0.000000000000000000, -0.000000000000000000, -1.000000000000000000 ) ) ;
#29158 = CARTESIAN_POINT ( 'NONE',  ( -37.50000000000000000, 0.000000000000000000, 10.00000000000000000 ) ) ;
#29159 = FACE_OUTER_BOUND ( 'NONE', #44147, .T. ) ;
#29160 = VERTEX_POINT ( 'NONE', #7149 ) ;
#29161 = DIRECTION ( 'NONE',  ( 1.000000000000000000, 0.000000000000000000, -1.860490536778032451E-50 ) ) ;
#29162 = VERTEX_POINT ( 'NONE', #26649 ) ;
#29163 = AXIS2_PLACEMENT_3D ( 'NONE', #9633, #12958, #4767 ) ;
#29164 = CARTESIAN_POINT ( 'NONE',  ( -16.76006782980216059, 2.050259795448645228, 9.178419661560148768 ) ) ;
#29165 = AXIS2_PLACEMENT_3D ( 'NONE', #11675, #7578, #23213 ) ;
#29166 = CARTESIAN_POINT ( 'NONE',  ( 75.05402655318509630, 2.143131898507880377E-16, -157.4317124430720014 ) ) ;
#29167 =( BOUNDED_CURVE ( )  B_SPLINE_CURVE ( 3, ( #24965, #5447, #21350, #13149 ),
 .UNSPECIFIED., .F., .F. ) 
 B_SPLINE_CURVE_WITH_KNOTS ( ( 4, 4 ),
 ( 1.570796326794896558, 3.141592653589793116 ),
 .UNSPECIFIED. ) 
 CURVE ( )  GEOMETRIC_REPRESENTATION_ITEM ( )  RATIONAL_B_SPLINE_CURVE ( ( 1.000000000000000000, 0.8047378541243649375, 0.8047378541243649375, 1.000000000000000000 ) ) 
 REPRESENTATION_ITEM ( '' )  );
#29168 = VERTEX_POINT ( 'NONE', #34603 ) ;
#29169 = CARTESIAN_POINT ( 'NONE',  ( 1.782521105131670724, -0.3635605703593869920, 9.903764339332079558 ) ) ;
#29170 = DIRECTION ( 'NONE',  ( -0.000000000000000000, -0.000000000000000000, -1.000000000000000000 ) ) ;
#29171 = EDGE_LOOP ( 'NONE', ( #2427, #23702, #19209, #27595, #17697 ) ) ;
#29172 = VERTEX_POINT ( 'NONE', #23037 ) ;
#29173 = ADVANCED_FACE ( 'NONE', ( #37962 ), #11256, .T. ) ;
#29174 =( BOUNDED_CURVE ( )  B_SPLINE_CURVE ( 3, ( #35531, #14998, #15752, #22689 ),
 .UNSPECIFIED., .F., .F. ) 
 B_SPLINE_CURVE_WITH_KNOTS ( ( 4, 4 ),
 ( 4.712388980384689674, 6.283185307179586232 ),
 .UNSPECIFIED. ) 
 CURVE ( )  GEOMETRIC_REPRESENTATION_ITEM ( )  RATIONAL_B_SPLINE_CURVE ( ( 1.000000000000000000, 0.8047378541243649375, 0.8047378541243649375, 1.000000000000000000 ) ) 
 REPRESENTATION_ITEM ( '' )  );
#29175 = ADVANCED_FACE ( 'NONE', ( #7410 ), #22790, .F. ) ;
#29176 = CARTESIAN_POINT ( 'NONE',  ( 35.05402655318504657, 2.143131898507880377E-16, 119.0682875569279702 ) ) ;
#29177 = CARTESIAN_POINT ( 'NONE',  ( -206.6959734468149463, 1.750000000000010658, -119.1817124430720440 ) ) ;
#29178 = CARTESIAN_POINT ( 'NONE',  ( -8.831420117243776957, -14.12636088103186260, -3.546734833711462365 ) ) ;
#29179 = AXIS2_PLACEMENT_3D ( 'NONE', #31449, #47043, #46538 ) ;
#29180 = ORIENTED_EDGE ( 'NONE', *, *, #2655, .F. ) ;
#29181 = DIRECTION ( 'NONE',  ( 1.000000000000000000, 0.000000000000000000, 0.000000000000000000 ) ) ;
#29182 = FACE_OUTER_BOUND ( 'NONE', #31452, .T. ) ;
#29183 = DIRECTION ( 'NONE',  ( -1.612977847700450206E-50, 0.000000000000000000, 1.000000000000000000 ) ) ;
#29184 = ORIENTED_EDGE ( 'NONE', *, *, #719, .F. ) ;
#29185 = AXIS2_PLACEMENT_3D ( 'NONE', #24202, #39863, #8048 ) ;
#29186 = EDGE_LOOP ( 'NONE', ( #28150, #43250, #49821, #20097 ) ) ;
#29187 = ORIENTED_EDGE ( 'NONE', *, *, #7173, .T. ) ;
#29188 =( BOUNDED_CURVE ( )  B_SPLINE_CURVE ( 3, ( #29438, #47887, #32551, #12780 ),
 .UNSPECIFIED., .F., .F. ) 
 B_SPLINE_CURVE_WITH_KNOTS ( ( 4, 4 ),
 ( 0.000000000000000000, 1.570796326794896558 ),
 .UNSPECIFIED. ) 
 CURVE ( )  GEOMETRIC_REPRESENTATION_ITEM ( )  RATIONAL_B_SPLINE_CURVE ( ( 1.000000000000000000, 0.8047378541243649375, 0.8047378541243649375, 1.000000000000000000 ) ) 
 REPRESENTATION_ITEM ( '' )  );
#29189 = DIRECTION ( 'NONE',  ( -1.000000000000000000, 0.000000000000000000, -2.958228394578794270E-31 ) ) ;
#29190 = ORIENTED_EDGE ( 'NONE', *, *, #34597, .T. ) ;
#29191 = DIRECTION ( 'NONE',  ( -1.000000000000000000, -0.000000000000000000, -0.000000000000000000 ) ) ;
#29192 = DIRECTION ( 'NONE',  ( -0.000000000000000000, -0.000000000000000000, -1.000000000000000000 ) ) ;
#29193 = AXIS2_PLACEMENT_3D ( 'NONE', #24705, #29048, #9294 ) ;
#29194 = CARTESIAN_POINT ( 'NONE',  ( -1.305887768059462717, 0.05395936523972331283, 9.945465957785078359 ) ) ;
#29195 = CARTESIAN_POINT ( 'NONE',  ( 71.55402655318505367, 0.000000000000000000, 42.56828755692799859 ) ) ;
#29196 = VECTOR ( 'NONE', #17449, 1000.000000000000000 ) ;
#29197 = DIRECTION ( 'NONE',  ( 0.000000000000000000, 0.000000000000000000, -1.000000000000000000 ) ) ;
#29198 = CARTESIAN_POINT ( 'NONE',  ( -46.69597344681494633, -1.750000000000009992, 160.8182875569279702 ) ) ;
#29199 = DIRECTION ( 'NONE',  ( 0.000000000000000000, -1.000000000000000000, 0.000000000000000000 ) ) ;
#29200 = DIRECTION ( 'NONE',  ( -1.000000000000000000, 0.000000000000000000, 0.000000000000000000 ) ) ;
#29201 = DIRECTION ( 'NONE',  ( 0.000000000000000000, -1.000000000000000000, 0.000000000000000000 ) ) ;
#29202 = VECTOR ( 'NONE', #31327, 1000.000000000000000 ) ;
#29203 = CARTESIAN_POINT ( 'NONE',  ( -30.25247992116029394, 39.82368563463828792, -3.760136334089591248 ) ) ;
#29204 = CARTESIAN_POINT ( 'NONE',  ( -34.38425513258695077, 36.82177522737848108, 8.807470649214879543 ) ) ;
#29205 = ORIENTED_EDGE ( 'NONE', *, *, #12961, .T. ) ;
#29206 = EDGE_CURVE ( 'NONE', #34290, #20654, #33240, .T. ) ;
#29207 = CARTESIAN_POINT ( 'NONE',  ( 0.000000000000000000, 17.00000000000000000, 0.000000000000000000 ) ) ;
#29208 = CARTESIAN_POINT ( 'NONE',  ( -168.4459734468149747, -1.025126265847089435, 2.568287556927986159 ) ) ;
#29209 = DIRECTION ( 'NONE',  ( -1.000000000000000000, -0.000000000000000000, 4.625929269271635797E-16 ) ) ;
#29210 = ORIENTED_EDGE ( 'NONE', *, *, #2638, .F. ) ;
#29211 = CARTESIAN_POINT ( 'NONE',  ( 0.000000000000000000, 17.00000000000000000, 0.000000000000000000 ) ) ;
#29212 = VECTOR ( 'NONE', #32646, 1000.000000000000000 ) ;
#29213 = PLANE ( 'NONE',  #45816 ) ;
#29214 = ORIENTED_EDGE ( 'NONE', *, *, #12073, .T. ) ;
#29215 = CARTESIAN_POINT ( 'NONE',  ( -165.6708471809677974, 1.750000000000010214, 79.79316129108087807 ) ) ;
#29216 = DIRECTION ( 'NONE',  ( 0.000000000000000000, 1.000000000000000000, 6.123233995736766036E-17 ) ) ;
#29217 = DIRECTION ( 'NONE',  ( -0.000000000000000000, -0.000000000000000000, -1.000000000000000000 ) ) ;
#29218 = ORIENTED_EDGE ( 'NONE', *, *, #14934, .T. ) ;
#29219 = DIRECTION ( 'NONE',  ( -3.172065784643302499E-16, -1.000000000000000000, 2.537652627714642000E-15 ) ) ;
#29220 = EDGE_LOOP ( 'NONE', ( #42041, #26137, #10425, #7030 ) ) ;
#29221 = EDGE_LOOP ( 'NONE', ( #39593, #28260, #4694, #40568, #25520 ) ) ;
#29222 = DIRECTION ( 'NONE',  ( 0.000000000000000000, -1.000000000000000000, 1.604368532695312981E-16 ) ) ;
#29223 = VECTOR ( 'NONE', #31599, 1000.000000000000000 ) ;
#29224 = VERTEX_POINT ( 'NONE', #3280 ) ;
#29225 = CARTESIAN_POINT ( 'NONE',  ( 181.0000000000000000, -5.999999999999950262, -350.0000000000001705 ) ) ;
#29226 = CARTESIAN_POINT ( 'NONE',  ( 210.0000000000000568, 0.000000000000000000, -37.43171244307202272 ) ) ;
#29227 = ORIENTED_EDGE ( 'NONE', *, *, #37194, .T. ) ;
#29228 = LINE ( 'NONE', #37694, #39387 ) ;
#29229 = LINE ( 'NONE', #10663, #1314 ) ;
#29230 = DIRECTION ( 'NONE',  ( -1.000000000000000000, -0.000000000000000000, -0.000000000000000000 ) ) ;
#29231 = CARTESIAN_POINT ( 'NONE',  ( 0.000000000000000000, 17.00000000000000000, 0.000000000000000000 ) ) ;
#29232 = ORIENTED_EDGE ( 'NONE', *, *, #37169, .F. ) ;
#29233 = VECTOR ( 'NONE', #12992, 1000.000000000000000 ) ;
#29234 = CARTESIAN_POINT ( 'NONE',  ( -46.69597344681494633, -1.750000000000010658, -119.1817124430720440 ) ) ;
#29235 = ORIENTED_EDGE ( 'NONE', *, *, #17415, .F. ) ;
#29236 = CARTESIAN_POINT ( 'NONE',  ( 0.000000000000000000, 181.0000000000000284, 355.9999999999997726 ) ) ;
#29237 = CARTESIAN_POINT ( 'NONE',  ( 181.0000000000000284, -174.9999999999999716, -111.0000000000001563 ) ) ;
#29238 = ORIENTED_EDGE ( 'NONE', *, *, #11766, .F. ) ;
#29239 = EDGE_LOOP ( 'NONE', ( #21061, #24002, #33720, #11432 ) ) ;
#29240 = VERTEX_POINT ( 'NONE', #29736 ) ;
#29241 = LINE ( 'NONE', #1294, #28659 ) ;
#29242 = DIRECTION ( 'NONE',  ( 0.000000000000000000, -1.000000000000000000, 0.000000000000000000 ) ) ;
#29243 = ORIENTED_EDGE ( 'NONE', *, *, #36979, .T. ) ;
#29244 = CARTESIAN_POINT ( 'NONE',  ( 0.000000000000000000, 17.00000000000000000, 0.000000000000000000 ) ) ;
#29245 = CARTESIAN_POINT ( 'NONE',  ( 210.0000000000000568, 0.000000000000000000, 120.8182875569279702 ) ) ;
#29246 = CARTESIAN_POINT ( 'NONE',  ( 0.6721397084974982672, 9.977385840602783773, 2.154851817814940063E-15 ) ) ;
#29247 = AXIS2_PLACEMENT_3D ( 'NONE', #40219, #9419, #9163 ) ;
#29248 = ORIENTED_EDGE ( 'NONE', *, *, #24569, .T. ) ;
#29249 = FACE_BOUND ( 'NONE', #23560, .T. ) ;
#29250 = DIRECTION ( 'NONE',  ( -0.000000000000000000, -0.000000000000000000, -1.000000000000000000 ) ) ;
#29251 = CARTESIAN_POINT ( 'NONE',  ( 195.9526953830863079, 2.688010569040066411, 23.74256005001722158 ) ) ;
#29252 = ORIENTED_EDGE ( 'NONE', *, *, #14563, .F. ) ;
#29253 = ITEM_DEFINED_TRANSFORMATION ( 'NONE', 'NONE', #16818,  #45486 ) ;
#29254 = CARTESIAN_POINT ( 'NONE',  ( 115.0540265531850395, 1.025126265847082108, -117.4317124430720440 ) ) ;
#29255 = LINE ( 'NONE', #21811, #28235 ) ;
#29256 =( BOUNDED_CURVE ( )  B_SPLINE_CURVE ( 3, ( #13083, #5632, #5384, #28747 ),
 .UNSPECIFIED., .F., .F. ) 
 B_SPLINE_CURVE_WITH_KNOTS ( ( 4, 4 ),
 ( 1.570796326794896558, 3.141592653589793116 ),
 .UNSPECIFIED. ) 
 CURVE ( )  GEOMETRIC_REPRESENTATION_ITEM ( )  RATIONAL_B_SPLINE_CURVE ( ( 1.000000000000000000, 0.8047378541243649375, 0.8047378541243649375, 1.000000000000000000 ) ) 
 REPRESENTATION_ITEM ( '' )  );
#29257 = FACE_OUTER_BOUND ( 'NONE', #4943, .T. ) ;
#29258 = CARTESIAN_POINT ( 'NONE',  ( 0.3862712429686810944, 1.188820645368943607, 10.00000000000000000 ) ) ;
#29259 = VERTEX_POINT ( 'NONE', #42036 ) ;
#29260 = CARTESIAN_POINT ( 'NONE',  ( -33.89193117067290473, -21.24469349090191983, 910.0000000000000000 ) ) ;
#29261 = ADVANCED_FACE ( 'NONE', ( #26894 ), #29999, .T. ) ;
#29262 = CYLINDRICAL_SURFACE ( 'NONE', #26169, 1.750000000000008438 ) ;
#29263 = DIRECTION ( 'NONE',  ( 0.000000000000000000, 1.000000000000000000, -1.822804496942680012E-16 ) ) ;
#29264 = DIRECTION ( 'NONE',  ( 0.000000000000000000, -1.000000000000000000, 0.000000000000000000 ) ) ;
#29265 = EDGE_CURVE ( 'NONE', #13085, #12365, #34890, .T. ) ;
#29266 = CYLINDRICAL_SURFACE ( 'NONE', #4963, 4.000000000000003553 ) ;
#29267 = EDGE_CURVE ( 'NONE', #35077, #1823, #49160, .T. ) ;
#29268 = VERTEX_POINT ( 'NONE', #15097 ) ;
#29269 = ORIENTED_EDGE ( 'NONE', *, *, #18350, .T. ) ;
#29270 = CARTESIAN_POINT ( 'NONE',  ( -6.875132362119187768, 33.14667368551891258, 8.356839323120299312 ) ) ;
#29271 = APPLICATION_CONTEXT ( 'automotive_design' ) ;
#29272 = ORIENTED_EDGE ( 'NONE', *, *, #29082, .T. ) ;
#29273 = CARTESIAN_POINT ( 'NONE',  ( -166.6959734468149463, 0.000000000000000000, 165.0000000000000000 ) ) ;
#29275 = EDGE_CURVE ( 'NONE', #16751, #21151, #50243, .T. ) ;
#29274 = CARTESIAN_POINT ( 'NONE',  ( 1.578643388466006714, -1.550786058692517511, 9.881002359080275355 ) ) ;
#29276 = EDGE_CURVE ( 'NONE', #8731, #35155, #37033, .T. ) ;
#29277 = CARTESIAN_POINT ( 'NONE',  ( -5.670847180967843570, 1.750000000000023537, -80.20683870891910772 ) ) ;
#29278 = ORIENTED_EDGE ( 'NONE', *, *, #20548, .T. ) ;
#29279 = EDGE_CURVE ( 'NONE', #25367, #46103, #49442, .T. ) ;
#29280 = CARTESIAN_POINT ( 'NONE',  ( -84.94597344681494633, 2.143131898507880377E-16, -0.9317124430720247208 ) ) ;
#29281 = VECTOR ( 'NONE', #24122, 1000.000000000000000 ) ;
#29282 = EDGE_LOOP ( 'NONE', ( #49819, #17240, #14603, #17865 ) ) ;
#29283 = CARTESIAN_POINT ( 'NONE',  ( -14.99999999999812594, 17.00000000000000000, 65.00000000000000000 ) ) ;
#29284 = CARTESIAN_POINT ( 'NONE',  ( 340.0000000000000000, 169.0000000000000284, 359.9999999999998295 ) ) ;
#29285 = FACE_OUTER_BOUND ( 'NONE', #28063, .T. ) ;
#29286 = CARTESIAN_POINT ( 'NONE',  ( -1.540662627795934769, 1.371465786296043765, 9.894754715216725671 ) ) ;
#29287 = DIRECTION ( 'NONE',  ( 0.000000000000000000, 1.000000000000000000, 0.000000000000000000 ) ) ;
#29288 = VERTEX_POINT ( 'NONE', #10487 ) ;
#29290 = EDGE_LOOP ( 'NONE', ( #28603, #3192, #18912, #31047, #417, #31, #6970, #14752 ) ) ;
#29289 = EDGE_CURVE ( 'NONE', #32679, #21399, #14330, .T. ) ;
#29291 = CARTESIAN_POINT ( 'NONE',  ( 2.499999999999945377, -224.9999999999999716, -224.9999999999999716 ) ) ;
#29292 = EDGE_CURVE ( 'NONE', #38442, #48485, #22287, .T. ) ;
#29293 = EDGE_CURVE ( 'NONE', #41952, #17244, #30243, .T. ) ;
#29294 = EDGE_CURVE ( 'NONE', #14457, #43944, #45019, .T. ) ;
#29295 = ORIENTED_EDGE ( 'NONE', *, *, #6477, .F. ) ;
#29296 = CARTESIAN_POINT ( 'NONE',  ( 191.5540265531850537, 1.025126265847088991, -157.4317124430720582 ) ) ;
#29297 = LINE ( 'NONE', #49244, #36312 ) ;
#29298 = ORIENTED_EDGE ( 'NONE', *, *, #15626, .F. ) ;
#29299 = CARTESIAN_POINT ( 'NONE',  ( 340.0000000000000568, 169.0000000000000000, 343.9999999999997726 ) ) ;
#29300 = EDGE_CURVE ( 'NONE', #49733, #17553, #9580, .T. ) ;
#29301 = ADVANCED_FACE ( 'NONE', ( #8423 ), #472, .T. ) ;
#29302 = CARTESIAN_POINT ( 'NONE',  ( 214.9999999999999432, -173.0000000000000000, 112.0000000000000284 ) ) ;
#29303 = B_SPLINE_SURFACE_WITH_KNOTS ( 'NONE', 3, 3, ( 
 ( #1425, #36331, #17992, #24769 ),
 ( #16559, #4751, #43992, #9114 ),
 ( #14140, #13203, #32716, #20393 ),
 ( #48057, #18242, #22106, #28861 ) ),
 .UNSPECIFIED., .F., .F., .F.,
 ( 4, 4 ),
 ( 4, 4 ),
 ( 0.000000000000000000, 1.000000000000000000 ),
 ( 0.000000000000000000, 1.000000000000000000 ),
 .UNSPECIFIED. ) ;
#29304 = ORIENTED_EDGE ( 'NONE', *, *, #9516, .F. ) ;
#29305 = CYLINDRICAL_SURFACE ( 'NONE', #31754, 4.000000000000003553 ) ;
#29306 = CARTESIAN_POINT ( 'NONE',  ( -14.91630425054805187, 7.943683830272224355, -9.008049429158100807 ) ) ;
#29307 = CARTESIAN_POINT ( 'NONE',  ( 1.343171584779923933, -1.414327272009459291, 9.896382706792440587 ) ) ;
#29308 = ORIENTED_EDGE ( 'NONE', *, *, #15222, .F. ) ;
#29309 = ORIENTED_EDGE ( 'NONE', *, *, #49394, .T. ) ;
#29310 = DIRECTION ( 'NONE',  ( -0.8962124318248270161, 0.000000000000000000, 0.4436251537532894806 ) ) ;
#29311 = CARTESIAN_POINT ( 'NONE',  ( -225.0000000000000568, 164.9999999999999716, 372.0000000000000000 ) ) ;
#29312 = DIRECTION ( 'NONE',  ( -0.000000000000000000, -0.000000000000000000, -1.000000000000000000 ) ) ;
#29313 = CARTESIAN_POINT ( 'NONE',  ( 210.0000000000000568, 0.000000000000000000, 80.81828755692798438 ) ) ;
#29314 = VERTEX_POINT ( 'NONE', #42781 ) ;
#29315 = ADVANCED_FACE ( 'NONE', ( #32028 ), #43297, .T. ) ;
#29316 = CARTESIAN_POINT ( 'NONE',  ( 111.5540265531850537, 1.025126265847081664, 42.56828755692797017 ) ) ;
#29317 = VERTEX_POINT ( 'NONE', #47363 ) ;
#29318 = CARTESIAN_POINT ( 'NONE',  ( 164.9999999999999716, 17.00000000000000000, 115.0000000000000142 ) ) ;
#29319 =( BOUNDED_CURVE ( )  B_SPLINE_CURVE ( 3, ( #36451, #1290, #40286, #13069 ),
 .UNSPECIFIED., .F., .F. ) 
 B_SPLINE_CURVE_WITH_KNOTS ( ( 4, 4 ),
 ( 1.570796326794896780, 3.141592653589793116 ),
 .UNSPECIFIED. ) 
 CURVE ( )  GEOMETRIC_REPRESENTATION_ITEM ( )  RATIONAL_B_SPLINE_CURVE ( ( 1.000000000000000000, 0.8047378541243650485, 0.8047378541243650485, 1.000000000000000000 ) ) 
 REPRESENTATION_ITEM ( '' )  );
#29320 = CARTESIAN_POINT ( 'NONE',  ( 210.0000000000000568, 0.000000000000000000, 120.8182875569279702 ) ) ;
#29321 = CARTESIAN_POINT ( 'NONE',  ( -6.695973446814940111, -1.750000000000024203, 120.8182875569279702 ) ) ;
#29322 = EDGE_CURVE ( 'NONE', #36125, #46025, #28410, .T. ) ;
#29323 = CIRCLE ( 'NONE', #24390, 2.000000000000001776 ) ;
#29324 = ADVANCED_FACE ( 'NONE', ( #16115 ), #31016, .T. ) ;
#29325 = CARTESIAN_POINT ( 'NONE',  ( 350.0000000000000000, 185.0000000000000284, -356.0000000000002274 ) ) ;
#29326 = FACE_OUTER_BOUND ( 'NONE', #22916, .T. ) ;
#29327 = DIRECTION ( 'NONE',  ( 1.000000000000000000, 0.000000000000000000, 0.000000000000000000 ) ) ;
#29328 = ORIENTED_EDGE ( 'NONE', *, *, #27289, .F. ) ;
#29329 = CARTESIAN_POINT ( 'NONE',  ( 0.000000000000000000, 169.0000000000000000, -356.0000000000002274 ) ) ;
#29330 =( BOUNDED_CURVE ( )  B_SPLINE_CURVE ( 3, ( #29633, #45255, #2441, #25537 ),
 .UNSPECIFIED., .F., .F. ) 
 B_SPLINE_CURVE_WITH_KNOTS ( ( 4, 4 ),
 ( 3.141592653589793116, 4.712388980384689674 ),
 .UNSPECIFIED. ) 
 CURVE ( )  GEOMETRIC_REPRESENTATION_ITEM ( )  RATIONAL_B_SPLINE_CURVE ( ( 1.000000000000000000, 0.8047378541243649375, 0.8047378541243649375, 1.000000000000000000 ) ) 
 REPRESENTATION_ITEM ( '' )  );
#29331 = CARTESIAN_POINT ( 'NONE',  ( 175.0000000000000000, 15.00000000000000000, -122.5000000000000000 ) ) ;
#29332 = CARTESIAN_POINT ( 'NONE',  ( 181.0000000000000000, 175.0000000000000284, -356.0000000000001705 ) ) ;
#29333 = EDGE_CURVE ( 'NONE', #31279, #32219, #14369, .T. ) ;
#29334 = CARTESIAN_POINT ( 'NONE',  ( 0.3862712429686810944, 1.188820645368943607, 10.00000000000000000 ) ) ;
#29335 = ORIENTED_EDGE ( 'NONE', *, *, #16177, .T. ) ;
#29336 = CARTESIAN_POINT ( 'NONE',  ( -20.37409433808010562, -26.28007012093468475, -2.408242355805840784 ) ) ;
#29337 = VERTEX_POINT ( 'NONE', #35883 ) ;
#29338 = CARTESIAN_POINT ( 'NONE',  ( 45.64490844644690526, 21.32281559348795597, 8.807470649214879543 ) ) ;
#29339 = CARTESIAN_POINT ( 'NONE',  ( 181.0000000000000000, -7.999999999999952038, -340.0000000000001137 ) ) ;
#29340 = FACE_OUTER_BOUND ( 'NONE', #6068, .T. ) ;
#29341 = EDGE_CURVE ( 'NONE', #29584, #45429, #8677, .T. ) ;
#29342 = ORIENTED_EDGE ( 'NONE', *, *, #13429, .F. ) ;
#29343 = B_SPLINE_CURVE_WITH_KNOTS ( 'NONE', 3,
 ( #33757, #34727, #20064, #39581 ),
 .UNSPECIFIED., .F., .F.,
 ( 4, 4 ),
 ( 0.000000000000000000, 0.001249001861321270834 ),
 .UNSPECIFIED. ) ;
#29344 = CARTESIAN_POINT ( 'NONE',  ( 7.749480817862238524, 14.85497772329518895, 9.403735324607438884 ) ) ;
#29345 = DIRECTION ( 'NONE',  ( 0.000000000000000000, 0.000000000000000000, -1.000000000000000000 ) ) ;
#29346 = ADVANCED_FACE ( 'NONE', ( #27919 ), #11504, .T. ) ;
#29347 = CARTESIAN_POINT ( 'NONE',  ( 166.9999999999999716, 175.0000000000000284, -344.0000000000001137 ) ) ;
#29348 = CARTESIAN_POINT ( 'NONE',  ( 155.0540265531850537, 0.000000000000000000, 162.5682875569279702 ) ) ;
#29349 = ORIENTED_EDGE ( 'NONE', *, *, #37194, .F. ) ;
#29350 = EDGE_LOOP ( 'NONE', ( #45164, #8961, #35503, #49915 ) ) ;
#29351 = DIRECTION ( 'NONE',  ( -0.000000000000000000, -0.000000000000000000, -1.000000000000000000 ) ) ;
#29352 = CARTESIAN_POINT ( 'NONE',  ( -0.3862712429686977478, 1.188820645368937390, -10.00000000000000000 ) ) ;
#29353 = EDGE_CURVE ( 'NONE', #41804, #7870, #19706, .T. ) ;
#29354 = ADVANCED_FACE ( 'NONE', ( #38967 ), #19948, .F. ) ;
#29355 = AXIS2_PLACEMENT_3D ( 'NONE', #26473, #27683, #27939 ) ;
#29356 = ORIENTED_EDGE ( 'NONE', *, *, #25559, .T. ) ;
#29357 = ORIENTED_EDGE ( 'NONE', *, *, #11890, .T. ) ;
#29358 = CARTESIAN_POINT ( 'NONE',  ( -114.9999999999987779, 16.00000000000000000, 30.00000000000000000 ) ) ;
#29359 = CYLINDRICAL_SURFACE ( 'NONE', #33998, 1.750000000000015543 ) ;
#29360 = ORIENTED_EDGE ( 'NONE', *, *, #16153, .F. ) ;
#29361 = ADVANCED_FACE ( 'NONE', ( #15360 ), #46928, .T. ) ;
#29362 = VERTEX_POINT ( 'NONE', #15857 ) ;
#29363 = ADVANCED_FACE ( 'NONE', ( #31526 ), #47111, .T. ) ;
#29364 = ADVANCED_FACE ( 'NONE', ( #8915 ), #33293, .F. ) ;
#29365 = CARTESIAN_POINT ( 'NONE',  ( 224.9999999999999716, -175.0000000000000000, 62.29650858650038003 ) ) ;
#29366 = VERTEX_POINT ( 'NONE', #13510 ) ;
#29367 = VERTEX_POINT ( 'NONE', #21461 ) ;
#29368 = DIRECTION ( 'NONE',  ( -1.000000000000000000, -0.000000000000000000, -0.000000000000000000 ) ) ;
#29369 = LINE ( 'NONE', #17814, #33908 ) ;
#29370 = ORIENTED_EDGE ( 'NONE', *, *, #4593, .T. ) ;
#29371 = EDGE_LOOP ( 'NONE', ( #38845, #22238, #2402, #17807, #10024, #36719 ) ) ;
#29372 = CARTESIAN_POINT ( 'NONE',  ( -1.769963848780949478, 9.842115015280430868, 0.000000000000000000 ) ) ;
#29373 = LINE ( 'NONE', #44000, #20689 ) ;
#29374 = EDGE_LOOP ( 'NONE', ( #12539, #20053, #22057, #37358 ) ) ;
#29375 = CARTESIAN_POINT ( 'NONE',  ( -8.176860274785726190, 5.756644512789648616, 9.282506307616472441 ) ) ;
#29376 = CARTESIAN_POINT ( 'NONE',  ( 7.500000000000000000, 224.9999999999999716, -224.9999999999999716 ) ) ;
#29377 = CARTESIAN_POINT ( 'NONE',  ( 210.0000000000000568, 0.000000000000000000, -39.18171244307202983 ) ) ;
#29378 = DIRECTION ( 'NONE',  ( 0.000000000000000000, -3.186989995019654210E-49, -1.000000000000000000 ) ) ;
#29379 = EDGE_CURVE ( 'NONE', #16336, #12217, #32538, .T. ) ;
#29380 = CARTESIAN_POINT ( 'NONE',  ( 71.55402655318505367, 0.000000000000000000, -77.43171244307198720 ) ) ;
#29381 = ORIENTED_EDGE ( 'NONE', *, *, #10833, .F. ) ;
#29382 = CARTESIAN_POINT ( 'NONE',  ( 113.3040265531850537, -1.749999999999997335, 80.81828755692798438 ) ) ;
#29383 = DIRECTION ( 'NONE',  ( 0.000000000000000000, -1.000000000000000000, 0.000000000000000000 ) ) ;
#29384 = CARTESIAN_POINT ( 'NONE',  ( -166.6959734468149463, -1.750000000000010658, 120.8182875569279702 ) ) ;
#29385 = DIRECTION ( 'NONE',  ( 1.132880637372608740E-16, 4.718402560806925739E-50, 1.000000000000000000 ) ) ;
#29386 = VECTOR ( 'NONE', #43263, 1000.000000000000000 ) ;
#29387 = PLANE ( 'NONE',  #19854 ) ;
#29388 = CARTESIAN_POINT ( 'NONE',  ( 181.0000000000000000, -9.999999999999953815, 339.9999999999998295 ) ) ;
#29389 = CARTESIAN_POINT ( 'NONE',  ( -5.000000000000000000, 165.2000000000000171, 340.1999999999997044 ) ) ;
#29390 = CARTESIAN_POINT ( 'NONE',  ( -86.69597344681496054, 0.000000000000000000, 165.0000000000000000 ) ) ;
#29391 = CARTESIAN_POINT ( 'NONE',  ( -543.3973046169135159, 54.43801056904003133, -177.1374399499827916 ) ) ;
#29392 = ORIENTED_EDGE ( 'NONE', *, *, #30646, .T. ) ;
#29393 = CARTESIAN_POINT ( 'NONE',  ( 1.011271242968688311, -0.7347315653655855927, 10.00000000000000000 ) ) ;
#29394 = LINE ( 'NONE', #5798, #15578 ) ;
#29395 =( BOUNDED_CURVE ( )  B_SPLINE_CURVE ( 3, ( #20230, #35900, #730, #5770 ),
 .UNSPECIFIED., .F., .F. ) 
 B_SPLINE_CURVE_WITH_KNOTS ( ( 4, 4 ),
 ( 0.000000000000000000, 1.570796326794896558 ),
 .UNSPECIFIED. ) 
 CURVE ( )  GEOMETRIC_REPRESENTATION_ITEM ( )  RATIONAL_B_SPLINE_CURVE ( ( 1.000000000000000000, 0.8047378541243649375, 0.8047378541243649375, 1.000000000000000000 ) ) 
 REPRESENTATION_ITEM ( '' )  );
#29396 = CYLINDRICAL_SURFACE ( 'NONE', #28626, 1.750000000000001554 ) ;
#29397 = CARTESIAN_POINT ( 'NONE',  ( 181.0000000000000000, -5.999999999999950262, -340.0000000000001137 ) ) ;
#29398 = CARTESIAN_POINT ( 'NONE',  ( 36.97942854200454832, -6.226705766838405154, 8.914903342594563185 ) ) ;
#29399 = ORIENTED_EDGE ( 'NONE', *, *, #38757, .T. ) ;
#29400 = FACE_OUTER_BOUND ( 'NONE', #7624, .T. ) ;
#29401 = B_SPLINE_SURFACE_WITH_KNOTS ( 'NONE', 3, 3, ( 
 ( #40680, #36602, #48322, #39930 ),
 ( #36850, #5516, #36086, #16067 ),
 ( #13211, #44493, #12206, #4513 ),
 ( #28872, #666, #8374, #8622 ) ),
 .UNSPECIFIED., .F., .F., .F.,
 ( 4, 4 ),
 ( 4, 4 ),
 ( 0.000000000000000000, 1.000000000000000000 ),
 ( 0.000000000000000000, 1.000000000000000000 ),
 .UNSPECIFIED. ) ;
#29402 = VERTEX_POINT ( 'NONE', #29421 ) ;
#29403 = CARTESIAN_POINT ( 'NONE',  ( 164.9999999999999716, 175.0000000000000284, -356.0000000000001705 ) ) ;
#29404 = CARTESIAN_POINT ( 'NONE',  ( -114.9999999999991047, 17.00000000000000000, -24.99999999999999289 ) ) ;
#29405 = EDGE_CURVE ( 'NONE', #23455, #48356, #44049, .T. ) ;
#29406 = ADVANCED_FACE ( 'NONE', ( #25322 ), #13004, .T. ) ;
#29407 = ORIENTED_EDGE ( 'NONE', *, *, #33487, .T. ) ;
#29408 = LINE ( 'NONE', #18106, #33605 ) ;
#29409 = DIRECTION ( 'NONE',  ( 0.000000000000000000, -1.822804496942679766E-16, -1.000000000000000000 ) ) ;
#29410 = ORIENTED_EDGE ( 'NONE', *, *, #48474, .F. ) ;
#29411 = ORIENTED_EDGE ( 'NONE', *, *, #14993, .F. ) ;
#29412 = EDGE_CURVE ( 'NONE', #33082, #21642, #37150, .T. ) ;
#29413 = B_SPLINE_CURVE_WITH_KNOTS ( 'NONE', 3,
 ( #38011, #49741, #47667, #11817 ),
 .UNSPECIFIED., .F., .F.,
 ( 4, 4 ),
 ( 0.7491799374948677759, 1.000000000000000000 ),
 .UNSPECIFIED. ) ;
#29415 = EDGE_CURVE ( 'NONE', #22675, #32324, #38488, .T. ) ;
#29414 = CARTESIAN_POINT ( 'NONE',  ( -1.066995270233474624, 50.00000000000000711, -3.760136334089591248 ) ) ;
#29416 = AXIS2_PLACEMENT_3D ( 'NONE', #44499, #44755, #25528 ) ;
#29417 = ADVANCED_FACE ( 'NONE', ( #47873, #45044 ), #32280, .T. ) ;
#29418 = DIRECTION ( 'NONE',  ( -2.874857526315640942E-31, 1.000000000000000000, -2.537652627714643577E-15 ) ) ;
#29419 = VERTEX_POINT ( 'NONE', #9668 ) ;
#29420 = VECTOR ( 'NONE', #36937, 1000.000000000000000 ) ;
#29421 = CARTESIAN_POINT ( 'NONE',  ( 196.8526953830863135, 160.1880105690400171, 22.84256005001721945 ) ) ;
#29422 = LINE ( 'NONE', #5820, #37029 ) ;
#29423 = DIRECTION ( 'NONE',  ( -0.000000000000000000, -0.000000000000000000, -1.000000000000000000 ) ) ;
#29424 = ORIENTED_EDGE ( 'NONE', *, *, #14486, .T. ) ;
#29425 = ORIENTED_EDGE ( 'NONE', *, *, #13113, .T. ) ;
#29426 = CARTESIAN_POINT ( 'NONE',  ( 112.2789002873379758, -1.749999999999996669, -40.20683870891911482 ) ) ;
#29427 = AXIS2_PLACEMENT_3D ( 'NONE', #16959, #35963, #16199 ) ;
#29428 = AXIS2_PLACEMENT_3D ( 'NONE', #7726, #7211, #23366 ) ;
#29429 = AXIS2_PLACEMENT_3D ( 'NONE', #41813, #45384, #34145 ) ;
#29430 = ADVANCED_FACE ( 'NONE', ( #25575 ), #41216, .F. ) ;
#29431 = FACE_OUTER_BOUND ( 'NONE', #40142, .T. ) ;
#29432 = ORIENTED_EDGE ( 'NONE', *, *, #16419, .F. ) ;
#29433 = VECTOR ( 'NONE', #19005, 1000.000000000000000 ) ;
#29434 = FACE_OUTER_BOUND ( 'NONE', #41144, .T. ) ;
#29435 = LINE ( 'NONE', #9680, #24772 ) ;
#29436 = DIRECTION ( 'NONE',  ( 1.000000000000000000, 0.000000000000000000, 0.000000000000000000 ) ) ;
#29437 = CARTESIAN_POINT ( 'NONE',  ( -4.999999999999948486, -214.9999999999999716, -234.7500000000000000 ) ) ;
#29438 = CARTESIAN_POINT ( 'NONE',  ( -88.44597344681497475, 0.000000000000000000, 79.06828755692795596 ) ) ;
#29439 = FACE_OUTER_BOUND ( 'NONE', #38419, .T. ) ;
#29440 = CARTESIAN_POINT ( 'NONE',  ( 12.16428377685533135, 11.73151505502934988, -9.008049429158100807 ) ) ;
#29441 = CARTESIAN_POINT ( 'NONE',  ( 181.0000000000000000, 8.000000000000062172, 339.9999999999998295 ) ) ;
#29442 = LINE ( 'NONE', #17641, #42447 ) ;
#29443 = CARTESIAN_POINT ( 'NONE',  ( 210.0000000000000568, 2.143131898507884075E-16, 39.06828755692797728 ) ) ;
#29444 = CARTESIAN_POINT ( 'NONE',  ( 1.011271242968683648, 0.7347315653655930312, 3.333333333333333481 ) ) ;
#29445 = ORIENTED_EDGE ( 'NONE', *, *, #8750, .F. ) ;
#29446 = B_SPLINE_CURVE_WITH_KNOTS ( 'NONE', 3,
 ( #15767, #20636, #11933, #31438 ),
 .UNSPECIFIED., .F., .F.,
 ( 4, 4 ),
 ( 0.0003850166616901197036, 0.006523527006578243477 ),
 .UNSPECIFIED. ) ;
#29447 = DIRECTION ( 'NONE',  ( -0.000000000000000000, -0.000000000000000000, 1.000000000000000000 ) ) ;
#29448 = CARTESIAN_POINT ( 'NONE',  ( -15.00099850811941948, -7.462898891544107016, 9.403735324607438884 ) ) ;
#29449 = VECTOR ( 'NONE', #38947, 1000.000000000000000 ) ;
#29450 = CARTESIAN_POINT ( 'NONE',  ( 35.00000000000091660, 17.00000000000000000, -24.99999999999999289 ) ) ;
#29451 = EDGE_CURVE ( 'NONE', #12553, #27291, #20714, .T. ) ;
#29452 = AXIS2_PLACEMENT_3D ( 'NONE', #43158, #40818, #40074 ) ;
#29453 =( BOUNDED_CURVE ( )  B_SPLINE_CURVE ( 3, ( #394, #20379, #47545, #42962 ),
 .UNSPECIFIED., .F., .F. ) 
 B_SPLINE_CURVE_WITH_KNOTS ( ( 4, 4 ),
 ( 1.570796326794896558, 3.141592653589793116 ),
 .UNSPECIFIED. ) 
 CURVE ( )  GEOMETRIC_REPRESENTATION_ITEM ( )  RATIONAL_B_SPLINE_CURVE ( ( 1.000000000000000000, 0.8047378541243649375, 0.8047378541243649375, 1.000000000000000000 ) ) 
 REPRESENTATION_ITEM ( '' )  );
#29454 = VERTEX_POINT ( 'NONE', #16876 ) ;
#29455 = LINE ( 'NONE', #32821, #30557 ) ;
#29456 = CIRCLE ( 'NONE', #17153, 4.000000000000003553 ) ;
#29457 = CARTESIAN_POINT ( 'NONE',  ( -48.44597344681496054, 1.025126265847089213, 162.5682875569279133 ) ) ;
#29458 = ORIENTED_EDGE ( 'NONE', *, *, #36855, .F. ) ;
#29459 = DIRECTION ( 'NONE',  ( 0.000000000000000000, 0.000000000000000000, 1.000000000000000000 ) ) ;
#29460 = CARTESIAN_POINT ( 'NONE',  ( -6.695973446814940111, -1.750000000000024203, 120.8182875569279702 ) ) ;
#29461 = DIRECTION ( 'NONE',  ( -0.000000000000000000, -0.000000000000000000, 1.000000000000000000 ) ) ;
#29462 = AXIS2_PLACEMENT_3D ( 'NONE', #14874, #18957, #30523 ) ;
#29463 = DIRECTION ( 'NONE',  ( 0.000000000000000000, -1.000000000000000000, 0.000000000000000000 ) ) ;
#29464 =( BOUNDED_CURVE ( )  B_SPLINE_CURVE ( 3, ( #46056, #41235, #26355, #6345 ),
 .UNSPECIFIED., .F., .F. ) 
 B_SPLINE_CURVE_WITH_KNOTS ( ( 4, 4 ),
 ( 3.141592653589793116, 4.712388980384689674 ),
 .UNSPECIFIED. ) 
 CURVE ( )  GEOMETRIC_REPRESENTATION_ITEM ( )  RATIONAL_B_SPLINE_CURVE ( ( 1.000000000000000000, 0.8047378541243649375, 0.8047378541243649375, 1.000000000000000000 ) ) 
 REPRESENTATION_ITEM ( '' )  );
#29465 = ORIENTED_EDGE ( 'NONE', *, *, #40839, .F. ) ;
#29466 = CARTESIAN_POINT ( 'NONE',  ( 71.55402655318505367, 0.000000000000000000, -80.93171244307204404 ) ) ;
#29467 = VERTEX_POINT ( 'NONE', #5564 ) ;
#29468 = ORIENTED_EDGE ( 'NONE', *, *, #29695, .F. ) ;
#29469 = CARTESIAN_POINT ( 'NONE',  ( 169.0000000000000284, 175.0000000000000284, 343.9999999999998863 ) ) ;
#29470 = VECTOR ( 'NONE', #14177, 1000.000000000000000 ) ;
#29471 = ORIENTED_EDGE ( 'NONE', *, *, #48337, .F. ) ;
#29472 = CARTESIAN_POINT ( 'NONE',  ( -166.6959734468149463, 1.750000000000010214, 40.81828755692798438 ) ) ;
#29473 = CARTESIAN_POINT ( 'NONE',  ( -167.7210997126620384, 1.750000000000009548, 161.8434138227750907 ) ) ;
#29474 = ORIENTED_EDGE ( 'NONE', *, *, #34600, .T. ) ;
#29475 = CARTESIAN_POINT ( 'NONE',  ( -543.5890838333644979, -61.66198943095990614, -176.2581102438216192 ) ) ;
#29476 = DIRECTION ( 'NONE',  ( 6.203854594147707562E-25, -2.067951531382569187E-25, 1.000000000000000000 ) ) ;
#29477 =( BOUNDED_CURVE ( )  B_SPLINE_CURVE ( 3, ( #36843, #21160, #1672, #17312 ),
 .UNSPECIFIED., .F., .F. ) 
 B_SPLINE_CURVE_WITH_KNOTS ( ( 4, 4 ),
 ( 4.712388980384689674, 6.283185307179586232 ),
 .UNSPECIFIED. ) 
 CURVE ( )  GEOMETRIC_REPRESENTATION_ITEM ( )  RATIONAL_B_SPLINE_CURVE ( ( 1.000000000000000000, 0.8047378541243649375, 0.8047378541243649375, 1.000000000000000000 ) ) 
 REPRESENTATION_ITEM ( '' )  );
#29478 = DIRECTION ( 'NONE',  ( 1.000000000000000000, 0.000000000000000000, -0.000000000000000000 ) ) ;
#29479 = ORIENTED_EDGE ( 'NONE', *, *, #22385, .F. ) ;
#29480 = DIRECTION ( 'NONE',  ( 0.000000000000000000, -1.000000000000000000, 0.000000000000000000 ) ) ;
#29481 = EDGE_CURVE ( 'NONE', #24944, #34755, #5053, .T. ) ;
#29482 = CARTESIAN_POINT ( 'NONE',  ( 0.000000000000000000, 17.00000000000000000, 0.000000000000000000 ) ) ;
#29483 = ORIENTED_EDGE ( 'NONE', *, *, #12669, .F. ) ;
#29484 = DIRECTION ( 'NONE',  ( -0.000000000000000000, -1.000000000000000000, -0.000000000000000000 ) ) ;
#29485 = CARTESIAN_POINT ( 'NONE',  ( 210.0000000000000568, 0.000000000000000000, 80.81828755692798438 ) ) ;
#29486 = ORIENTED_EDGE ( 'NONE', *, *, #14888, .T. ) ;
#29487 = ORIENTED_EDGE ( 'NONE', *, *, #26918, .F. ) ;
#29488 = VERTEX_POINT ( 'NONE', #48371 ) ;
#29489 = CARTESIAN_POINT ( 'NONE',  ( -4.945973446814917018, 1.025126265847097207, -157.4317124430720014 ) ) ;
#29490 = ADVANCED_FACE ( 'NONE', ( #40477 ), #48118, .F. ) ;
#29491 = CARTESIAN_POINT ( 'NONE',  ( -114.9999999999991047, 17.00000000000000000, 0.000000000000000000 ) ) ;
#29492 = EDGE_LOOP ( 'NONE', ( #36083, #34477, #27777, #12672 ) ) ;
#29493 = AXIS2_PLACEMENT_3D ( 'NONE', #36954, #8967, #28222 ) ;
#29494 = VECTOR ( 'NONE', #30731, 1000.000000000000000 ) ;
#29495 = CARTESIAN_POINT ( 'NONE',  ( -70.00000000000002842, 16.00000000000000000, -114.9999999999999858 ) ) ;
#29496 = CARTESIAN_POINT ( 'NONE',  ( -6.695973446814940111, 0.000000000000000000, 165.0000000000000000 ) ) ;
#29497 = DIRECTION ( 'NONE',  ( 0.000000000000000000, 0.000000000000000000, 1.000000000000000000 ) ) ;
#29498 = VECTOR ( 'NONE', #41130, 1000.000000000000000 ) ;
#29499 = CARTESIAN_POINT ( 'NONE',  ( -40.00000000000000000, 0.000000000000000000, 897.6604670114603550 ) ) ;
#29500 = VERTEX_POINT ( 'NONE', #5313 ) ;
#29501 = CARTESIAN_POINT ( 'NONE',  ( 135.0000000000012790, 17.00000000000000000, 30.00000000000000000 ) ) ;
#29502 = DIRECTION ( 'NONE',  ( 0.000000000000000000, -1.000000000000000000, 2.969158215481698263E-48 ) ) ;
#29503 = VECTOR ( 'NONE', #48182, 1000.000000000000000 ) ;
#29504 = LINE ( 'NONE', #29251, #14981 ) ;
#29505 = VERTEX_POINT ( 'NONE', #20975 ) ;
#29507 = LINE ( 'NONE', #21810, #6041 ) ;
#29506 = VECTOR ( 'NONE', #79, 1000.000000000000000 ) ;
#29508 = CARTESIAN_POINT ( 'NONE',  ( -124.9459734468149321, 1.025126265847081886, 119.0682875569279702 ) ) ;
#29509 = CARTESIAN_POINT ( 'NONE',  ( -1.011271242968683426, -0.7347315653655928092, 10.00000000000000000 ) ) ;
#29510 = DIRECTION ( 'NONE',  ( 0.000000000000000000, 0.000000000000000000, 1.000000000000000000 ) ) ;
#29511 = ORIENTED_EDGE ( 'NONE', *, *, #40037, .F. ) ;
#29512 = LINE ( 'NONE', #13605, #18959 ) ;
#29513 = CYLINDRICAL_SURFACE ( 'NONE', #19609, 0.5000000000000004441 ) ;
#29514 = CARTESIAN_POINT ( 'NONE',  ( -14.99999999999937472, 17.00000000000000000, -54.99999999999999289 ) ) ;
#29515 = CARTESIAN_POINT ( 'NONE',  ( 0.8284317003885898201, 1.889026769141425310, 9.889206916986893248 ) ) ;
#29516 = CARTESIAN_POINT ( 'NONE',  ( 85.00000000000090949, 17.00000000000000000, 0.000000000000000000 ) ) ;
#29517 = EDGE_CURVE ( 'NONE', #42480, #50107, #18809, .T. ) ;
#29518 = ORIENTED_EDGE ( 'NONE', *, *, #7184, .F. ) ;
#29519 = CARTESIAN_POINT ( 'NONE',  ( 358.0000000000001137, 182.1715728752538155, 357.1715728752536734 ) ) ;
#29520 = ORIENTED_EDGE ( 'NONE', *, *, #26189, .T. ) ;
#29521 = CARTESIAN_POINT ( 'NONE',  ( 0.000000000000000000, 181.0000000000000284, -344.0000000000001705 ) ) ;
#29522 = ORIENTED_EDGE ( 'NONE', *, *, #5845, .F. ) ;
#29523 = CARTESIAN_POINT ( 'NONE',  ( 111.5540265531850537, 0.000000000000000000, 162.5682875569279702 ) ) ;
#29524 = LINE ( 'NONE', #24677, #384 ) ;
#29525 = CARTESIAN_POINT ( 'NONE',  ( 85.00000000000090949, 17.00000000000000000, -24.99999999999999289 ) ) ;
#29526 = ORIENTED_EDGE ( 'NONE', *, *, #25437, .F. ) ;
#29527 = VECTOR ( 'NONE', #7702, 1000.000000000000000 ) ;
#29528 = CARTESIAN_POINT ( 'NONE',  ( -204.9459734468149463, 2.143131898507880377E-16, 165.0000000000000000 ) ) ;
#29529 = ORIENTED_EDGE ( 'NONE', *, *, #43963, .T. ) ;
#29530 = CARTESIAN_POINT ( 'NONE',  ( 194.9999999999999432, 164.9999999999999716, 352.0000000000000000 ) ) ;
#29531 = CARTESIAN_POINT ( 'NONE',  ( 210.0000000000000568, 0.000000000000000000, 162.5682875569279702 ) ) ;
#29532 = CARTESIAN_POINT ( 'NONE',  ( 73.30402655318508209, -1.750000000000009992, 160.8182875569279702 ) ) ;
#29533 = VECTOR ( 'NONE', #22483, 1000.000000000000000 ) ;
#29534 = DIRECTION ( 'NONE',  ( 0.000000000000000000, 0.000000000000000000, -1.000000000000000000 ) ) ;
#29535 = PRESENTATION_LAYER_ASSIGNMENT (  '', '', ( #16428 ) ) ;
#29536 = VERTEX_POINT ( 'NONE', #32782 ) ;
#29537 = ORIENTED_EDGE ( 'NONE', *, *, #12924, .F. ) ;
#29538 = DIRECTION ( 'NONE',  ( -2.775557561562891351E-16, -0.7071067811865477948, -0.7071067811865473507 ) ) ;
#29539 = ORIENTED_EDGE ( 'NONE', *, *, #18897, .F. ) ;
#29540 = CARTESIAN_POINT ( 'NONE',  ( 210.0000000000000568, 0.000000000000000000, -79.18171244307201562 ) ) ;
#29541 = CARTESIAN_POINT ( 'NONE',  ( -126.6959734468149321, -1.749999999999997335, 120.8182875569279702 ) ) ;
#29542 = ORIENTED_EDGE ( 'NONE', *, *, #24897, .T. ) ;
#29543 = PLANE ( 'NONE',  #40970 ) ;
#29544 = B_SPLINE_CURVE_WITH_KNOTS ( 'NONE', 3,
 ( #15341, #30996, #46585, #11482 ),
 .UNSPECIFIED., .F., .F.,
 ( 4, 4 ),
 ( 0.000000000000000000, 0.0001252128669263237308 ),
 .UNSPECIFIED. ) ;
#29545 = ADVANCED_FACE ( 'NONE', ( #7342 ), #10426, .F. ) ;
#29546 = ORIENTED_EDGE ( 'NONE', *, *, #13705, .T. ) ;
#29547 = B_SPLINE_CURVE_WITH_KNOTS ( 'NONE', 3,
 ( #21631, #37320, #2144, #17788 ),
 .UNSPECIFIED., .F., .F.,
 ( 4, 4 ),
 ( 0.9890644561681873892, 1.000000000000000000 ),
 .UNSPECIFIED. ) ;
#29548 = FACE_OUTER_BOUND ( 'NONE', #9575, .T. ) ;
#29549 = LINE ( 'NONE', #29807, #34140 ) ;
#29550 = CARTESIAN_POINT ( 'NONE',  ( 31.55402655318503236, 0.000000000000000000, -117.4317124430720156 ) ) ;
#29551 = FACE_OUTER_BOUND ( 'NONE', #38194, .T. ) ;
#29552 = VERTEX_POINT ( 'NONE', #37403 ) ;
#29553 = ORIENTED_EDGE ( 'NONE', *, *, #24246, .F. ) ;
#29554 = CARTESIAN_POINT ( 'NONE',  ( 151.5540265531850537, 1.025126265847089213, -37.43171244307202272 ) ) ;
#29555 = CARTESIAN_POINT ( 'NONE',  ( 46.11867747200574996, -19.86470446310233484, -8.016098858316199838 ) ) ;
#29556 = ADVANCED_FACE ( 'NONE', ( #30695 ), #18862, .T. ) ;
#29557 = CARTESIAN_POINT ( 'NONE',  ( 130.0000000000018474, 17.00000000000000000, 90.00000000000000000 ) ) ;
#29558 = CARTESIAN_POINT ( 'NONE',  ( 10.00000000000000000, 1.224646799147353256E-15, 0.000000000000000000 ) ) ;
#29559 = ORIENTED_EDGE ( 'NONE', *, *, #8894, .T. ) ;
#29560 = DIRECTION ( 'NONE',  ( -0.000000000000000000, -1.000000000000000000, -0.000000000000000000 ) ) ;
#29562 = ORIENTED_EDGE ( 'NONE', *, *, #9663, .T. ) ;
#29561 = VECTOR ( 'NONE', #42277, 1000.000000000000000 ) ;
#29563 = SHAPE_REPRESENTATION_RELATIONSHIP ( 'NONE' , 'NONE' ,  #31369, #36305 ) ;
#29564 = EDGE_CURVE ( 'NONE', #586, #49298, #2226, .T. ) ;
#29565 = CARTESIAN_POINT ( 'NONE',  ( -125.6708471809678542, -1.749999999999996225, 159.7931612910809065 ) ) ;
#29566 = CARTESIAN_POINT ( 'NONE',  ( 1.424725715586983243, -0.8249487629949646683, 9.927568724237804787 ) ) ;
#29567 = CARTESIAN_POINT ( 'NONE',  ( -7.749480817862350435, -14.85497772329513211, 9.403735324607438884 ) ) ;
#29568 = VECTOR ( 'NONE', #15074, 1000.000000000000114 ) ;
#29569 = CARTESIAN_POINT ( 'NONE',  ( -46.69597344681494633, 0.000000000000000000, 165.0000000000000000 ) ) ;
#29570 = CARTESIAN_POINT ( 'NONE',  ( -164.9999999999990905, 17.00000000000000000, 0.000000000000000000 ) ) ;
#29571 = CARTESIAN_POINT ( 'NONE',  ( -44.94597344681493922, 1.025126265847089657, -120.9317124430720440 ) ) ;
#29572 = VERTEX_POINT ( 'NONE', #33533 ) ;
#29573 = LINE ( 'NONE', #17523, #38665 ) ;
#29575 = AXIS2_PLACEMENT_3D ( 'NONE', #46521, #11411, #23206 ) ;
#29574 = LINE ( 'NONE', #1631, #28549 ) ;
#29576 = CARTESIAN_POINT ( 'NONE',  ( -0.3862712429686895876, 1.188820645368940720, 10.00000000000000000 ) ) ;
#29577 = EDGE_CURVE ( 'NONE', #23786, #38645, #9459, .T. ) ;
#29578 = ADVANCED_FACE ( 'NONE', ( #49129 ), #26336, .T. ) ;
#29579 = ADVANCED_FACE ( 'NONE', ( #14781 ), #26076, .T. ) ;
#29580 = EDGE_CURVE ( 'NONE', #15732, #30427, #41977, .T. ) ;
#29581 = CARTESIAN_POINT ( 'NONE',  ( 355.9999999999999432, -174.9999999999999432, 355.9999999999998295 ) ) ;
#29582 = ORIENTED_EDGE ( 'NONE', *, *, #45015, .F. ) ;
#29583 = DIRECTION ( 'NONE',  ( 0.000000000000000000, 0.000000000000000000, 1.000000000000000000 ) ) ;
#29584 = VERTEX_POINT ( 'NONE', #42231 ) ;
#29585 = DIRECTION ( 'NONE',  ( -1.000000000000000000, 0.000000000000000000, 0.000000000000000000 ) ) ;
#29586 = CARTESIAN_POINT ( 'NONE',  ( 1.468713901642212161, 0.3220470327672588229, 9.927319414211225990 ) ) ;
#29587 = DIRECTION ( 'NONE',  ( 0.000000000000000000, 0.000000000000000000, 1.000000000000000000 ) ) ;
#29588 = DIRECTION ( 'NONE',  ( 0.000000000000000000, 0.000000000000000000, 1.000000000000000000 ) ) ;
#29589 = ORIENTED_EDGE ( 'NONE', *, *, #3434, .T. ) ;
#29590 = FACE_OUTER_BOUND ( 'NONE', #264, .T. ) ;
#29591 = CYLINDRICAL_SURFACE ( 'NONE', #18831, 1.750000000000008438 ) ;
#29592 = CARTESIAN_POINT ( 'NONE',  ( 16.99749102614301677, -1.320765928724307425, 8.953103998512858652 ) ) ;
#29593 = ORIENTED_EDGE ( 'NONE', *, *, #47857, .F. ) ;
#29594 = EDGE_LOOP ( 'NONE', ( #9847, #36172, #38157, #36423 ) ) ;
#29595 = EDGE_CURVE ( 'NONE', #36396, #9851, #38402, .T. ) ;
#29596 = DIRECTION ( 'NONE',  ( -1.000000000000000000, 0.000000000000000000, -0.000000000000000000 ) ) ;
#29597 = LINE ( 'NONE', #26013, #49221 ) ;
#29598 = VECTOR ( 'NONE', #23448, 1000.000000000000000 ) ;
#29599 = EDGE_CURVE ( 'NONE', #26176, #19710, #41473, .T. ) ;
#29600 = VERTEX_POINT ( 'NONE', #14010 ) ;
#29601 = EDGE_CURVE ( 'NONE', #40803, #10095, #15538, .T. ) ;
#29602 = ORIENTED_EDGE ( 'NONE', *, *, #48355, .F. ) ;
#29603 = DIRECTION ( 'NONE',  ( 0.000000000000000000, 0.000000000000000000, -1.000000000000000000 ) ) ;
#29604 = DIRECTION ( 'NONE',  ( 1.000000000000000000, 0.000000000000000000, 0.000000000000000000 ) ) ;
#29605 = DIRECTION ( 'NONE',  ( -0.000000000000000000, -0.000000000000000000, -1.000000000000000000 ) ) ;
#29606 = CARTESIAN_POINT ( 'NONE',  ( -69.99999999999940314, 16.00000000000000000, -54.99999999999999289 ) ) ;
#29607 = ORIENTED_EDGE ( 'NONE', *, *, #6752, .T. ) ;
#29608 = CARTESIAN_POINT ( 'NONE',  ( 73.30402655318508209, 1.750000000000010658, 80.81828755692798438 ) ) ;
#29609 = ADVANCED_FACE ( 'NONE', ( #34287 ), #34044, .F. ) ;
#29610 = VERTEX_POINT ( 'NONE', #6331 ) ;
#29611 = AXIS2_PLACEMENT_3D ( 'NONE', #15568, #11222, #3764 ) ;
#29612 = CIRCLE ( 'NONE', #18136, 1.750000000000015543 ) ;
#29613 = ADVANCED_FACE ( 'NONE', ( #37647 ), #14522, .T. ) ;
#29614 = CYLINDRICAL_SURFACE ( 'NONE', #28335, 1.750000000000008438 ) ;
#29615 = DIRECTION ( 'NONE',  ( 0.000000000000000000, 0.000000000000000000, 1.000000000000000000 ) ) ;
#29616 = ORIENTED_EDGE ( 'NONE', *, *, #39701, .F. ) ;
#29617 = ORIENTED_EDGE ( 'NONE', *, *, #41058, .T. ) ;
#29618 = CARTESIAN_POINT ( 'NONE',  ( -4.945973446814903696, 2.143131898507912917E-16, 159.0682875569279418 ) ) ;
#29619 =( BOUNDED_CURVE ( )  B_SPLINE_CURVE ( 3, ( #29833, #18261, #22130, #21117 ),
 .UNSPECIFIED., .F., .F. ) 
 B_SPLINE_CURVE_WITH_KNOTS ( ( 4, 4 ),
 ( 4.712388980384689674, 6.283185307179586232 ),
 .UNSPECIFIED. ) 
 CURVE ( )  GEOMETRIC_REPRESENTATION_ITEM ( )  RATIONAL_B_SPLINE_CURVE ( ( 1.000000000000000000, 0.8047378541243649375, 0.8047378541243649375, 1.000000000000000000 ) ) 
 REPRESENTATION_ITEM ( '' )  );
#29620 = VERTEX_POINT ( 'NONE', #10675 ) ;
#29621 = CARTESIAN_POINT ( 'NONE',  ( -10.01251772323708522, 8.486842105263161073, -18.46084505325461578 ) ) ;
#29622 = VERTEX_POINT ( 'NONE', #18118 ) ;
#29623 = DIRECTION ( 'NONE',  ( 0.000000000000000000, 0.2223603367690656640, 0.9749645535258950613 ) ) ;
#29624 = ORIENTED_EDGE ( 'NONE', *, *, #28439, .F. ) ;
#29625 = LINE ( 'NONE', #26038, #39789 ) ;
#29626 = CARTESIAN_POINT ( 'NONE',  ( -119.9999999999997158, 17.00000000000000000, -84.99999999999998579 ) ) ;
#29627 = DIRECTION ( 'NONE',  ( 0.000000000000000000, 0.000000000000000000, -1.000000000000000000 ) ) ;
#29628 = CARTESIAN_POINT ( 'NONE',  ( 0.000000000000000000, 169.0000000000000000, 357.9999999999997726 ) ) ;
#29629 = ADVANCED_FACE ( 'NONE', ( #38153 ), #44112, .T. ) ;
#29630 = ORIENTED_EDGE ( 'NONE', *, *, #3960, .T. ) ;
#29631 = DIRECTION ( 'NONE',  ( 0.4374820812098791922, 0.3178493372392781069, 0.8411784753765542133 ) ) ;
#29632 = DIRECTION ( 'NONE',  ( -1.000000000000000000, -0.000000000000000000, -0.000000000000000000 ) ) ;
#29633 = CARTESIAN_POINT ( 'NONE',  ( 71.55402655318505367, 0.000000000000000000, -117.4317124430720156 ) ) ;
#29634 = CARTESIAN_POINT ( 'NONE',  ( -37.09503908879538159, 5.733418411339063603, 4.835783797351798086 ) ) ;
#29635 = EDGE_CURVE ( 'NONE', #1211, #16952, #12885, .T. ) ;
#29636 = ADVANCED_FACE ( 'NONE', ( #15303, #9052 ), #47996, .F. ) ;
#29637 = EDGE_CURVE ( 'NONE', #6876, #35009, #7009, .T. ) ;
#29638 = CARTESIAN_POINT ( 'NONE',  ( 9.999999999999998224, 8.486842105263161073, -18.34680996553532140 ) ) ;
#29639 = LINE ( 'NONE', #18327, #17952 ) ;
#29640 = VECTOR ( 'NONE', #12411, 1000.000000000000000 ) ;
#29641 = EDGE_CURVE ( 'NONE', #4392, #50192, #5190, .T. ) ;
#29642 = CARTESIAN_POINT ( 'NONE',  ( 164.9999999999999716, 17.00000000000000000, 59.99999999999999289 ) ) ;
#29643 = DIRECTION ( 'NONE',  ( -1.000000000000000000, 0.000000000000000000, 0.000000000000000000 ) ) ;
#29644 = EDGE_CURVE ( 'NONE', #2629, #29259, #34573, .T. ) ;
#29645 = VECTOR ( 'NONE', #46341, 1000.000000000000000 ) ;
#29646 = DIRECTION ( 'NONE',  ( -1.000000000000000000, -0.000000000000000000, -0.000000000000000000 ) ) ;
#29647 = ORIENTED_EDGE ( 'NONE', *, *, #30240, .T. ) ;
#29648 = DIRECTION ( 'NONE',  ( 0.000000000000000000, -1.000000000000000000, -1.544785076050074834E-48 ) ) ;
#29649 = CARTESIAN_POINT ( 'NONE',  ( -30.77287599203642188, -12.70002479445974686, 3.199614146704519602 ) ) ;
#29650 = CARTESIAN_POINT ( 'NONE',  ( 85.00000000000152056, 16.00000000000000000, 35.00000000000000000 ) ) ;
#29651 = FACE_OUTER_BOUND ( 'NONE', #13447, .T. ) ;
#29652 = FACE_OUTER_BOUND ( 'NONE', #9760, .T. ) ;
#29653 = ORIENTED_EDGE ( 'NONE', *, *, #36982, .T. ) ;
#29654 = VERTEX_POINT ( 'NONE', #23505 ) ;
#29655 = CARTESIAN_POINT ( 'NONE',  ( 75.05402655318509630, 1.025126265847089657, 42.56828755692799149 ) ) ;
#29656 = CARTESIAN_POINT ( 'NONE',  ( 1.780432407520001536, 1.041450996408479046, 9.894754715216729224 ) ) ;
#29657 = ORIENTED_EDGE ( 'NONE', *, *, #49872, .T. ) ;
#29658 = EDGE_CURVE ( 'NONE', #36434, #28673, #48529, .T. ) ;
#29659 = CARTESIAN_POINT ( 'NONE',  ( 0.3370904143228947158, 0.2449105217885311492, 10.00000000000000000 ) ) ;
#29660 = CARTESIAN_POINT ( 'NONE',  ( 153.3040265531850537, 0.000000000000000000, 165.0000000000000000 ) ) ;
#29661 = ORIENTED_EDGE ( 'NONE', *, *, #5113, .F. ) ;
#29662 = VERTEX_POINT ( 'NONE', #13140 ) ;
#29663 = VECTOR ( 'NONE', #30319, 1000.000000000000000 ) ;
#29664 = ORIENTED_EDGE ( 'NONE', *, *, #26185, .T. ) ;
#29665 = PRODUCT_DEFINITION ( 'UNKNOWN', '', #450, #27803 ) ;
#29666 = VECTOR ( 'NONE', #5469, 1000.000000000000000 ) ;
#29667 = CARTESIAN_POINT ( 'NONE',  ( 75.05402655318509630, -1.025126265847089657, 119.0682875569279560 ) ) ;
#29668 = CARTESIAN_POINT ( 'NONE',  ( 36.80807479611532784, -7.357694319819502837, 1.982731392810463067 ) ) ;
#29669 = CARTESIAN_POINT ( 'NONE',  ( 35.05402655318504657, 2.143131898507880377E-16, 165.0000000000000000 ) ) ;
#29670 = ORIENTED_EDGE ( 'NONE', *, *, #6692, .T. ) ;
#29671 = DIRECTION ( 'NONE',  ( -1.000000000000000000, 0.000000000000000000, -1.612977847700450206E-50 ) ) ;
#29672 = VECTOR ( 'NONE', #7977, 1000.000000000000000 ) ;
#29673 = CARTESIAN_POINT ( 'NONE',  ( 0.000000000000000000, 0.000000000000000000, -240.0000000000000000 ) ) ;
#29674 = FILL_AREA_STYLE ('',( #49866 ) ) ;
#29675 = VERTEX_POINT ( 'NONE', #42717 ) ;
#29676 = EDGE_LOOP ( 'NONE', ( #14456, #33186, #36720, #47968 ) ) ;
#29677 = DIRECTION ( 'NONE',  ( -0.000000000000000000, -1.000000000000000000, 2.537652627714643577E-15 ) ) ;
#29678 = ADVANCED_FACE ( 'NONE', ( #23756 ), #28801, .F. ) ;
#29679 = CARTESIAN_POINT ( 'NONE',  ( 0.9983599181300923942, 1.124146016603553733, 9.953784399990620813 ) ) ;
#29680 = DIRECTION ( 'NONE',  ( -0.000000000000000000, -0.000000000000000000, -1.000000000000000000 ) ) ;
#29681 = ORIENTED_EDGE ( 'NONE', *, *, #10300, .T. ) ;
#29682 = CARTESIAN_POINT ( 'NONE',  ( -206.6959734468149463, -1.750000000000010658, -119.1817124430720440 ) ) ;
#29683 = DIRECTION ( 'NONE',  ( 0.000000000000000000, 0.000000000000000000, -1.000000000000000000 ) ) ;
#29684 = CARTESIAN_POINT ( 'NONE',  ( 2.052581215100350853, -0.2042358160480859663, 9.886433018048069954 ) ) ;
#29685 = CARTESIAN_POINT ( 'NONE',  ( -44.94597344681493922, 2.143131898507880377E-16, -160.9317124430720582 ) ) ;
#29686 = EDGE_CURVE ( 'NONE', #18457, #39326, #32651, .T. ) ;
#29687 = LINE ( 'NONE', #17876, #11005 ) ;
#29688 = DIRECTION ( 'NONE',  ( -1.586032892321652236E-16, -1.000000000000000000, -6.853681917100419162E-49 ) ) ;
#29689 = LINE ( 'NONE', #7108, #34078 ) ;
#29690 = CIRCLE ( 'NONE', #32158, 4.000000000000003553 ) ;
#29691 = DIRECTION ( 'NONE',  ( -1.000000000000000000, -0.000000000000000000, -0.000000000000000000 ) ) ;
#29692 = CARTESIAN_POINT ( 'NONE',  ( 1.211301556933464862, 0.1727733738854638212, 9.993783931180534097 ) ) ;
#29693 = CARTESIAN_POINT ( 'NONE',  ( 193.3040265531851105, 1.750000000000010658, 80.81828755692798438 ) ) ;
#29694 = EDGE_CURVE ( 'NONE', #20602, #41952, #3739, .T. ) ;
#29695 = EDGE_CURVE ( 'NONE', #25164, #41719, #33401, .T. ) ;
#29696 =( BOUNDED_CURVE ( )  B_SPLINE_CURVE ( 3, ( #18312, #33992, #2184, #49579 ),
 .UNSPECIFIED., .F., .F. ) 
 B_SPLINE_CURVE_WITH_KNOTS ( ( 4, 4 ),
 ( 1.570796326794896558, 3.141592653589793116 ),
 .UNSPECIFIED. ) 
 CURVE ( )  GEOMETRIC_REPRESENTATION_ITEM ( )  RATIONAL_B_SPLINE_CURVE ( ( 1.000000000000000000, 0.8047378541243649375, 0.8047378541243649375, 1.000000000000000000 ) ) 
 REPRESENTATION_ITEM ( '' )  );
#29697 = LINE ( 'NONE', #49151, #19143 ) ;
#29698=STYLED_ITEM('',(#50775),#5532);
#29699 = ORIENTED_EDGE ( 'NONE', *, *, #35359, .F. ) ;
#29700 = DIRECTION ( 'NONE',  ( 0.000000000000000000, 0.000000000000000000, 1.000000000000000000 ) ) ;
#29701 = VECTOR ( 'NONE', #33925, 1000.000000000000000 ) ;
#29702 = ADVANCED_FACE ( 'NONE', ( #35074 ), #20776, .T. ) ;
#29703 = CARTESIAN_POINT ( 'NONE',  ( 35.00000000000186162, 17.00000000000000000, 65.00000000000000000 ) ) ;
#29704 = CARTESIAN_POINT ( 'NONE',  ( -4.353119224255007857, -9.002796955359011477, 0.000000000000000000 ) ) ;
#29705 = ADVANCED_FACE ( 'NONE', ( #9295 ), #9549, .T. ) ;
#29706 = ADVANCED_FACE ( 'NONE', ( #29548 ), #17251, .F. ) ;
#29707 = ORIENTED_EDGE ( 'NONE', *, *, #24296, .F. ) ;
#29708 = LINE ( 'NONE', #25611, #10079 ) ;
#29709 = VECTOR ( 'NONE', #6888, 1000.000000000000000 ) ;
#29710 = FACE_OUTER_BOUND ( 'NONE', #10678, .T. ) ;
#29711 = ORIENTED_EDGE ( 'NONE', *, *, #37796, .T. ) ;
#29712 = DIRECTION ( 'NONE',  ( -0.000000000000000000, 1.000000000000000000, 0.000000000000000000 ) ) ;
#29713 = DIRECTION ( 'NONE',  ( -0.000000000000000000, -0.000000000000000000, -1.000000000000000000 ) ) ;
#29714 = CARTESIAN_POINT ( 'NONE',  ( 210.0000000000000568, 2.143131898507881856E-16, -80.93171244307202983 ) ) ;
#29715 = CARTESIAN_POINT ( 'NONE',  ( -84.94597344681494633, 2.143131898507880377E-16, 165.0000000000000000 ) ) ;
#29716 = EDGE_CURVE ( 'NONE', #17436, #3012, #24095, .T. ) ;
#29717 = ORIENTED_EDGE ( 'NONE', *, *, #43706, .T. ) ;
#29718 = CARTESIAN_POINT ( 'NONE',  ( 181.0000000000000000, -268.4999999999999432, -349.9999999999999432 ) ) ;
#29719 = B_SPLINE_SURFACE_WITH_KNOTS ( 'NONE', 3, 3, ( 
 ( #40143, #16539, #16789, #44218 ),
 ( #47789, #20885, #1649, #48290 ),
 ( #40889, #4978, #24999, #44715 ),
 ( #40400, #17290, #12676, #43968 ) ),
 .UNSPECIFIED., .F., .F., .F.,
 ( 4, 4 ),
 ( 4, 4 ),
 ( 0.000000000000000000, 1.000000000000000000 ),
 ( 0.000000000000000000, 1.000000000000000000 ),
 .UNSPECIFIED. ) ;
#29720 = EDGE_LOOP ( 'NONE', ( #45918, #39278, #43777, #11359, #33763, #42881 ) ) ;
#29721 = EDGE_LOOP ( 'NONE', ( #19883, #39954, #38920, #39317 ) ) ;
#29722 = DIRECTION ( 'NONE',  ( -1.000000000000000000, 0.000000000000000000, 0.000000000000000000 ) ) ;
#29723 = VERTEX_POINT ( 'NONE', #32917 ) ;
#29724 = CARTESIAN_POINT ( 'NONE',  ( 85.00000000000056843, 17.00000000000000000, -30.00000000000000000 ) ) ;
#29725 = DIRECTION ( 'NONE',  ( 0.000000000000000000, -1.000000000000000000, 0.000000000000000000 ) ) ;
#29726 = ORIENTED_EDGE ( 'NONE', *, *, #17680, .F. ) ;
#29727 = CARTESIAN_POINT ( 'NONE',  ( -128.4459734468149179, 2.143131898507880377E-16, -160.9317124430720298 ) ) ;
#29728 = CARTESIAN_POINT ( 'NONE',  ( 164.9999999999999716, -272.4999999999999432, -343.9999999999999432 ) ) ;
#29729 = AXIS2_PLACEMENT_3D ( 'NONE', #40101, #4433, #9047 ) ;
#29730 = CARTESIAN_POINT ( 'NONE',  ( 3.808200756227633654, 0.8261963378076531139, 9.741991644047248045 ) ) ;
#29731 = ORIENTED_EDGE ( 'NONE', *, *, #1507, .T. ) ;
#29732 = DIRECTION ( 'NONE',  ( 1.387778780781444256E-14, -0.000000000000000000, 1.000000000000000000 ) ) ;
#29733 = DIRECTION ( 'NONE',  ( 0.000000000000000000, -1.000000000000000000, 0.000000000000000000 ) ) ;
#29734 = CARTESIAN_POINT ( 'NONE',  ( 85.00000000000213163, 17.00000000000000000, 95.00000000000000000 ) ) ;
#29735 = EDGE_LOOP ( 'NONE', ( #29056, #45985, #7282, #2691 ) ) ;
#29736 = CARTESIAN_POINT ( 'NONE',  ( 9.358026734184097251, 3.388353563403873350E-15, -22.00000000000000000 ) ) ;
#29737 = CARTESIAN_POINT ( 'NONE',  ( -54.99999999999997868, -52.50000000000000711, 5.000000000000000000 ) ) ;
#29738 = VERTEX_POINT ( 'NONE', #2108 ) ;
#29739 = ORIENTED_EDGE ( 'NONE', *, *, #33972, .F. ) ;
#29740 = VERTEX_POINT ( 'NONE', #44666 ) ;
#29741 = LINE ( 'NONE', #45357, #25438 ) ;
#29742 = AXIS2_PLACEMENT_3D ( 'NONE', #9491, #14091, #40801 ) ;
#29743 = CARTESIAN_POINT ( 'NONE',  ( -1.011271242968693862, 0.7347315653655780432, -10.00000000000000000 ) ) ;
#29744 = ORIENTED_EDGE ( 'NONE', *, *, #26413, .T. ) ;
#29746 = ADVANCED_FACE ( 'NONE', ( #48994 ), #48500, .T. ) ;
#29745 = AXIS2_PLACEMENT_3D ( 'NONE', #7123, #33823, #26870 ) ;
#29747 = LINE ( 'NONE', #22041, #29856 ) ;
#29748 = SURFACE_STYLE_FILL_AREA ( #9236 ) ;
#29749 = FACE_BOUND ( 'NONE', #1034, .T. ) ;
#29750 = CARTESIAN_POINT ( 'NONE',  ( 195.0540265531851105, -1.025126265847088991, 2.568287556927986159 ) ) ;
#29751 = VECTOR ( 'NONE', #45878, 1000.000000000000000 ) ;
#29752 = ORIENTED_EDGE ( 'NONE', *, *, #11084, .T. ) ;
#29753 = DIRECTION ( 'NONE',  ( 0.000000000000000000, 0.000000000000000000, -1.000000000000000000 ) ) ;
#29754 = LINE ( 'NONE', #5387, #33308 ) ;
#29755 = CARTESIAN_POINT ( 'NONE',  ( 341.9999999999999432, 174.9999999999996589, -344.0000000000002842 ) ) ;
#29756 = ORIENTED_EDGE ( 'NONE', *, *, #35248, .F. ) ;
#29757 = CARTESIAN_POINT ( 'NONE',  ( 164.9999999999999716, -268.5000000000000000, -339.9999999999998863 ) ) ;
#29758 =( BOUNDED_CURVE ( )  B_SPLINE_CURVE ( 3, ( #24453, #44419, #44173, #16737 ),
 .UNSPECIFIED., .F., .F. ) 
 B_SPLINE_CURVE_WITH_KNOTS ( ( 4, 4 ),
 ( 4.712388980384689674, 6.283185307179586232 ),
 .UNSPECIFIED. ) 
 CURVE ( )  GEOMETRIC_REPRESENTATION_ITEM ( )  RATIONAL_B_SPLINE_CURVE ( ( 1.000000000000000000, 0.8047378541243649375, 0.8047378541243649375, 1.000000000000000000 ) ) 
 REPRESENTATION_ITEM ( '' )  );
#29759 = CARTESIAN_POINT ( 'NONE',  ( -36.28567981536816234, -9.465698090293395595, -9.422646554964174470 ) ) ;
#29760 = EDGE_CURVE ( 'NONE', #21529, #25320, #10052, .T. ) ;
#29761 = EDGE_CURVE ( 'NONE', #8521, #5511, #4749, .T. ) ;
#29762 = CARTESIAN_POINT ( 'NONE',  ( 153.2026953830863647, 103.0380105690400683, -17.65743994998277699 ) ) ;
#29763 = DIRECTION ( 'NONE',  ( 0.000000000000000000, 1.000000000000000000, 8.673617379884027583E-15 ) ) ;
#29764 = ORIENTED_EDGE ( 'NONE', *, *, #33765, .F. ) ;
#29765 = DIRECTION ( 'NONE',  ( 0.000000000000000000, -2.537652627714643577E-15, -1.000000000000000000 ) ) ;
#29766 = CARTESIAN_POINT ( 'NONE',  ( -36.63544619771738553, -20.34968343020614512, 7.544061037322998153 ) ) ;
#29767 =( BOUNDED_CURVE ( )  B_SPLINE_CURVE ( 3, ( #43784, #32011, #4036, #12744 ),
 .UNSPECIFIED., .F., .F. ) 
 B_SPLINE_CURVE_WITH_KNOTS ( ( 4, 4 ),
 ( 1.570796326794896558, 3.141592653589793116 ),
 .UNSPECIFIED. ) 
 CURVE ( )  GEOMETRIC_REPRESENTATION_ITEM ( )  RATIONAL_B_SPLINE_CURVE ( ( 1.000000000000000000, 0.8047378541243649375, 0.8047378541243649375, 1.000000000000000000 ) ) 
 REPRESENTATION_ITEM ( '' )  );
#29768 = LINE ( 'NONE', #36999, #15507 ) ;
#29769 = DIRECTION ( 'NONE',  ( 0.000000000000000000, 0.000000000000000000, 1.000000000000000000 ) ) ;
#29770 = EDGE_CURVE ( 'NONE', #21356, #1069, #3917, .T. ) ;
#29771 = ADVANCED_FACE ( 'NONE', ( #33421 ), #29305, .T. ) ;
#29772 = VERTEX_POINT ( 'NONE', #44910 ) ;
#29773 = CARTESIAN_POINT ( 'NONE',  ( 181.0000000000000000, -184.9999999999999716, -350.0000000000001705 ) ) ;
#29774 = ORIENTED_EDGE ( 'NONE', *, *, #45840, .F. ) ;
#29775 = LINE ( 'NONE', #9763, #16382 ) ;
#29776 = AXIS2_PLACEMENT_3D ( 'NONE', #28466, #29461, #5090 ) ;
#29777 = ORIENTED_EDGE ( 'NONE', *, *, #21532, .T. ) ;
#29778 = EDGE_CURVE ( 'NONE', #16880, #45973, #41100, .T. ) ;
#29779 = CARTESIAN_POINT ( 'NONE',  ( 1.249999999999999778, 0.000000000000000000, 9.972675548442463622 ) ) ;
#29780 = AXIS2_PLACEMENT_3D ( 'NONE', #8872, #44257, #1194 ) ;
#29781 = CARTESIAN_POINT ( 'NONE',  ( -125.6708471809678542, -1.749999999999996669, 161.8434138227750907 ) ) ;
#29782 =( BOUNDED_CURVE ( )  B_SPLINE_CURVE ( 3, ( #19022, #25739, #21888, #42122 ),
 .UNSPECIFIED., .F., .F. ) 
 B_SPLINE_CURVE_WITH_KNOTS ( ( 4, 4 ),
 ( 1.570796326794896558, 3.141592653589793116 ),
 .UNSPECIFIED. ) 
 CURVE ( )  GEOMETRIC_REPRESENTATION_ITEM ( )  RATIONAL_B_SPLINE_CURVE ( ( 1.000000000000000000, 0.8047378541243649375, 0.8047378541243649375, 1.000000000000000000 ) ) 
 REPRESENTATION_ITEM ( '' )  );
#29783 = CARTESIAN_POINT ( 'NONE',  ( -215.0000000000000568, -165.2931214222915344, 497.2965085865002948 ) ) ;
#29784 = VERTEX_POINT ( 'NONE', #17499 ) ;
#29785 = MECHANICAL_DESIGN_GEOMETRIC_PRESENTATION_REPRESENTATION (  '', ( #12560 ), #32246 ) ;
#29786 = DIRECTION ( 'NONE',  ( -1.000000000000000000, 0.000000000000000000, 0.000000000000000000 ) ) ;
#29787 = AXIS2_PLACEMENT_3D ( 'NONE', #23973, #39628, #20114 ) ;
#29788 = ORIENTED_EDGE ( 'NONE', *, *, #1116, .T. ) ;
#29789 = CARTESIAN_POINT ( 'NONE',  ( -166.6959734468149463, 1.750000000000010658, 80.81828755692798438 ) ) ;
#29790 = CARTESIAN_POINT ( 'NONE',  ( 340.0000000000000568, 166.6568542494923975, 341.6568542494921417 ) ) ;
#29791 = CARTESIAN_POINT ( 'NONE',  ( 0.000000000000000000, -175.0000000000000284, 350.0000000000002274 ) ) ;
#29792 = LINE ( 'NONE', #50241, #33291 ) ;
#29793 = DIRECTION ( 'NONE',  ( 0.6805276818820402696, 0.4944323023722069221, 0.5407575913134970991 ) ) ;
#29794 = EDGE_LOOP ( 'NONE', ( #30178, #9158, #23798, #11242 ) ) ;
#29795 = VERTEX_POINT ( 'NONE', #14137 ) ;
#29796 = AXIS2_PLACEMENT_3D ( 'NONE', #6774, #25775, #49321 ) ;
#29797 = ORIENTED_EDGE ( 'NONE', *, *, #35190, .T. ) ;
#29798 = CARTESIAN_POINT ( 'NONE',  ( 5.083187235775197266, 8.611690166631179366, 9.646707543097347681 ) ) ;
#29799 = CARTESIAN_POINT ( 'NONE',  ( -127.7210997126620242, -1.749999999999996891, 121.8434138227750481 ) ) ;
#29800 = VERTEX_POINT ( 'NONE', #29805 ) ;
#29801 = CARTESIAN_POINT ( 'NONE',  ( 1.468713901642212161, 0.3220470327672588229, 9.927319414211225990 ) ) ;
#29802 = B_SPLINE_CURVE_WITH_KNOTS ( 'NONE', 3,
 ( #31871, #46699, #26988, #7503 ),
 .UNSPECIFIED., .F., .F.,
 ( 4, 4 ),
 ( 0.000000000000000000, 0.002466147708923230146 ),
 .UNSPECIFIED. ) ;
#29803 = CARTESIAN_POINT ( 'NONE',  ( -44.94597344681493922, 2.143131898507882349E-16, -165.0000000000000000 ) ) ;
#29804 = ORIENTED_EDGE ( 'NONE', *, *, #38948, .F. ) ;
#29805 = CARTESIAN_POINT ( 'NONE',  ( -215.0000000000000568, -175.0000000000000000, 10.00000000000000000 ) ) ;
#29806 = EDGE_CURVE ( 'NONE', #35123, #31511, #6390, .T. ) ;
#29807 = CARTESIAN_POINT ( 'NONE',  ( 210.0000000000000568, 0.000000000000000000, -37.43171244307202272 ) ) ;
#29808 = CARTESIAN_POINT ( 'NONE',  ( -168.4459734468149463, 0.000000000000000000, 165.0000000000000000 ) ) ;
#29809 = DIRECTION ( 'NONE',  ( 4.996003610813203446E-16, 1.000000000000000000, 0.000000000000000000 ) ) ;
#29810 = PLANE ( 'NONE',  #39505 ) ;
#29811 = EDGE_LOOP ( 'NONE', ( #28367, #11310, #4505, #18892, #43688, #6816 ) ) ;
#29812 = ORIENTED_EDGE ( 'NONE', *, *, #81, .F. ) ;
#29813 = AXIS2_PLACEMENT_3D ( 'NONE', #10785, #42580, #30296 ) ;
#29814 = PLANE ( 'NONE',  #12971 ) ;
#29815 = CARTESIAN_POINT ( 'NONE',  ( 9.999999999999996447, -34.54492135858216528, 0.000000000000000000 ) ) ;
#29816 = VECTOR ( 'NONE', #41808, 1000.000000000000000 ) ;
#29817 = CARTESIAN_POINT ( 'NONE',  ( -119.9999999999978400, 16.00000000000000000, 115.0000000000000142 ) ) ;
#29818 = CARTESIAN_POINT ( 'NONE',  ( 73.30402655318508209, -1.750000000000009992, 0.8182875569279768335 ) ) ;
#29819 = VERTEX_POINT ( 'NONE', #40019 ) ;
#29820 = AXIS2_PLACEMENT_3D ( 'NONE', #44028, #39203, #43280 ) ;
#29821 = DIRECTION ( 'NONE',  ( -1.000000000000000000, 1.586032997072805650E-16, 4.759647537211363479E-16 ) ) ;
#29822 = ORIENTED_EDGE ( 'NONE', *, *, #15418, .T. ) ;
#29823 = VECTOR ( 'NONE', #48141, 1000.000000000000227 ) ;
#29824 = CARTESIAN_POINT ( 'NONE',  ( 6.619412807845094449, -7.495556955913033725, 9.646707543097347681 ) ) ;
#29825 = CYLINDRICAL_SURFACE ( 'NONE', #45688, 1.750000000000001554 ) ;
#29826 = CARTESIAN_POINT ( 'NONE',  ( 1.011271242968688311, -0.7347315653655855927, 10.00000000000000000 ) ) ;
#29827 = DIRECTION ( 'NONE',  ( -1.000000000000000000, 0.000000000000000000, -7.793956916774525800E-48 ) ) ;
#29828 = CARTESIAN_POINT ( 'NONE',  ( 340.5182995536247859, 2.688010569040066411, 224.7724958161645077 ) ) ;
#29829 = CARTESIAN_POINT ( 'NONE',  ( -46.69597344681494633, 1.750000000000010658, -119.1817124430720440 ) ) ;
#29830 = ORIENTED_EDGE ( 'NONE', *, *, #32504, .F. ) ;
#29831 = CARTESIAN_POINT ( 'NONE',  ( -194.9999999999999432, -173.0000000000000000, 112.0000000000000284 ) ) ;
#29832 = PRODUCT ( 'tire 1', 'tire 1', '', ( #39810 ) ) ;
#29833 = CARTESIAN_POINT ( 'NONE',  ( 33.30402655318503946, -1.750000000000010214, -39.18171244307202983 ) ) ;
#29834 = CARTESIAN_POINT ( 'NONE',  ( 0.09523839817332763191, 1.466467394239034050, 9.958264684458713489 ) ) ;
#29835 = VECTOR ( 'NONE', #23833, 1000.000000000000000 ) ;
#29836 = CARTESIAN_POINT ( 'NONE',  ( 49.89397392339123627, -8.245536726716670373, 7.906207997025717304 ) ) ;
#29837 = EDGE_LOOP ( 'NONE', ( #25452, #39224, #39917, #1144, #7462 ) ) ;
#29838 = CARTESIAN_POINT ( 'NONE',  ( -30.22736451279196856, -39.84193304692609416, -2.408242355805840784 ) ) ;
#29839 = VERTEX_POINT ( 'NONE', #36431 ) ;
#29840 = EDGE_CURVE ( 'NONE', #27056, #35523, #48408, .T. ) ;
#29841 = B_SPLINE_CURVE_WITH_KNOTS ( 'NONE', 3,
 ( #37469, #18434, #22543, #42300 ),
 .UNSPECIFIED., .F., .F.,
 ( 4, 4 ),
 ( 0.000000000000000000, 0.2637263876330691592 ),
 .UNSPECIFIED. ) ;
#29842 = DIRECTION ( 'NONE',  ( 0.6805276818820432672, -0.4944323023722019261, -0.5407575913134976542 ) ) ;
#29843 = CARTESIAN_POINT ( 'NONE',  ( 1.468535767197692188, 0.3224370614409108327, 9.944962737616616977 ) ) ;
#29844 = DIRECTION ( 'NONE',  ( 0.000000000000000000, 0.000000000000000000, 1.000000000000000000 ) ) ;
#29845 = ORIENTED_EDGE ( 'NONE', *, *, #39944, .T. ) ;
#29846 = DIRECTION ( 'NONE',  ( -0.000000000000000000, -0.000000000000000000, -1.000000000000000000 ) ) ;
#29847 = ORIENTED_EDGE ( 'NONE', *, *, #48489, .T. ) ;
#29848 = CARTESIAN_POINT ( 'NONE',  ( 195.0540265531851105, -1.025126265847088991, 159.0682875569279418 ) ) ;
#29849 = VECTOR ( 'NONE', #4246, 1000.000000000000000 ) ;
#29850 = DIRECTION ( 'NONE',  ( 0.000000000000000000, 0.000000000000000000, 1.000000000000000000 ) ) ;
#29851 = CARTESIAN_POINT ( 'NONE',  ( 0.1287570809895575430, 0.3962735484563150168, 10.00000000000000000 ) ) ;
#29852 = AXIS2_PLACEMENT_3D ( 'NONE', #11551, #7960, #28212 ) ;
#29853 = ORIENTED_EDGE ( 'NONE', *, *, #43053, .F. ) ;
#29854 = EDGE_LOOP ( 'NONE', ( #11275, #18987, #24899, #24765 ) ) ;
#29855 = LINE ( 'NONE', #46219, #10373 ) ;
#29856 = VECTOR ( 'NONE', #49452, 1000.000000000000000 ) ;
#29857 = CARTESIAN_POINT ( 'NONE',  ( 35.00000000000061107, 17.00000000000000000, -54.99999999999999289 ) ) ;
#29858 = VERTEX_POINT ( 'NONE', #4612 ) ;
#29859 = ORIENTED_EDGE ( 'NONE', *, *, #33199, .F. ) ;
#29860 = CARTESIAN_POINT ( 'NONE',  ( 35.05402655318504657, 1.025126265847089657, -120.9317124430720440 ) ) ;
#29861 = CARTESIAN_POINT ( 'NONE',  ( 7.499999999999996447, 194.9999999999999716, -240.0000000000000000 ) ) ;
#29862 = PLANE ( 'NONE',  #10028 ) ;
#29863 = ORIENTED_EDGE ( 'NONE', *, *, #45662, .T. ) ;
#29864 = CARTESIAN_POINT ( 'NONE',  ( 85.00000000000213163, 16.00000000000000000, 115.0000000000000142 ) ) ;
#29865 = ORIENTED_EDGE ( 'NONE', *, *, #26994, .F. ) ;
#29866 = FACE_OUTER_BOUND ( 'NONE', #10180, .T. ) ;
#29867 = CARTESIAN_POINT ( 'NONE',  ( 2.500000000000000444, 224.9999999999999716, -240.0000000000000000 ) ) ;
#29868 = AXIS2_PLACEMENT_3D ( 'NONE', #26479, #41625, #2372 ) ;
#29869 = EDGE_LOOP ( 'NONE', ( #46781, #2751, #3758, #34579, #2832, #29997 ) ) ;
#29870 = ORIENTED_EDGE ( 'NONE', *, *, #453, .T. ) ;
#29871 = AXIS2_PLACEMENT_3D ( 'NONE', #15382, #31037, #26673 ) ;
#29872 = CARTESIAN_POINT ( 'NONE',  ( 210.0000000000000568, 0.000000000000000000, 42.56828755692799149 ) ) ;
#29873 = CARTESIAN_POINT ( 'NONE',  ( 30.00000000000123279, 17.00000000000000000, 5.000000000000004441 ) ) ;
#29874 = ORIENTED_EDGE ( 'NONE', *, *, #27321, .T. ) ;
#29875 = DIRECTION ( 'NONE',  ( -1.000000000000000000, -0.000000000000000000, -0.000000000000000000 ) ) ;
#29876 = EDGE_LOOP ( 'NONE', ( #8983, #28775, #4775, #37336 ) ) ;
#29877 = DIRECTION ( 'NONE',  ( 0.000000000000000000, -0.000000000000000000, 1.000000000000000000 ) ) ;
#29878 = ORIENTED_EDGE ( 'NONE', *, *, #596, .T. ) ;
#29879 = FACE_OUTER_BOUND ( 'NONE', #7581, .T. ) ;
#29880 = DIRECTION ( 'NONE',  ( 0.000000000000000000, 1.000000000000000000, 0.000000000000000000 ) ) ;
#29881 = CARTESIAN_POINT ( 'NONE',  ( -0.9300423221600405688, -1.714483250866335240, 9.896382706792437034 ) ) ;
#29882 = CARTESIAN_POINT ( 'NONE',  ( -86.69597344681494633, 1.750000000000009992, -159.1817124430720298 ) ) ;
#29883 = VECTOR ( 'NONE', #26387, 1000.000000000000000 ) ;
#29884 = LINE ( 'NONE', #17826, #4485 ) ;
#29885 = VERTEX_POINT ( 'NONE', #20254 ) ;
#29886 = CARTESIAN_POINT ( 'NONE',  ( -126.6959734468149321, 1.749999999999996891, -159.1817124430720298 ) ) ;
#29887 = DIRECTION ( 'NONE',  ( -0.000000000000000000, -0.000000000000000000, -1.000000000000000000 ) ) ;
#29888 = CARTESIAN_POINT ( 'NONE',  ( -168.4459734468149747, 1.025126265847088991, -157.4317124430720582 ) ) ;
#29889 = CARTESIAN_POINT ( 'NONE',  ( -31.28977333267361871, 11.25592690310926969, -2.408242355805840784 ) ) ;
#29890 = AXIS2_PLACEMENT_3D ( 'NONE', #36340, #12950, #9120 ) ;
#29891 = EDGE_CURVE ( 'NONE', #35576, #2845, #1518, .T. ) ;
#29892 = CARTESIAN_POINT ( 'NONE',  ( -1.721971274562257515, -0.09408549481333014497, 9.928159647716187308 ) ) ;
#29893 = CARTESIAN_POINT ( 'NONE',  ( 350.0000000000001137, 181.0000000000000284, 343.9999999999997726 ) ) ;
#29894 = CARTESIAN_POINT ( 'NONE',  ( 151.5540265531850537, 0.000000000000000000, -0.9317124430720247208 ) ) ;
#29895 = CARTESIAN_POINT ( 'NONE',  ( 3.229232847726260403, -16.57333684275945629, 9.178419661560148768 ) ) ;
#29896 = EDGE_CURVE ( 'NONE', #11397, #31874, #35681, .T. ) ;
#29897 = LINE ( 'NONE', #42194, #28692 ) ;
#29898 = CARTESIAN_POINT ( 'NONE',  ( 15.57957361750251302, 5.755602074545510760, 3.266473740018926541 ) ) ;
#29899 = EDGE_CURVE ( 'NONE', #5590, #46138, #44819, .T. ) ;
#29900 = VERTEX_POINT ( 'NONE', #12806 ) ;
#29901 = ADVANCED_FACE ( 'NONE', ( #17161 ), #13297, .T. ) ;
#29902 = CARTESIAN_POINT ( 'NONE',  ( 9.760995290733820440, -2.173239732351728293, 9.646707543097347681 ) ) ;
#29903 = AXIS2_PLACEMENT_3D ( 'NONE', #42451, #3717, #42958 ) ;
#29904 = FACE_OUTER_BOUND ( 'NONE', #9350, .T. ) ;
#29905 = VECTOR ( 'NONE', #3638, 1000.000000000000000 ) ;
#29906 = CARTESIAN_POINT ( 'NONE',  ( 0.3370904143228959926, -0.2449105217885284291, 10.00000000000000000 ) ) ;
#29907 = LINE ( 'NONE', #37628, #16658 ) ;
#29908 = DIRECTION ( 'NONE',  ( -2.958228394578793832E-31, 0.000000000000000000, -1.000000000000000000 ) ) ;
#29909 = ORIENTED_EDGE ( 'NONE', *, *, #12028, .F. ) ;
#29910 = ORIENTED_EDGE ( 'NONE', *, *, #43970, .F. ) ;
#29911 = DIRECTION ( 'NONE',  ( 0.000000000000000000, 0.000000000000000000, -1.000000000000000000 ) ) ;
#29912 = COLOUR_RGB ( '',0.7921568627450980005, 0.8196078431372548767, 0.9333333333333333481 ) ;
#29913 = ORIENTED_EDGE ( 'NONE', *, *, #19025, .T. ) ;
#29914 = DIRECTION ( 'NONE',  ( -1.000000000000000000, -0.000000000000000000, -0.000000000000000000 ) ) ;
#29915 = CARTESIAN_POINT ( 'NONE',  ( 195.0540265531851105, 1.025126265847089657, -37.43171244307202272 ) ) ;
#29916 = VECTOR ( 'NONE', #43548, 1000.000000000000000 ) ;
#29917 = ORIENTED_EDGE ( 'NONE', *, *, #44186, .F. ) ;
#29918 = ORIENTED_EDGE ( 'NONE', *, *, #42103, .T. ) ;
#29919 = ORIENTED_EDGE ( 'NONE', *, *, #8703, .T. ) ;
#29920 =( BOUNDED_CURVE ( )  B_SPLINE_CURVE ( 3, ( #14514, #34033, #13562, #25377 ),
 .UNSPECIFIED., .F., .F. ) 
 B_SPLINE_CURVE_WITH_KNOTS ( ( 4, 4 ),
 ( 4.712388980384689674, 6.283185307179586232 ),
 .UNSPECIFIED. ) 
 CURVE ( )  GEOMETRIC_REPRESENTATION_ITEM ( )  RATIONAL_B_SPLINE_CURVE ( ( 1.000000000000000000, 0.8047378541243649375, 0.8047378541243649375, 1.000000000000000000 ) ) 
 REPRESENTATION_ITEM ( '' )  );
#29921 = AXIS2_PLACEMENT_3D ( 'NONE', #34696, #19784, #7229 ) ;
#29922 = EDGE_CURVE ( 'NONE', #44427, #34969, #40128, .T. ) ;
#29923 = ADVANCED_FACE ( 'NONE', ( #13048 ), #12296, .F. ) ;
#29924 = VECTOR ( 'NONE', #29821, 1000.000000000000000 ) ;
#29925 = DIRECTION ( 'NONE',  ( -0.000000000000000000, -1.000000000000000000, -0.000000000000000000 ) ) ;
#29926 = CARTESIAN_POINT ( 'NONE',  ( 16.99749102614301677, -1.320765928724307425, 8.953103998512858652 ) ) ;
#29927 = DIRECTION ( 'NONE',  ( 0.000000000000000000, 2.969158215481698263E-48, -1.000000000000000000 ) ) ;
#29928 = EDGE_CURVE ( 'NONE', #36961, #31206, #31467, .T. ) ;
#29929 = ORIENTED_EDGE ( 'NONE', *, *, #22103, .F. ) ;
#29930 = EDGE_CURVE ( 'NONE', #22771, #42166, #5091, .T. ) ;
#29931 = CARTESIAN_POINT ( 'NONE',  ( 1.249999999999999778, 0.000000000000000000, 10.00000000000000000 ) ) ;
#29932 = DIRECTION ( 'NONE',  ( 1.000000000000000000, 0.000000000000000000, 0.000000000000000000 ) ) ;
#29933 = DIRECTION ( 'NONE',  ( -0.000000000000000000, 0.8962124318248270161, 0.4436251537532894806 ) ) ;
#29934 = ORIENTED_EDGE ( 'NONE', *, *, #22751, .F. ) ;
#29935 = VERTEX_POINT ( 'NONE', #4359 ) ;
#29936 = CARTESIAN_POINT ( 'NONE',  ( 0.000000000000000000, 169.0000000000000000, -342.0000000000001705 ) ) ;
#29937 = EDGE_CURVE ( 'NONE', #13146, #7036, #25736, .T. ) ;
#29938 = CARTESIAN_POINT ( 'NONE',  ( -30.87089393895367095, 12.69923079256638587, -9.367992836599954742 ) ) ;
#29939 = EDGE_CURVE ( 'NONE', #23932, #7036, #22129, .T. ) ;
#29940 = PLANE ( 'NONE',  #14388 ) ;
#29941 = ORIENTED_EDGE ( 'NONE', *, *, #24742, .F. ) ;
#29942 = LINE ( 'NONE', #48882, #50308 ) ;
#29943 = CARTESIAN_POINT ( 'NONE',  ( 10.50000000000000178, -46.51315789473684248, 5.916985404131814619 ) ) ;
#29944 = AXIS2_PLACEMENT_3D ( 'NONE', #16725, #39091, #8033 ) ;
#29945 = CARTESIAN_POINT ( 'NONE',  ( -4.945973446814916130, 1.025126265847097651, 122.5682875569280128 ) ) ;
#29946 = CARTESIAN_POINT ( 'NONE',  ( 0.000000000000000000, 0.000000000000000000, 900.0000000000000000 ) ) ;
#29947 = PLANE ( 'NONE',  #34769 ) ;
#29948 = AXIS2_PLACEMENT_3D ( 'NONE', #13784, #2745, #34316 ) ;
#29949 = ORIENTED_EDGE ( 'NONE', *, *, #28393, .F. ) ;
#29950 = CARTESIAN_POINT ( 'NONE',  ( -1.011271242968677875, -0.7347315653656004697, 3.333333333333333481 ) ) ;
#29951 = CARTESIAN_POINT ( 'NONE',  ( 35.00000000000091660, 17.00000000000000000, -24.99999999999999289 ) ) ;
#29953 = CIRCLE ( 'NONE', #49562, 2.000000000000001776 ) ;
#29952 = DIRECTION ( 'NONE',  ( -1.000000000000000000, 0.000000000000000000, -0.000000000000000000 ) ) ;
#29954 = CARTESIAN_POINT ( 'NONE',  ( -204.9459734468149463, 2.143131898507890731E-16, 165.0000000000000000 ) ) ;
#29955 = EDGE_CURVE ( 'NONE', #48177, #14442, #24371, .T. ) ;
#29956 = LINE ( 'NONE', #25103, #41076 ) ;
#29957=STYLED_ITEM('',(#50782),#22574);
#29958 = EDGE_CURVE ( 'NONE', #40407, #40831, #39769, .T. ) ;
#29959 = ADVANCED_FACE ( 'NONE', ( #12545 ), #4841, .F. ) ;
#29961 = VECTOR ( 'NONE', #29242, 1000.000000000000000 ) ;
#29960 = FACE_OUTER_BOUND ( 'NONE', #35076, .T. ) ;
#29962 = VERTEX_POINT ( 'NONE', #3043 ) ;
#29963 = FACE_OUTER_BOUND ( 'NONE', #10996, .T. ) ;
#29964 = CARTESIAN_POINT ( 'NONE',  ( -36.97942854200451990, 6.226705766838657397, 8.914903342594564961 ) ) ;
#29965 = VECTOR ( 'NONE', #29631, 1000.000000000000114 ) ;
#29966 = CARTESIAN_POINT ( 'NONE',  ( 0.2776613828612440882, -1.251395203515894172, 9.967237415621763574 ) ) ;
#29967 = EDGE_CURVE ( 'NONE', #21965, #34539, #1169, .T. ) ;
#29968 = ORIENTED_EDGE ( 'NONE', *, *, #31934, .F. ) ;
#29969 = LINE ( 'NONE', #38435, #15828 ) ;
#29970 = DIRECTION ( 'NONE',  ( -0.000000000000000000, -0.000000000000000000, 1.000000000000000000 ) ) ;
#29971 = VERTEX_POINT ( 'NONE', #14856 ) ;
#29972 = CARTESIAN_POINT ( 'NONE',  ( 168.9999999999999716, -184.9999999999999716, -356.0000000000001705 ) ) ;
#29973 = FACE_OUTER_BOUND ( 'NONE', #11203, .T. ) ;
#29974 = LINE ( 'NONE', #46078, #22368 ) ;
#29975 = DIRECTION ( 'NONE',  ( -0.000000000000000000, -0.000000000000000000, -1.000000000000000000 ) ) ;
#29976 = EDGE_LOOP ( 'NONE', ( #32718, #30577, #763, #38641, #47556 ) ) ;
#29977 = DIRECTION ( 'NONE',  ( -6.938893903907227392E-16, 1.000000000000000000, 0.000000000000000000 ) ) ;
#29978 = ORIENTED_EDGE ( 'NONE', *, *, #4497, .F. ) ;
#29979 = ORIENTED_EDGE ( 'NONE', *, *, #18583, .T. ) ;
#29980 = CARTESIAN_POINT ( 'NONE',  ( -4.945973446814903696, 2.143131898507912917E-16, -120.9317124430720725 ) ) ;
#29981 = AXIS2_PLACEMENT_3D ( 'NONE', #26575, #22719, #11946 ) ;
#29982 = ORIENTED_EDGE ( 'NONE', *, *, #19095, .F. ) ;
#29983 = LINE ( 'NONE', #45091, #39365 ) ;
#29984 = CARTESIAN_POINT ( 'NONE',  ( -0.3862712429686809279, -1.188820645368943163, 10.00000000000000000 ) ) ;
#29985 = EDGE_CURVE ( 'NONE', #19548, #30870, #13864, .T. ) ;
#29986 = VECTOR ( 'NONE', #708, 1000.000000000000000 ) ;
#29987 = CARTESIAN_POINT ( 'NONE',  ( 29.61572577327002520, 16.11461842845735859, 8.807470649214879543 ) ) ;
#29988 = LINE ( 'NONE', #6885, #2654 ) ;
#29989 = VECTOR ( 'NONE', #29385, 1000.000000000000000 ) ;
#29990 = CARTESIAN_POINT ( 'NONE',  ( 0.3910393408562611861, 3.877122853646846945, 9.741991644046958498 ) ) ;
#29991 = VERTEX_POINT ( 'NONE', #41049 ) ;
#29992 = CARTESIAN_POINT ( 'NONE',  ( 34.95136153415558056, -36.40974830873469870, 8.356839323120299312 ) ) ;
#29993 = CARTESIAN_POINT ( 'NONE',  ( -88.44597344681497475, 0.000000000000000000, 82.56828755692801280 ) ) ;
#29994 = DIRECTION ( 'NONE',  ( 0.000000000000000000, -1.000000000000000000, 0.000000000000000000 ) ) ;
#29995=STYLED_ITEM('',(#50747),#22914);
#29996 = EDGE_CURVE ( 'NONE', #41657, #38451, #30258, .T. ) ;
#29997 = ORIENTED_EDGE ( 'NONE', *, *, #29412, .F. ) ;
#29998 = ADVANCED_FACE ( 'NONE', ( #37229 ), #14086, .F. ) ;
#29999 = CYLINDRICAL_SURFACE ( 'NONE', #48861, 1.750000000000008438 ) ;
#30000 = CARTESIAN_POINT ( 'NONE',  ( -204.9459734468149463, 2.143131898507880377E-16, 39.06828755692798438 ) ) ;
#30001 = ORIENTED_EDGE ( 'NONE', *, *, #8751, .T. ) ;
#30002 = CIRCLE ( 'NONE', #7887, 37.50000000000000000 ) ;
#30003 = ORIENTED_EDGE ( 'NONE', *, *, #40965, .T. ) ;
#30004 = ORIENTED_EDGE ( 'NONE', *, *, #6024, .T. ) ;
#30005 = CARTESIAN_POINT ( 'NONE',  ( 80.00000000000028422, 17.00000000000000000, -84.99999999999998579 ) ) ;
#30006 = EDGE_CURVE ( 'NONE', #13383, #43783, #36238, .T. ) ;
#30007 = PLANE ( 'NONE',  #25056 ) ;
#30008 = EDGE_LOOP ( 'NONE', ( #12506, #16086, #18210, #16101, #34272, #24720 ) ) ;
#30009 = VECTOR ( 'NONE', #18844, 1000.000000000000000 ) ;
#30010 = ADVANCED_FACE ( 'NONE', ( #49953 ), #42048, .F. ) ;
#30011 = LINE ( 'NONE', #41792, #49958 ) ;
#30012 = ADVANCED_FACE ( 'NONE', ( #48939 ), #22045, .F. ) ;
#30013 = FACE_BOUND ( 'NONE', #37907, .T. ) ;
#30014 = CARTESIAN_POINT ( 'NONE',  ( -164.9999999999984936, 17.00000000000000000, 35.00000000000000000 ) ) ;
#30015 = EDGE_LOOP ( 'NONE', ( #38003, #6914, #41156, #48374 ) ) ;
#30016 =( BOUNDED_CURVE ( )  B_SPLINE_CURVE ( 3, ( #30772, #14858, #6910, #39236 ),
 .UNSPECIFIED., .F., .F. ) 
 B_SPLINE_CURVE_WITH_KNOTS ( ( 4, 4 ),
 ( 1.570796326794896558, 3.141592653589793116 ),
 .UNSPECIFIED. ) 
 CURVE ( )  GEOMETRIC_REPRESENTATION_ITEM ( )  RATIONAL_B_SPLINE_CURVE ( ( 1.000000000000000000, 0.8047378541243649375, 0.8047378541243649375, 1.000000000000000000 ) ) 
 REPRESENTATION_ITEM ( '' )  );
#30017 = CARTESIAN_POINT ( 'NONE',  ( 6.429410166934437676, 2.386389549874229132, 9.753789706659947711 ) ) ;
#30018 =( NAMED_UNIT ( * ) PLANE_ANGLE_UNIT ( ) SI_UNIT ( $, .RADIAN. ) );
#30019 = ADVANCED_FACE ( 'NONE', ( #13825 ), #2545, .F. ) ;
#30020 = CARTESIAN_POINT ( 'NONE',  ( -8.831420117243776957, -14.12636088103186260, -3.546734833711462365 ) ) ;
#30021 = ORIENTED_EDGE ( 'NONE', *, *, #3633, .T. ) ;
#30022 = CONTEXT_DEPENDENT_SHAPE_REPRESENTATION ( #18765, #7754 ) ;
#30023 = CARTESIAN_POINT ( 'NONE',  ( 113.3040265531850537, 1.749999999999997335, -119.1817124430720440 ) ) ;
#30024 = CARTESIAN_POINT ( 'NONE',  ( 28.55116071645549525, -41.05976639056858346, -2.408242355805840784 ) ) ;
#30025 = AXIS2_PLACEMENT_3D ( 'NONE', #41148, #33722, #41659 ) ;
#30026 = AXIS2_PLACEMENT_3D ( 'NONE', #20333, #4182, #345 ) ;
#30027 = ADVANCED_FACE ( 'NONE', ( #2050 ), #17696, .T. ) ;
#30029 = CIRCLE ( 'NONE', #41478, 3.500000000000003109 ) ;
#30028 = CARTESIAN_POINT ( 'NONE',  ( 342.0000000000000000, -2.999999999999919176, 171.9999999999998295 ) ) ;
#30030 = CARTESIAN_POINT ( 'NONE',  ( -2.391286777839504385, 5.398370916126228103, 9.586754400233969520 ) ) ;
#30031 = EDGE_LOOP ( 'NONE', ( #29616, #24385, #17304, #9115 ) ) ;
#30032 = CARTESIAN_POINT ( 'NONE',  ( 195.0540265531851105, 2.143131898507880377E-16, 165.0000000000000000 ) ) ;
#30033 = CARTESIAN_POINT ( 'NONE',  ( 24.39427009665985224, 44.07992421011656603, 8.807470649214879543 ) ) ;
#30034 = DIRECTION ( 'NONE',  ( 0.000000000000000000, 0.000000000000000000, -1.000000000000000000 ) ) ;
#30035 = LINE ( 'NONE', #45640, #20058 ) ;
#30036 = CARTESIAN_POINT ( 'NONE',  ( 113.3040265531850537, 1.749999999999997335, 80.81828755692798438 ) ) ;
#30037 = VECTOR ( 'NONE', #38781, 1000.000000000000000 ) ;
#30038 = ORIENTED_EDGE ( 'NONE', *, *, #2276, .T. ) ;
#30039 = DIRECTION ( 'NONE',  ( -1.000000000000000000, 0.000000000000000000, 0.000000000000000000 ) ) ;
#30040 = ORIENTED_EDGE ( 'NONE', *, *, #42017, .F. ) ;
#30041 = CARTESIAN_POINT ( 'NONE',  ( 74.32915281903215998, -1.750000000000009548, -40.20683870891912193 ) ) ;
#30042 = VERTEX_POINT ( 'NONE', #29499 ) ;
#30043 = DIRECTION ( 'NONE',  ( -0.000000000000000000, -1.000000000000000000, -0.000000000000000000 ) ) ;
#30044 = DIRECTION ( 'NONE',  ( -1.000000000000000000, 0.000000000000000000, -0.000000000000000000 ) ) ;
#30045 = VERTEX_POINT ( 'NONE', #21802 ) ;
#30046 = SURFACE_STYLE_USAGE ( .BOTH. , #37505 ) ;
#30047 = ORIENTED_EDGE ( 'NONE', *, *, #17205, .F. ) ;
#30048 = VECTOR ( 'NONE', #43111, 1000.000000000000000 ) ;
#30049 = CARTESIAN_POINT ( 'NONE',  ( 34.32915281903212446, -1.750000000000009548, 39.79316129108089228 ) ) ;
#30050 = ORIENTED_EDGE ( 'NONE', *, *, #48527, .T. ) ;
#30051 = DIRECTION ( 'NONE',  ( -1.000000000000000000, -0.000000000000000000, -0.000000000000000000 ) ) ;
#30052 = PLANE ( 'NONE',  #29813 ) ;
#30053 = CARTESIAN_POINT ( 'NONE',  ( 0.000000000000000000, 184.8000000000000114, 359.7999999999997840 ) ) ;
#30054 = CARTESIAN_POINT ( 'NONE',  ( 193.3040265531851105, 1.750000000000010214, -39.18171244307202983 ) ) ;
#30055 = CARTESIAN_POINT ( 'NONE',  ( -1.873480598308069123, 3.275918692700744206, 9.865049507598756762 ) ) ;
#30056 = VERTEX_POINT ( 'NONE', #37474 ) ;
#30057 = VERTEX_POINT ( 'NONE', #10746 ) ;
#30058 = LINE ( 'NONE', #30302, #43945 ) ;
#30059 = EDGE_CURVE ( 'NONE', #24640, #26096, #48898, .T. ) ;
#30060 = ORIENTED_EDGE ( 'NONE', *, *, #6986, .F. ) ;
#30061 = EDGE_CURVE ( 'NONE', #45355, #39370, #47275, .T. ) ;
#30062 = AXIS2_PLACEMENT_3D ( 'NONE', #2474, #49628, #45791 ) ;
#30063 = CARTESIAN_POINT ( 'NONE',  ( 194.9999999999999432, 173.0000000000000000, 231.9999999999999716 ) ) ;
#30064 = FACE_OUTER_BOUND ( 'NONE', #16477, .T. ) ;
#30065 = ORIENTED_EDGE ( 'NONE', *, *, #7420, .T. ) ;
#30066 = CARTESIAN_POINT ( 'NONE',  ( 214.9999999999999432, -175.0000000000000000, 500.0000000000000000 ) ) ;
#30067 = ADVANCED_FACE ( 'NONE', ( #26148 ), #15371, .T. ) ;
#30068 = CARTESIAN_POINT ( 'NONE',  ( 80.00000000000216005, 16.00000000000000000, 95.00000000000000000 ) ) ;
#30069 = ORIENTED_EDGE ( 'NONE', *, *, #42974, .F. ) ;
#30070 = DIRECTION ( 'NONE',  ( -1.000000000000000000, 0.000000000000000000, 0.000000000000000000 ) ) ;
#30071 = EDGE_CURVE ( 'NONE', #8815, #14722, #2793, .T. ) ;
#30072 = CARTESIAN_POINT ( 'NONE',  ( -48.44597344681495343, 0.000000000000000000, -117.4317124430720156 ) ) ;
#30073 = EDGE_CURVE ( 'NONE', #13712, #24906, #48602, .T. ) ;
#30074 =( BOUNDED_CURVE ( )  B_SPLINE_CURVE ( 3, ( #1678, #13212, #5266, #44494 ),
 .UNSPECIFIED., .F., .F. ) 
 B_SPLINE_CURVE_WITH_KNOTS ( ( 4, 4 ),
 ( 3.141592653589793116, 4.712388980384689674 ),
 .UNSPECIFIED. ) 
 CURVE ( )  GEOMETRIC_REPRESENTATION_ITEM ( )  RATIONAL_B_SPLINE_CURVE ( ( 1.000000000000000000, 0.8047378541243649375, 0.8047378541243649375, 1.000000000000000000 ) ) 
 REPRESENTATION_ITEM ( '' )  );
#30075 = DIRECTION ( 'NONE',  ( -1.000000000000000000, -0.000000000000000000, -0.000000000000000000 ) ) ;
#30076 = ORIENTED_EDGE ( 'NONE', *, *, #41215, .F. ) ;
#30077 = ORIENTED_EDGE ( 'NONE', *, *, #27562, .F. ) ;
#30078 =( BOUNDED_CURVE ( )  B_SPLINE_CURVE ( 3, ( #24542, #20687, #17090, #45012 ),
 .UNSPECIFIED., .F., .F. ) 
 B_SPLINE_CURVE_WITH_KNOTS ( ( 4, 4 ),
 ( 0.000000000000000000, 1.570796326794896558 ),
 .UNSPECIFIED. ) 
 CURVE ( )  GEOMETRIC_REPRESENTATION_ITEM ( )  RATIONAL_B_SPLINE_CURVE ( ( 1.000000000000000000, 0.8047378541243649375, 0.8047378541243649375, 1.000000000000000000 ) ) 
 REPRESENTATION_ITEM ( '' )  );
#30079 = ADVANCED_FACE ( 'NONE', ( #16130 ), #7162, .T. ) ;
#30080 = CARTESIAN_POINT ( 'NONE',  ( 26.18032376592674737, -21.95228666728361233, 7.455576670931136185 ) ) ;
#30081 = ORIENTED_EDGE ( 'NONE', *, *, #38139, .F. ) ;
#30082 = VECTOR ( 'NONE', #30627, 1000.000000000000000 ) ;
#30083 = ORIENTED_EDGE ( 'NONE', *, *, #94, .F. ) ;
#30084 = DIRECTION ( 'NONE',  ( 0.000000000000000000, 0.000000000000000000, 1.000000000000000000 ) ) ;
#30085 = CARTESIAN_POINT ( 'NONE',  ( 6.219530239386670267, -7.848697864701615678, 6.429802539306459508 ) ) ;
#30086 = FACE_OUTER_BOUND ( 'NONE', #7070, .T. ) ;
#30087 = DIRECTION ( 'NONE',  ( 0.4055129968046615185, 0.4055129968046615185, -0.8192181753629524943 ) ) ;
#30088 = LINE ( 'NONE', #33441, #37349 ) ;
#30089 = CARTESIAN_POINT ( 'NONE',  ( 359.9999999999999432, -169.0000000000001705, 344.0000000000000000 ) ) ;
#30090 = LINE ( 'NONE', #38308, #11692 ) ;
#30091 = ORIENTED_EDGE ( 'NONE', *, *, #32564, .F. ) ;
#30092 = LINE ( 'NONE', #41122, #19818 ) ;
#30093 = LINE ( 'NONE', #14432, #3142 ) ;
#30094 = CARTESIAN_POINT ( 'NONE',  ( 0.000000000000000000, 0.000000000000000000, 910.0000000000000000 ) ) ;
#30095 = DIRECTION ( 'NONE',  ( -1.132880637372608740E-16, -4.718402560806925739E-50, -1.000000000000000000 ) ) ;
#30097 = VERTEX_POINT ( 'NONE', #26661 ) ;
#30096 = CIRCLE ( 'NONE', #11297, 4.000000000000003553 ) ;
#30098 = DIRECTION ( 'NONE',  ( 0.000000000000000000, 0.000000000000000000, -1.000000000000000000 ) ) ;
#30099 = ORIENTED_EDGE ( 'NONE', *, *, #43706, .F. ) ;
#30100 = LINE ( 'NONE', #37812, #42629 ) ;
#30101 = CARTESIAN_POINT ( 'NONE',  ( 1.326845121651809789, -0.3624933883365012988, 9.972175347158398040 ) ) ;
#30102 = DIRECTION ( 'NONE',  ( 0.000000000000000000, 1.000000000000000000, 0.000000000000000000 ) ) ;
#30103 = ORIENTED_EDGE ( 'NONE', *, *, #45622, .T. ) ;
#30104 = EDGE_CURVE ( 'NONE', #16089, #42464, #31291, .T. ) ;
#30105 = ORIENTED_EDGE ( 'NONE', *, *, #36352, .F. ) ;
#30106 = DIRECTION ( 'NONE',  ( -1.000000000000000000, 0.000000000000000000, -1.612977847700450206E-50 ) ) ;
#30107 = CARTESIAN_POINT ( 'NONE',  ( -5.670847180967843570, 1.750000000000022427, 161.8434138227750907 ) ) ;
#30108 = ORIENTED_EDGE ( 'NONE', *, *, #39974, .F. ) ;
#30109 = EDGE_LOOP ( 'NONE', ( #46274, #31359, #2170, #40119, #11961, #45879 ) ) ;
#30110 = DIRECTION ( 'NONE',  ( 1.000000000000000000, 0.000000000000000000, -0.000000000000000000 ) ) ;
#30111 = FACE_OUTER_BOUND ( 'NONE', #31194, .T. ) ;
#30112 = EDGE_LOOP ( 'NONE', ( #46998, #25788, #42136, #15497 ) ) ;
#30113 = VERTEX_POINT ( 'NONE', #39490 ) ;
#30114 = DIRECTION ( 'NONE',  ( -1.000000000000000000, 0.000000000000000000, 0.000000000000000000 ) ) ;
#30115 = LINE ( 'NONE', #42400, #45544 ) ;
#30116 = CARTESIAN_POINT ( 'NONE',  ( 31.55402655318503236, 0.000000000000000000, 159.0682875569279702 ) ) ;
#30117 = EDGE_LOOP ( 'NONE', ( #28874, #2764, #24946, #5300, #6601, #33637, #39596, #36313 ) ) ;
#30118 = PLANE ( 'NONE',  #15327 ) ;
#30119 = ORIENTED_EDGE ( 'NONE', *, *, #2080, .T. ) ;
#30120 = LINE ( 'NONE', #38850, #22575 ) ;
#30121 = FACE_OUTER_BOUND ( 'NONE', #23184, .T. ) ;
#30122 = ORIENTED_EDGE ( 'NONE', *, *, #37837, .F. ) ;
#30123 = AXIS2_PLACEMENT_3D ( 'NONE', #46560, #35088, #15561 ) ;
#30124 = EDGE_LOOP ( 'NONE', ( #20018, #35060, #49750, #46740 ) ) ;
#30125 = ORIENTED_EDGE ( 'NONE', *, *, #38669, .T. ) ;
#30126 = ADVANCED_FACE ( 'NONE', ( #15110 ), #16674, .T. ) ;
#30127 = FACE_OUTER_BOUND ( 'NONE', #17435, .T. ) ;
#30128 = DIRECTION ( 'NONE',  ( -0.000000000000000000, -1.000000000000000000, -0.000000000000000000 ) ) ;
#30129 = ORIENTED_EDGE ( 'NONE', *, *, #23028, .T. ) ;
#30130 = DIRECTION ( 'NONE',  ( -1.000000000000000000, -0.000000000000000000, -0.000000000000000000 ) ) ;
#30131 = EDGE_LOOP ( 'NONE', ( #37402, #10164, #26277, #33781 ) ) ;
#30132 = CARTESIAN_POINT ( 'NONE',  ( -2.769930902779030646, 9.621092503091231762, 6.185716040203081079 ) ) ;
#30133 = DIRECTION ( 'NONE',  ( -1.000000000000000000, 0.000000000000000000, -0.000000000000000000 ) ) ;
#30134 = ORIENTED_EDGE ( 'NONE', *, *, #7173, .F. ) ;
#30135 = CARTESIAN_POINT ( 'NONE',  ( 350.0000000000000000, -164.9999999999999432, 343.9999999999997726 ) ) ;
#30136 = B_SPLINE_CURVE_WITH_KNOTS ( 'NONE', 3,
 ( #30422, #19626, #11425, #27331 ),
 .UNSPECIFIED., .F., .F.,
 ( 4, 4 ),
 ( 0.8097120833243712790, 0.9322955464062560038 ),
 .UNSPECIFIED. ) ;
#30137 = CARTESIAN_POINT ( 'NONE',  ( 183.0000000000000284, -174.9999999999999716, -111.0000000000001563 ) ) ;
#30138 = FACE_OUTER_BOUND ( 'NONE', #16151, .T. ) ;
#30139 = CARTESIAN_POINT ( 'NONE',  ( -86.69597344681494633, 1.750000000000010214, -39.18171244307202983 ) ) ;
#30140 = CARTESIAN_POINT ( 'NONE',  ( -165.6708471809677974, -1.750000000000010436, -120.2068387089191219 ) ) ;
#30141 = ORIENTED_EDGE ( 'NONE', *, *, #3999, .T. ) ;
#30142 = CARTESIAN_POINT ( 'NONE',  ( 135.0000000000015632, 16.00000000000000000, 35.00000000000000000 ) ) ;
#30143 = CIRCLE ( 'NONE', #25232, 4.000000000000003553 ) ;
#30144 = DIRECTION ( 'NONE',  ( 0.000000000000000000, 0.000000000000000000, 1.000000000000000000 ) ) ;
#30145 = DIRECTION ( 'NONE',  ( 1.000000000000000000, 0.000000000000000000, 0.000000000000000000 ) ) ;
#30146 = DIRECTION ( 'NONE',  ( -1.000000000000000000, 0.000000000000000000, 0.000000000000000000 ) ) ;
#30147 = FACE_OUTER_BOUND ( 'NONE', #13402, .T. ) ;
#30148 = CARTESIAN_POINT ( 'NONE',  ( 135.0000000000009663, 17.00000000000000000, -24.99999999999999289 ) ) ;
#30149 = DIRECTION ( 'NONE',  ( 0.000000000000000000, -0.000000000000000000, 1.000000000000000000 ) ) ;
#30150 = DIRECTION ( 'NONE',  ( 0.000000000000000000, 0.000000000000000000, -1.000000000000000000 ) ) ;
#30151 = ADVANCED_FACE ( 'NONE', ( #27674 ), #23830, .T. ) ;
#30152 = VERTEX_POINT ( 'NONE', #8180 ) ;
#30153 = CARTESIAN_POINT ( 'NONE',  ( 32.57680531928920686, 38.13496438397469035, -8.466730184410787174 ) ) ;
#30154 = VECTOR ( 'NONE', #36675, 1000.000000000000000 ) ;
#30155 = CARTESIAN_POINT ( 'NONE',  ( 85.00000000000184741, 17.00000000000000000, 65.00000000000000000 ) ) ;
#30156 = CARTESIAN_POINT ( 'NONE',  ( 0.1475726264153646716, 1.496347932843221429, 9.927319414211224213 ) ) ;
#30157 = CARTESIAN_POINT ( 'NONE',  ( 168.9999999999999716, -93.49999999999998579, -350.0000000000001705 ) ) ;
#30158 = FACE_BOUND ( 'NONE', #12174, .T. ) ;
#30159 = ORIENTED_EDGE ( 'NONE', *, *, #21901, .T. ) ;
#30160 = ORIENTED_EDGE ( 'NONE', *, *, #1547, .F. ) ;
#30161 = CARTESIAN_POINT ( 'NONE',  ( -4.999999999999997335, 214.9999999999999716, -234.7500000000000000 ) ) ;
#30162 = DIRECTION ( 'NONE',  ( 0.000000000000000000, -1.000000000000000000, -1.544785076050074834E-48 ) ) ;
#30163 = ORIENTED_EDGE ( 'NONE', *, *, #29405, .T. ) ;
#30164 = CARTESIAN_POINT ( 'NONE',  ( -12.97493236725075683, 11.05939663307000664, 8.953103998512858652 ) ) ;
#30165 = CARTESIAN_POINT ( 'NONE',  ( 85.00000000000090949, 16.00000000000000000, -24.99999999999999289 ) ) ;
#30166 = CARTESIAN_POINT ( 'NONE',  ( -15.00199999999999712, -34.54492135858216528, 0.000000000000000000 ) ) ;
#30167 = ORIENTED_EDGE ( 'NONE', *, *, #4527, .F. ) ;
#30168 = ORIENTED_EDGE ( 'NONE', *, *, #10588, .F. ) ;
#30169 = ORIENTED_EDGE ( 'NONE', *, *, #34567, .F. ) ;
#30170 = DIRECTION ( 'NONE',  ( -1.000000000000000000, 0.000000000000000000, 0.000000000000000000 ) ) ;
#30171 = CARTESIAN_POINT ( 'NONE',  ( 113.3040265531850537, -1.749999999999997113, -39.18171244307202983 ) ) ;
#30172 = CARTESIAN_POINT ( 'NONE',  ( -16.07893968642797233, -33.88550589494182930, 8.100132398494514163 ) ) ;
#30173 = ORIENTED_EDGE ( 'NONE', *, *, #48394, .T. ) ;
#30174 = DIRECTION ( 'NONE',  ( 0.000000000000000000, 0.000000000000000000, 1.000000000000000000 ) ) ;
#30175 = DIRECTION ( 'NONE',  ( 0.000000000000000000, 0.000000000000000000, 1.000000000000000000 ) ) ;
#30176 = LINE ( 'NONE', #41981, #49871 ) ;
#30177 = VERTEX_POINT ( 'NONE', #26907 ) ;
#30178 = ORIENTED_EDGE ( 'NONE', *, *, #17782, .T. ) ;
#30179 = CARTESIAN_POINT ( 'NONE',  ( 75.05402655318509630, 2.143131898507880377E-16, 165.0000000000000000 ) ) ;
#30180 = EDGE_CURVE ( 'NONE', #21718, #34526, #30828, .T. ) ;
#30181 = CARTESIAN_POINT ( 'NONE',  ( 1.224655226406667019, 1.100228625579998010, 9.936700280135880803 ) ) ;
#30182 = CARTESIAN_POINT ( 'NONE',  ( 71.55402655318505367, 0.000000000000000000, 79.06828755692797017 ) ) ;
#30183 = ORIENTED_EDGE ( 'NONE', *, *, #32402, .F. ) ;
#30184 = DIRECTION ( 'NONE',  ( 0.000000000000000000, -2.537652627714643577E-15, -1.000000000000000000 ) ) ;
#30185 = FACE_OUTER_BOUND ( 'NONE', #44976, .T. ) ;
#30186 = DIRECTION ( 'NONE',  ( 0.000000000000000000, 0.000000000000000000, 1.000000000000000000 ) ) ;
#30187 = DIRECTION ( 'NONE',  ( -0.000000000000000000, -0.000000000000000000, -1.000000000000000000 ) ) ;
#30188 = AXIS2_PLACEMENT_3D ( 'NONE', #25045, #28130, #4523 ) ;
#30189 = DIRECTION ( 'NONE',  ( 0.000000000000000000, 0.000000000000000000, -1.000000000000000000 ) ) ;
#30190 = VERTEX_POINT ( 'NONE', #42545 ) ;
#30191 = CYLINDRICAL_SURFACE ( 'NONE', #47204, 4.000000000000003553 ) ;
#30192 = EDGE_CURVE ( 'NONE', #6937, #11052, #11519, .T. ) ;
#30193 = CARTESIAN_POINT ( 'NONE',  ( -69.99999999999972999, 17.00000000000000000, -84.99999999999998579 ) ) ;
#30194 = LINE ( 'NONE', #42496, #50190 ) ;
#30195 = ADVANCED_FACE ( 'NONE', ( #38981 ), #3814, .T. ) ;
#30196 = CARTESIAN_POINT ( 'NONE',  ( -34.94239438780405749, -13.71128139791396272, 3.209567239418968487 ) ) ;
#30197 = CLOSED_SHELL ( 'NONE', ( #20860, #19897, #4556, #14867, #50100, #917, #2749, #49607, #17385, #33103, #21764, #36085, #23955, #44661, #13928, #12733, #10558, #50676 ) ) ;
#30198 = ADVANCED_FACE ( 'NONE', ( #46873 ), #43056, .F. ) ;
#30199 = CARTESIAN_POINT ( 'NONE',  ( 48.98697415750968531, 11.03699497439252575, -8.016098858316205167 ) ) ;
#30200 = DIRECTION ( 'NONE',  ( 1.000000000000000000, -4.758098676964957447E-16, -1.586032892321651989E-16 ) ) ;
#30201 = EDGE_LOOP ( 'NONE', ( #49903, #43810, #37389, #4037 ) ) ;
#30202 = CARTESIAN_POINT ( 'NONE',  ( 33.16902712922644270, -37.70469005304286725, 1.847720168420772691 ) ) ;
#30203 = DIRECTION ( 'NONE',  ( -1.000000000000000000, -0.000000000000000000, -0.000000000000000000 ) ) ;
#30204 = EDGE_CURVE ( 'NONE', #14675, #36229, #6995, .T. ) ;
#30205 = EDGE_CURVE ( 'NONE', #1237, #40207, #40751, .T. ) ;
#30206 = CARTESIAN_POINT ( 'NONE',  ( 115.0540265531850395, 2.143131898507847836E-16, -157.4317124430720582 ) ) ;
#30208 = ORIENTED_EDGE ( 'NONE', *, *, #38542, .T. ) ;
#30207 = EDGE_CURVE ( 'NONE', #15732, #40036, #31791, .T. ) ;
#30209 = ADVANCED_FACE ( 'NONE', ( #40491, #25094 ), #728, .T. ) ;
#30210 = CARTESIAN_POINT ( 'NONE',  ( 7.499999999999996447, 194.9999999999999716, -240.0000000000000000 ) ) ;
#30211 = ORIENTED_EDGE ( 'NONE', *, *, #35568, .F. ) ;
#30212 = DIRECTION ( 'NONE',  ( 1.000000000000000000, 0.000000000000000000, 0.000000000000000000 ) ) ;
#30213 = CARTESIAN_POINT ( 'NONE',  ( 151.5540265531850537, 0.000000000000000000, 159.0682875569279702 ) ) ;
#30214 = DIRECTION ( 'NONE',  ( 0.000000000000000000, -1.000000000000000000, 0.000000000000000000 ) ) ;
#30215 = CARTESIAN_POINT ( 'NONE',  ( -46.69597344681494633, 1.750000000000010658, 120.8182875569279702 ) ) ;
#30216 = EDGE_CURVE ( 'NONE', #21335, #16313, #6686, .T. ) ;
#30217 =( BOUNDED_CURVE ( )  B_SPLINE_CURVE ( 3, ( #14960, #49548, #30107, #41898 ),
 .UNSPECIFIED., .F., .F. ) 
 B_SPLINE_CURVE_WITH_KNOTS ( ( 4, 4 ),
 ( 3.141592653589793116, 4.712388980384689674 ),
 .UNSPECIFIED. ) 
 CURVE ( )  GEOMETRIC_REPRESENTATION_ITEM ( )  RATIONAL_B_SPLINE_CURVE ( ( 1.000000000000000000, 0.8047378541243649375, 0.8047378541243649375, 1.000000000000000000 ) ) 
 REPRESENTATION_ITEM ( '' )  );
#30218 = ORIENTED_EDGE ( 'NONE', *, *, #31588, .T. ) ;
#30219 = DIRECTION ( 'NONE',  ( -1.000000000000000000, -0.000000000000000000, -0.000000000000000000 ) ) ;
#30220 = ORIENTED_EDGE ( 'NONE', *, *, #45075, .T. ) ;
#30221 = ORIENTED_EDGE ( 'NONE', *, *, #15192, .F. ) ;
#30222 = CARTESIAN_POINT ( 'NONE',  ( -5.923309609702550382, 5.336940278790372361, -7.724940478959219092E-16 ) ) ;
#30223 = AXIS2_PLACEMENT_3D ( 'NONE', #2919, #18572, #34248 ) ;
#30224 = VECTOR ( 'NONE', #5078, 1000.000000000000000 ) ;
#30225 = ORIENTED_EDGE ( 'NONE', *, *, #45007, .T. ) ;
#30226 = CARTESIAN_POINT ( 'NONE',  ( -5.000000000000000000, 175.0000000000000284, 350.0000000000002274 ) ) ;
#30227 = CYLINDRICAL_SURFACE ( 'NONE', #27399, 1.750000000000010214 ) ;
#30228 = CARTESIAN_POINT ( 'NONE',  ( 181.0000000000000000, -5.999999999999950262, 339.9999999999998295 ) ) ;
#30229 = AXIS2_PLACEMENT_3D ( 'NONE', #44620, #32101, #12583 ) ;
#30230 = AXIS2_PLACEMENT_3D ( 'NONE', #36194, #32340, #40041 ) ;
#30231 = PLANE ( 'NONE',  #1026 ) ;
#30232 = LINE ( 'NONE', #33095, #50495 ) ;
#30233 = AXIS2_PLACEMENT_3D ( 'NONE', #15174, #31083, #19262 ) ;
#30234 = ADVANCED_FACE ( 'NONE', ( #12517 ), #40235, .F. ) ;
#30235 = ORIENTED_EDGE ( 'NONE', *, *, #10458, .F. ) ;
#30236 = FACE_OUTER_BOUND ( 'NONE', #28585, .T. ) ;
#30237 = CARTESIAN_POINT ( 'NONE',  ( 75.05402655318509630, 2.143131898507880377E-16, 159.0682875569279702 ) ) ;
#30238 = DIRECTION ( 'NONE',  ( -1.096345236817341200E-13, 0.000000000000000000, 1.000000000000000000 ) ) ;
#30239 = AXIS2_PLACEMENT_3D ( 'NONE', #33845, #13561, #34100 ) ;
#30240 = EDGE_CURVE ( 'NONE', #36302, #24372, #20774, .T. ) ;
#30241 = ORIENTED_EDGE ( 'NONE', *, *, #46124, .T. ) ;
#30242 = ADVANCED_FACE ( 'NONE', ( #1247 ), #5574, .F. ) ;
#30243 = LINE ( 'NONE', #34355, #25152 ) ;
#30244 = CARTESIAN_POINT ( 'NONE',  ( -69.99999999999783995, 17.00000000000000000, 95.00000000000000000 ) ) ;
#30245 = ORIENTED_EDGE ( 'NONE', *, *, #22812, .T. ) ;
#30246 = APPLICATION_CONTEXT ( 'automotive_design' ) ;
#30247 = ORIENTED_EDGE ( 'NONE', *, *, #30906, .F. ) ;
#30248 = VERTEX_POINT ( 'NONE', #8692 ) ;
#30249 = CARTESIAN_POINT ( 'NONE',  ( -164.9459734468149463, 2.143131898507880377E-16, -80.93171244307201562 ) ) ;
#30250 = EDGE_CURVE ( 'NONE', #10906, #21159, #36549, .T. ) ;
#30251 = CARTESIAN_POINT ( 'NONE',  ( 5.888214538810389698, 16.20866436362417673, 8.727788335465566760 ) ) ;
#30252 = PRODUCT_DEFINITION_SHAPE ( 'NONE', 'NONE',  #38783 ) ;
#30253 = ORIENTED_EDGE ( 'NONE', *, *, #45604, .F. ) ;
#30254 = EDGE_CURVE ( 'NONE', #17123, #29900, #11953, .T. ) ;
#30255 = CARTESIAN_POINT ( 'NONE',  ( 113.3040265531850537, 0.000000000000000000, 165.0000000000000000 ) ) ;
#30256 = CARTESIAN_POINT ( 'NONE',  ( 356.0000000000001137, 165.0000000000000000, 339.9999999999998295 ) ) ;
#30257 = CARTESIAN_POINT ( 'NONE',  ( 343.9999999999994316, 183.0000000000000284, -358.0000000000001705 ) ) ;
#30258 = LINE ( 'NONE', #17929, #46423 ) ;
#30259 = CARTESIAN_POINT ( 'NONE',  ( -9.174209336589896679, -3.979181203266159095, 9.646707543097347681 ) ) ;
#30260 = ORIENTED_EDGE ( 'NONE', *, *, #11716, .T. ) ;
#30261 = CARTESIAN_POINT ( 'NONE',  ( -0.7606162131530730397, 1.296876929034918691, 9.953784399990622589 ) ) ;
#30262 = DIRECTION ( 'NONE',  ( 0.000000000000000000, 0.000000000000000000, 1.000000000000000000 ) ) ;
#30263 = CARTESIAN_POINT ( 'NONE',  ( -54.99999999999997868, -52.50000000000000711, -5.000000000000000000 ) ) ;
#30264 = ORIENTED_EDGE ( 'NONE', *, *, #459, .T. ) ;
#30265 = ITEM_DEFINED_TRANSFORMATION ( 'NONE', 'NONE', #21744,  #45486 ) ;
#30266 = VECTOR ( 'NONE', #31877, 1000.000000000000000 ) ;
#30267 = CARTESIAN_POINT ( 'NONE',  ( 0.000000000000000000, 0.000000000000000000, 5.000000000000000000 ) ) ;
#30268 = CARTESIAN_POINT ( 'NONE',  ( 1.114871695981101585, -0.4953159757246433093, 9.963925895596188909 ) ) ;
#30269 = AXIS2_PLACEMENT_3D ( 'NONE', #2381, #45700, #41635 ) ;
#30270 = EDGE_CURVE ( 'NONE', #23377, #418, #4580, .T. ) ;
#30271 = CARTESIAN_POINT ( 'NONE',  ( 8.864235763825218939, 4.693841405978110615, 9.516222621873129839 ) ) ;
#30272 = CARTESIAN_POINT ( 'NONE',  ( 339.9999999999998863, -168.9999999999999432, 343.9999999999997726 ) ) ;
#30273 = ORIENTED_EDGE ( 'NONE', *, *, #36311, .T. ) ;
#30274 = CARTESIAN_POINT ( 'NONE',  ( -4.945973446814903696, 2.143131898507912917E-16, -40.93171244307205825 ) ) ;
#30275 = CARTESIAN_POINT ( 'NONE',  ( 46.76852358249013975, -17.86468378716709537, -9.367992836599954742 ) ) ;
#30276 = CARTESIAN_POINT ( 'NONE',  ( -45.67084718096785423, 1.750000000000010214, -78.15658617722490931 ) ) ;
#30277 = VECTOR ( 'NONE', #10152, 1000.000000000000000 ) ;
#30279 = ORIENTED_EDGE ( 'NONE', *, *, #8769, .F. ) ;
#30278 = EDGE_CURVE ( 'NONE', #9673, #4495, #28440, .T. ) ;
#30280 = CARTESIAN_POINT ( 'NONE',  ( -114.9999999999997158, 17.00000000000000000, -84.99999999999998579 ) ) ;
#30281 = EDGE_CURVE ( 'NONE', #37687, #12617, #24110, .T. ) ;
#30282 = VERTEX_POINT ( 'NONE', #44062 ) ;
#30283 = CARTESIAN_POINT ( 'NONE',  ( -4.945973446814903696, 2.143131898507912917E-16, 159.0682875569279418 ) ) ;
#30284 = ORIENTED_EDGE ( 'NONE', *, *, #44048, .T. ) ;
#30285 = EDGE_CURVE ( 'NONE', #19835, #34493, #20726, .T. ) ;
#30286 = CARTESIAN_POINT ( 'NONE',  ( 210.0000000000000568, 0.000000000000000000, 122.5682875569279844 ) ) ;
#30287 = CARTESIAN_POINT ( 'NONE',  ( -126.6959734468149321, -1.749999999999996891, 160.8182875569279702 ) ) ;
#30288 = EDGE_CURVE ( 'NONE', #11124, #38096, #44307, .T. ) ;
#30289 = ORIENTED_EDGE ( 'NONE', *, *, #12886, .T. ) ;
#30290 = FILL_AREA_STYLE_COLOUR ( '', #33895 ) ;
#30291 = ORIENTED_EDGE ( 'NONE', *, *, #13886, .T. ) ;
#30292 = EDGE_CURVE ( 'NONE', #1914, #21304, #50508, .T. ) ;
#30293 = CYLINDRICAL_SURFACE ( 'NONE', #19339, 1.749999999999973799 ) ;
#30294 = VERTEX_POINT ( 'NONE', #45055 ) ;
#30295 = CARTESIAN_POINT ( 'NONE',  ( 164.9999999999999716, 17.00000000000000000, -85.00000000000001421 ) ) ;
#30296 = DIRECTION ( 'NONE',  ( 0.000000000000000000, 1.000000000000000000, -2.537652627714642000E-15 ) ) ;
#30297 = ORIENTED_EDGE ( 'NONE', *, *, #49715, .F. ) ;
#30298 = CARTESIAN_POINT ( 'NONE',  ( 135.0000000000000000, 17.00000000000000000, -114.9999999999999858 ) ) ;
#30299 = LINE ( 'NONE', #49993, #47955 ) ;
#30300 = EDGE_LOOP ( 'NONE', ( #45138, #38630, #30582, #4860 ) ) ;
#30301 = EDGE_LOOP ( 'NONE', ( #20001, #5368, #702, #11836 ) ) ;
#30302 = CARTESIAN_POINT ( 'NONE',  ( 0.000000000000000000, 183.0000000000000284, -356.0000000000002274 ) ) ;
#30303 = VECTOR ( 'NONE', #20818, 1000.000000000000000 ) ;
#30304 = AXIS2_PLACEMENT_3D ( 'NONE', #29521, #18710, #10023 ) ;
#30305 = ORIENTED_EDGE ( 'NONE', *, *, #21182, .T. ) ;
#30306 = EDGE_CURVE ( 'NONE', #39166, #76, #7563, .T. ) ;
#30307 = CARTESIAN_POINT ( 'NONE',  ( 29.38926261462401257, -40.45084971874711499, 0.000000000000000000 ) ) ;
#30308 = CARTESIAN_POINT ( 'NONE',  ( 0.2553279260466790879, -1.933711247496585184, 9.896382706792378414 ) ) ;
#30309 =( BOUNDED_CURVE ( )  B_SPLINE_CURVE ( 3, ( #9971, #29473, #33336, #28474 ),
 .UNSPECIFIED., .F., .F. ) 
 B_SPLINE_CURVE_WITH_KNOTS ( ( 4, 4 ),
 ( 4.712388980384689674, 6.283185307179586232 ),
 .UNSPECIFIED. ) 
 CURVE ( )  GEOMETRIC_REPRESENTATION_ITEM ( )  RATIONAL_B_SPLINE_CURVE ( ( 1.000000000000000000, 0.8047378541243649375, 0.8047378541243649375, 1.000000000000000000 ) ) 
 REPRESENTATION_ITEM ( '' )  );
#30310 = ORIENTED_EDGE ( 'NONE', *, *, #10182, .F. ) ;
#30311 = CARTESIAN_POINT ( 'NONE',  ( 115.0540265531850395, 2.143131898507847836E-16, 165.0000000000000000 ) ) ;
#30312 = AXIS2_PLACEMENT_3D ( 'NONE', #11314, #19502, #15417 ) ;
#30313 = DIRECTION ( 'NONE',  ( 0.000000000000000000, 0.000000000000000000, 1.000000000000000000 ) ) ;
#30314 = ORIENTED_EDGE ( 'NONE', *, *, #44747, .F. ) ;
#30315 = DIRECTION ( 'NONE',  ( 0.000000000000000000, 0.000000000000000000, 1.000000000000000000 ) ) ;
#30316 = CARTESIAN_POINT ( 'NONE',  ( 12.97493236725083676, -11.05939663306990717, 8.953103998512858652 ) ) ;
#30317 = DIRECTION ( 'NONE',  ( -1.000000000000000000, -0.000000000000000000, -0.000000000000000000 ) ) ;
#30318 = VECTOR ( 'NONE', #17969, 1000.000000000000000 ) ;
#30319 = DIRECTION ( 'NONE',  ( -1.000000000000000000, -0.000000000000000000, -0.000000000000000000 ) ) ;
#30320 = ORIENTED_EDGE ( 'NONE', *, *, #1178, .T. ) ;
#30321 = FACE_OUTER_BOUND ( 'NONE', #12860, .T. ) ;
#30322 = CARTESIAN_POINT ( 'NONE',  ( -12.35406723005387875, 11.51001571518090039, 9.178419661560148768 ) ) ;
#30323 = EDGE_CURVE ( 'NONE', #9008, #5210, #45803, .T. ) ;
#30324 = CARTESIAN_POINT ( 'NONE',  ( 85.00000000000184741, 17.00000000000000000, 90.00000000000000000 ) ) ;
#30325 = EDGE_LOOP ( 'NONE', ( #43600, #50456, #26577, #30429, #39704, #36649 ) ) ;
#30326 = VERTEX_POINT ( 'NONE', #6589 ) ;
#30327 = CARTESIAN_POINT ( 'NONE',  ( 177.5000000000000284, 112.5000000000000000, 0.000000000000000000 ) ) ;
#30328 = CARTESIAN_POINT ( 'NONE',  ( 210.0000000000000568, 0.000000000000000000, 40.81828755692798438 ) ) ;
#30329 = CARTESIAN_POINT ( 'NONE',  ( -69.99999999999816680, 17.00000000000000000, 65.00000000000000000 ) ) ;
#30330 = CARTESIAN_POINT ( 'NONE',  ( -126.6959734468149321, 1.749999999999996891, -159.1817124430720298 ) ) ;
#30331 = DIRECTION ( 'NONE',  ( -0.000000000000000000, -0.000000000000000000, -1.000000000000000000 ) ) ;
#30332 = CARTESIAN_POINT ( 'NONE',  ( 12.78770032058947237, 31.68259716188277864, 7.455576670931136185 ) ) ;
#30333 = ORIENTED_EDGE ( 'NONE', *, *, #43147, .F. ) ;
#30334 = DIRECTION ( 'NONE',  ( 0.000000000000000000, -1.000000000000000000, 0.000000000000000000 ) ) ;
#30335 = CARTESIAN_POINT ( 'NONE',  ( -31.94178169330213279, 9.256608784834037706, -3.760136334089591248 ) ) ;
#30336 = DIRECTION ( 'NONE',  ( 0.000000000000000000, 0.000000000000000000, 1.000000000000000000 ) ) ;
#30337 = AXIS2_PLACEMENT_3D ( 'NONE', #9151, #40466, #40718 ) ;
#30338 = VECTOR ( 'NONE', #11352, 1000.000000000000000 ) ;
#30339 = EDGE_CURVE ( 'NONE', #21405, #34478, #45304, .T. ) ;
#30340 = VECTOR ( 'NONE', #49226, 1000.000000000000000 ) ;
#30341 = SURFACE_STYLE_USAGE ( .BOTH. , #42377 ) ;
#30342 = EDGE_CURVE ( 'NONE', #30870, #10383, #40987, .T. ) ;
#30343 = ORIENTED_EDGE ( 'NONE', *, *, #44643, .T. ) ;
#30344 = VECTOR ( 'NONE', #7875, 1000.000000000000000 ) ;
#30345 = CARTESIAN_POINT ( 'NONE',  ( -165.3973046169136012, 103.9380105690400597, -17.65743994998277699 ) ) ;
#30346 = ORIENTED_EDGE ( 'NONE', *, *, #47426, .T. ) ;
#30347 = CIRCLE ( 'NONE', #49957, 1.750000000000001554 ) ;
#30348 = DIRECTION ( 'NONE',  ( -1.000000000000000000, 0.000000000000000000, 0.000000000000000000 ) ) ;
#30349 = LINE ( 'NONE', #26751, #6922 ) ;
#30350 = CIRCLE ( 'NONE', #22144, 2.000000000000001776 ) ;
#30351 = EDGE_CURVE ( 'NONE', #50360, #7318, #20473, .T. ) ;
#30352 = CARTESIAN_POINT ( 'NONE',  ( 7.398363427652524749, -15.19415887381133246, -9.008049429158102583 ) ) ;
#30353 = ORIENTED_EDGE ( 'NONE', *, *, #23968, .T. ) ;
#30354 = EDGE_CURVE ( 'NONE', #37052, #23178, #41551, .T. ) ;
#30355 = EDGE_CURVE ( 'NONE', #23599, #14979, #14279, .T. ) ;
#30356 = CARTESIAN_POINT ( 'NONE',  ( 0.000000000000000000, -168.9999999999999432, -342.0000000000001705 ) ) ;
#30357 = VERTEX_POINT ( 'NONE', #10687 ) ;
#30358 = CARTESIAN_POINT ( 'NONE',  ( 28.96803024440893992, 18.11533787072037072, 7.455576670931136185 ) ) ;
#30359 = CARTESIAN_POINT ( 'NONE',  ( 166.9999999999999716, -256.4999999999993179, -114.9999999999999574 ) ) ;
#30360 = CARTESIAN_POINT ( 'NONE',  ( -120.0000000000000426, 17.00000000000000000, -114.9999999999999858 ) ) ;
#30361 = EDGE_CURVE ( 'NONE', #2551, #12862, #30096, .T. ) ;
#30362 = EDGE_LOOP ( 'NONE', ( #1011, #43525, #26589, #42132 ) ) ;
#30363 = ORIENTED_EDGE ( 'NONE', *, *, #18018, .F. ) ;
#30364 = CARTESIAN_POINT ( 'NONE',  ( -25.40454589245989325, -27.58367357691681931, -8.192531242611266862 ) ) ;
#30365 = LINE ( 'NONE', #26266, #7492 ) ;
#30366 =( BOUNDED_CURVE ( )  B_SPLINE_CURVE ( 3, ( #46911, #46148, #275, #42835 ),
 .UNSPECIFIED., .F., .F. ) 
 B_SPLINE_CURVE_WITH_KNOTS ( ( 4, 4 ),
 ( 1.570796326794896558, 3.141592653589793116 ),
 .UNSPECIFIED. ) 
 CURVE ( )  GEOMETRIC_REPRESENTATION_ITEM ( )  RATIONAL_B_SPLINE_CURVE ( ( 1.000000000000000000, 0.8047378541243649375, 0.8047378541243649375, 1.000000000000000000 ) ) 
 REPRESENTATION_ITEM ( '' )  );
#30367 = ORIENTED_EDGE ( 'NONE', *, *, #13142, .F. ) ;
#30368 = ORIENTED_EDGE ( 'NONE', *, *, #11144, .F. ) ;
#30369 = CARTESIAN_POINT ( 'NONE',  ( 2.134702841136851603, 5.564253780994583565, -8.944667923005411581E-16 ) ) ;
#30370 = CARTESIAN_POINT ( 'NONE',  ( 15.00000000000000000, -46.01315789473684248, 5.916985404131814619 ) ) ;
#30371 = DIRECTION ( 'NONE',  ( 0.000000000000000000, 1.387778780781444256E-14, -1.000000000000000000 ) ) ;
#30372 = ORIENTED_EDGE ( 'NONE', *, *, #28077, .T. ) ;
#30373 = DIRECTION ( 'NONE',  ( -0.000000000000000000, -0.000000000000000000, -1.000000000000000000 ) ) ;
#30374 = ORIENTED_EDGE ( 'NONE', *, *, #15506, .F. ) ;
#30375 =( BOUNDED_CURVE ( )  B_SPLINE_CURVE ( 3, ( #37061, #2143, #17787, #17533 ),
 .UNSPECIFIED., .F., .F. ) 
 B_SPLINE_CURVE_WITH_KNOTS ( ( 4, 4 ),
 ( 1.570796326794896558, 3.141592653589793116 ),
 .UNSPECIFIED. ) 
 CURVE ( )  GEOMETRIC_REPRESENTATION_ITEM ( )  RATIONAL_B_SPLINE_CURVE ( ( 1.000000000000000000, 0.8047378541243649375, 0.8047378541243649375, 1.000000000000000000 ) ) 
 REPRESENTATION_ITEM ( '' )  );
#30376 = CARTESIAN_POINT ( 'NONE',  ( -46.10908423965022251, -19.89422939639105437, 1.847720168420772691 ) ) ;
#30377 = CARTESIAN_POINT ( 'NONE',  ( 370.7621192902014968, 103.9380105690400597, -17.65743994998277699 ) ) ;
#30378 = VECTOR ( 'NONE', #10977, 1000.000000000000000 ) ;
#30379 = LINE ( 'NONE', #26783, #21420 ) ;
#30380 = VECTOR ( 'NONE', #10356, 1000.000000000000000 ) ;
#30381 = ORIENTED_EDGE ( 'NONE', *, *, #34364, .F. ) ;
#30382 = VERTEX_POINT ( 'NONE', #18378 ) ;
#30383 = EDGE_LOOP ( 'NONE', ( #22399, #47713, #14222, #7031 ) ) ;
#30384 = CARTESIAN_POINT ( 'NONE',  ( 1.193089574352119264, 0.2545860991493882342, 9.963925895596188909 ) ) ;
#30385 = VECTOR ( 'NONE', #38027, 1000.000000000000000 ) ;
#30386 = CARTESIAN_POINT ( 'NONE',  ( -29.39982726364978660, -16.78152490921149109, 8.356839323120299312 ) ) ;
#30387 = ORIENTED_EDGE ( 'NONE', *, *, #16580, .F. ) ;
#30388 = CARTESIAN_POINT ( 'NONE',  ( 0.8965959638259385356, 1.582931917743541028, 9.903764339332076005 ) ) ;
#30389 = AXIS2_PLACEMENT_3D ( 'NONE', #5851, #9697, #48401 ) ;
#30390 = ORIENTED_EDGE ( 'NONE', *, *, #38792, .T. ) ;
#30391 = EDGE_CURVE ( 'NONE', #14610, #44239, #46451, .T. ) ;
#30392 = FACE_OUTER_BOUND ( 'NONE', #48927, .T. ) ;
#30393 = ORIENTED_EDGE ( 'NONE', *, *, #7309, .F. ) ;
#30394 = CARTESIAN_POINT ( 'NONE',  ( -114.9999999999978542, 17.00000000000000000, 95.00000000000000000 ) ) ;
#30395 = CARTESIAN_POINT ( 'NONE',  ( -16.16402646813540755, 4.033894069732547827, -3.546734833711462365 ) ) ;
#30396 = LINE ( 'NONE', #7291, #21659 ) ;
#30397 = EDGE_LOOP ( 'NONE', ( #22651, #27374, #28347, #43745 ) ) ;
#30398 = PLANE ( 'NONE',  #50094 ) ;
#30399 = CARTESIAN_POINT ( 'NONE',  ( 166.9999999999999716, 165.0000000000000000, -356.0000000000001705 ) ) ;
#30400 = CARTESIAN_POINT ( 'NONE',  ( 185.0000000000000000, -180.9999999999999716, -350.0000000000001705 ) ) ;
#30401 = DIRECTION ( 'NONE',  ( -1.000000000000000000, -0.000000000000000000, -0.000000000000000000 ) ) ;
#30402 = DIRECTION ( 'NONE',  ( -1.586032880504786307E-16, 1.654361225106055350E-24, -1.000000000000000000 ) ) ;
#30403 = ADVANCED_FACE ( 'NONE', ( #37162 ), #34058, .T. ) ;
#30404 = CARTESIAN_POINT ( 'NONE',  ( 114.3291528190321173, -1.749999999999996669, -0.2068387089191042749 ) ) ;
#30405 = FACE_OUTER_BOUND ( 'NONE', #40322, .T. ) ;
#30406 = DIRECTION ( 'NONE',  ( 0.000000000000000000, -1.000000000000000000, 0.000000000000000000 ) ) ;
#30407 = AXIS2_PLACEMENT_3D ( 'NONE', #24463, #40361, #28809 ) ;
#30408 = EDGE_CURVE ( 'NONE', #20578, #21162, #48633, .T. ) ;
#30409 = EDGE_CURVE ( 'NONE', #2900, #28813, #13523, .T. ) ;
#30410 = EDGE_LOOP ( 'NONE', ( #47611, #21260, #14409, #46083 ) ) ;
#30411 = FILL_AREA_STYLE_COLOUR ( '', #3498 ) ;
#30412 = CARTESIAN_POINT ( 'NONE',  ( 181.0000000000000000, -79.49999999999995737, -115.0000000000001563 ) ) ;
#30413 = DIRECTION ( 'NONE',  ( -1.000000000000000000, 0.000000000000000000, 0.000000000000000000 ) ) ;
#30414 = EDGE_CURVE ( 'NONE', #42350, #45889, #45510, .T. ) ;
#30415 = DIRECTION ( 'NONE',  ( -1.000000000000000000, 0.000000000000000000, 0.000000000000000000 ) ) ;
#30416 = CARTESIAN_POINT ( 'NONE',  ( -0.9599924130074112272, 0.8495346730527952861, 9.948547179989619238 ) ) ;
#30417 = AXIS2_PLACEMENT_3D ( 'NONE', #17238, #13630, #36762 ) ;
#30418 = ORIENTED_EDGE ( 'NONE', *, *, #4346, .T. ) ;
#30419 = AXIS2_PLACEMENT_3D ( 'NONE', #38627, #39393, #11167 ) ;
#30420 = ORIENTED_EDGE ( 'NONE', *, *, #24236, .T. ) ;
#30421 = DIRECTION ( 'NONE',  ( -0.000000000000000000, -0.000000000000000000, -1.000000000000000000 ) ) ;
#30422 = CARTESIAN_POINT ( 'NONE',  ( -8.001683061421429599, -5.997755262142646870, 9.282506307616484875 ) ) ;
#30423 = ORIENTED_EDGE ( 'NONE', *, *, #41643, .F. ) ;
#30424 = DIRECTION ( 'NONE',  ( -1.860490536778032451E-50, 0.000000000000000000, -1.000000000000000000 ) ) ;
#30425 = CARTESIAN_POINT ( 'NONE',  ( 0.5107275442771160856, 1.175643901748075537, 9.976582533991678048 ) ) ;
#30426 = CARTESIAN_POINT ( 'NONE',  ( 35.05402655318504657, 2.143131898507880377E-16, 165.0000000000000000 ) ) ;
#30427 = VERTEX_POINT ( 'NONE', #9931 ) ;
#30428 = ORIENTED_EDGE ( 'NONE', *, *, #26189, .F. ) ;
#30429 = ORIENTED_EDGE ( 'NONE', *, *, #4280, .T. ) ;
#30430 = DIRECTION ( 'NONE',  ( 1.000000000000000000, 0.000000000000000000, 0.000000000000000000 ) ) ;
#30431 = CYLINDRICAL_SURFACE ( 'NONE', #5397, 1.750000000000015543 ) ;
#30432 = CARTESIAN_POINT ( 'NONE',  ( -167.4999999999999432, -69.93075758371368522, -120.5992382549688671 ) ) ;
#30433 = ORIENTED_EDGE ( 'NONE', *, *, #45517, .F. ) ;
#30434 = CARTESIAN_POINT ( 'NONE',  ( -34.91952936320829792, 13.67027684621028349, -9.422646554964178023 ) ) ;
#30435 = CARTESIAN_POINT ( 'NONE',  ( -204.9459734468149463, 2.143131898507880377E-16, 2.568287556927978166 ) ) ;
#30436 = PLANE ( 'NONE',  #16352 ) ;
#30437 = ORIENTED_EDGE ( 'NONE', *, *, #41290, .F. ) ;
#30438 = ORIENTED_EDGE ( 'NONE', *, *, #39696, .F. ) ;
#30439 = LINE ( 'NONE', #39169, #33648 ) ;
#30440 = SURFACE_STYLE_FILL_AREA ( #3745 ) ;
#30441 = AXIS2_PLACEMENT_3D ( 'NONE', #17458, #25928, #25414 ) ;
#30442 = CARTESIAN_POINT ( 'NONE',  ( 73.30402655318508209, -1.750000000000010658, 80.81828755692798438 ) ) ;
#30443 = ORIENTED_EDGE ( 'NONE', *, *, #41222, .F. ) ;
#30444 = ORIENTED_EDGE ( 'NONE', *, *, #44072, .T. ) ;
#30445 = ADVANCED_FACE ( 'NONE', ( #17873 ), #33552, .T. ) ;
#30446 = VECTOR ( 'NONE', #21476, 1000.000000000000000 ) ;
#30447 = FACE_OUTER_BOUND ( 'NONE', #19010, .T. ) ;
#30448 = CARTESIAN_POINT ( 'NONE',  ( 350.0000000000001137, 183.0000000000000284, 343.9999999999997726 ) ) ;
#30449 = FACE_OUTER_BOUND ( 'NONE', #34107, .T. ) ;
#30450 = DIRECTION ( 'NONE',  ( 1.000000000000000000, 0.000000000000000000, -1.586032892321652482E-16 ) ) ;
#30451 = CARTESIAN_POINT ( 'NONE',  ( -205.6708471809678827, 1.750000000000010214, -78.15658617722490931 ) ) ;
#30452 = VERTEX_POINT ( 'NONE', #2488 ) ;
#30453 = DIRECTION ( 'NONE',  ( -1.000000000000000000, -0.000000000000000000, -0.000000000000000000 ) ) ;
#30454 = CARTESIAN_POINT ( 'NONE',  ( 344.0000000000000000, -164.9999999999999432, 339.9999999999998295 ) ) ;
#30455 = DIRECTION ( 'NONE',  ( 0.000000000000000000, 0.000000000000000000, 1.000000000000000000 ) ) ;
#30456 = CIRCLE ( 'NONE', #26357, 5.000000000000000000 ) ;
#30457 = PLANE ( 'NONE',  #48960 ) ;
#30458 = FACE_OUTER_BOUND ( 'NONE', #16616, .T. ) ;
#30459 = LINE ( 'NONE', #30723, #10949 ) ;
#30460 = ORIENTED_EDGE ( 'NONE', *, *, #26775, .T. ) ;
#30461 = CARTESIAN_POINT ( 'NONE',  ( 17.51065725283126895, -28.41934970907778890, -9.367992836599954742 ) ) ;
#30462 = CARTESIAN_POINT ( 'NONE',  ( -14.29087950072019098, -9.652079258044555132, 8.727788335465566760 ) ) ;
#30463 = DIRECTION ( 'NONE',  ( 0.000000000000000000, 0.000000000000000000, -1.000000000000000000 ) ) ;
#30464 = ORIENTED_EDGE ( 'NONE', *, *, #11357, .F. ) ;
#30465 = CARTESIAN_POINT ( 'NONE',  ( -114.9999999999994031, 17.00000000000000000, -54.99999999999999289 ) ) ;
#30466 = CARTESIAN_POINT ( 'NONE',  ( 85.00000000000029843, 16.00000000000000000, -84.99999999999998579 ) ) ;
#30467 = ORIENTED_EDGE ( 'NONE', *, *, #17628, .T. ) ;
#30468 = LINE ( 'NONE', #3504, #983 ) ;
#30469 = CARTESIAN_POINT ( 'NONE',  ( 1.411185367335151541, 16.64174154430383012, -9.458680755252684591 ) ) ;
#30470 = EDGE_CURVE ( 'NONE', #27492, #17731, #45320, .T. ) ;
#30471 = PLANE ( 'NONE',  #15013 ) ;
#30472 = CARTESIAN_POINT ( 'NONE',  ( -239.0000000000000853, -165.6999999999999602, 254.8599999999999852 ) ) ;
#30473 = AXIS2_PLACEMENT_3D ( 'NONE', #13145, #10057, #37035 ) ;
#30474 = VERTEX_POINT ( 'NONE', #33803 ) ;
#30475 = DIRECTION ( 'NONE',  ( -1.000000000000000000, -6.938893903907233308E-16, -0.000000000000000000 ) ) ;
#30476 = ORIENTED_EDGE ( 'NONE', *, *, #11819, .F. ) ;
#30477 = ORIENTED_EDGE ( 'NONE', *, *, #21907, .T. ) ;
#30478 = LINE ( 'NONE', #49677, #15612 ) ;
#30479 = ORIENTED_EDGE ( 'NONE', *, *, #19898, .F. ) ;
#30480 = VECTOR ( 'NONE', #28512, 1000.000000000000000 ) ;
#30481 = PLANE ( 'NONE',  #13077 ) ;
#30482 = CYLINDRICAL_SURFACE ( 'NONE', #35590, 1.750000000000001554 ) ;
#30483 = CARTESIAN_POINT ( 'NONE',  ( -208.4459734468149463, 0.000000000000000000, -120.9317124430720156 ) ) ;
#30484 = CARTESIAN_POINT ( 'NONE',  ( -47.72109971266203132, -1.750000000000010214, 119.7931612910808781 ) ) ;
#30485 = FACE_OUTER_BOUND ( 'NONE', #12952, .T. ) ;
#30486 = ORIENTED_EDGE ( 'NONE', *, *, #29139, .F. ) ;
#30487 = EDGE_CURVE ( 'NONE', #15638, #43597, #3084, .T. ) ;
#30488 = CARTESIAN_POINT ( 'NONE',  ( -0.9602803029231570253, 0.8490247040095960651, 9.976582533991679824 ) ) ;
#30489 = CARTESIAN_POINT ( 'NONE',  ( 214.9999999999999432, 173.0000000000000000, 112.0000000000000000 ) ) ;
#30490 = DIRECTION ( 'NONE',  ( -0.000000000000000000, -0.000000000000000000, -1.000000000000000000 ) ) ;
#30491 = DIRECTION ( 'NONE',  ( 1.000000000000000000, 0.000000000000000000, 0.000000000000000000 ) ) ;
#30492 = ORIENTED_EDGE ( 'NONE', *, *, #14284, .F. ) ;
#30493 = CARTESIAN_POINT ( 'NONE',  ( -167.7210997126620384, -1.750000000000009548, 41.84341382277508359 ) ) ;
#30494 = PLANE ( 'NONE',  #41696 ) ;
#30495 = VERTEX_POINT ( 'NONE', #31224 ) ;
#30496 = EDGE_LOOP ( 'NONE', ( #42822, #38532, #13931, #18449, #5930, #17356 ) ) ;
#30497 = VERTEX_POINT ( 'NONE', #23771 ) ;
#30498 = LINE ( 'NONE', #30005, #40167 ) ;
#30499 = VECTOR ( 'NONE', #4183, 1000.000000000000000 ) ;
#30500 = LINE ( 'NONE', #6643, #27514 ) ;
#30501 = EDGE_CURVE ( 'NONE', #15139, #11317, #50658, .T. ) ;
#30502 = ORIENTED_EDGE ( 'NONE', *, *, #4826, .T. ) ;
#30503 = CARTESIAN_POINT ( 'NONE',  ( 195.0540265531851105, 2.143131898507880377E-16, 165.0000000000000000 ) ) ;
#30504 = SURFACE_SIDE_STYLE ('',( #3812 ) ) ;
#30505 =( BOUNDED_CURVE ( )  B_SPLINE_CURVE ( 3, ( #20091, #27556, #11380, #35780 ),
 .UNSPECIFIED., .F., .F. ) 
 B_SPLINE_CURVE_WITH_KNOTS ( ( 4, 4 ),
 ( 5.723266580096323608, 6.843104034262848856 ),
 .UNSPECIFIED. ) 
 CURVE ( )  GEOMETRIC_REPRESENTATION_ITEM ( )  RATIONAL_B_SPLINE_CURVE ( ( 1.000000000000000000, 0.8981988528445483677, 0.8981988528445483677, 1.000000000000000000 ) ) 
 REPRESENTATION_ITEM ( '' )  );
#30506 = CARTESIAN_POINT ( 'NONE',  ( 112.2789002873379758, 1.749999999999996891, 39.79316129108089228 ) ) ;
#30507 = DIRECTION ( 'NONE',  ( -3.364279341222519273E-16, 0.7071067811865474617, -0.7071067811865476838 ) ) ;
#30508 = DIRECTION ( 'NONE',  ( -0.000000000000000000, -0.000000000000000000, -1.000000000000000000 ) ) ;
#30509 = VECTOR ( 'NONE', #23240, 1000.000000000000000 ) ;
#30510 = CARTESIAN_POINT ( 'NONE',  ( 24.47767542868285062, -23.18653802921781448, 8.807470649214879543 ) ) ;
#30511 =( BOUNDED_CURVE ( )  B_SPLINE_CURVE ( 3, ( #11325, #18509, #34955, #42863 ),
 .UNSPECIFIED., .F., .F. ) 
 B_SPLINE_CURVE_WITH_KNOTS ( ( 4, 4 ),
 ( 0.000000000000000000, 1.570796326794896558 ),
 .UNSPECIFIED. ) 
 CURVE ( )  GEOMETRIC_REPRESENTATION_ITEM ( )  RATIONAL_B_SPLINE_CURVE ( ( 1.000000000000000000, 0.8047378541243649375, 0.8047378541243649375, 1.000000000000000000 ) ) 
 REPRESENTATION_ITEM ( '' )  );
#30512 = AXIS2_PLACEMENT_3D ( 'NONE', #9308, #6457, #17510 ) ;
#30513 = CARTESIAN_POINT ( 'NONE',  ( -12.78770032058971395, -31.68259716188267916, 7.455576670931136185 ) ) ;
#30514 = VECTOR ( 'NONE', #19989, 1000.000000000000000 ) ;
#30515 = ORIENTED_EDGE ( 'NONE', *, *, #27734, .T. ) ;
#30516 = LINE ( 'NONE', #46884, #33930 ) ;
#30517 = CARTESIAN_POINT ( 'NONE',  ( 350.0000000000000000, -180.9999999999999716, -342.0000000000001705 ) ) ;
#30518 = AXIS2_PLACEMENT_3D ( 'NONE', #9848, #29603, #30818 ) ;
#30519 = CARTESIAN_POINT ( 'NONE',  ( -124.9459734468149463, 2.143131898507847836E-16, 122.5682875569279560 ) ) ;
#30520 = LINE ( 'NONE', #42560, #34717 ) ;
#30521 = ORIENTED_EDGE ( 'NONE', *, *, #17701, .F. ) ;
#30522 = CARTESIAN_POINT ( 'NONE',  ( -24.39427009666018265, -44.07992421011638129, 8.807470649214879543 ) ) ;
#30523 = DIRECTION ( 'NONE',  ( 0.000000000000000000, 0.000000000000000000, 1.000000000000000000 ) ) ;
#30524 = B_SPLINE_CURVE_WITH_KNOTS ( 'NONE', 3,
 ( #32638, #32130, #12615, #43915 ),
 .UNSPECIFIED., .F., .F.,
 ( 4, 4 ),
 ( 0.001403500796105004635, 0.001586656765099030445 ),
 .UNSPECIFIED. ) ;
#30525 =( BOUNDED_CURVE ( )  B_SPLINE_CURVE ( 3, ( #7097, #10682, #6841, #22736 ),
 .UNSPECIFIED., .F., .F. ) 
 B_SPLINE_CURVE_WITH_KNOTS ( ( 4, 4 ),
 ( 4.712388980384689674, 6.283185307179586232 ),
 .UNSPECIFIED. ) 
 CURVE ( )  GEOMETRIC_REPRESENTATION_ITEM ( )  RATIONAL_B_SPLINE_CURVE ( ( 1.000000000000000000, 0.8047378541243649375, 0.8047378541243649375, 1.000000000000000000 ) ) 
 REPRESENTATION_ITEM ( '' )  );
#30526 = CARTESIAN_POINT ( 'NONE',  ( 33.01266944765062306, -5.813986777101467496, 1.847720168420772691 ) ) ;
#30527 = CARTESIAN_POINT ( 'NONE',  ( -8.277096487746778308, 33.14818118907697198, 7.455576670931136185 ) ) ;
#30528 = PRESENTATION_STYLE_ASSIGNMENT (( #25933 ) ) ;
#30529 = EDGE_LOOP ( 'NONE', ( #44788, #24047, #38919, #46715 ) ) ;
#30530 = ADVANCED_FACE ( 'NONE', ( #15811 ), #46814, .F. ) ;
#30531 = CARTESIAN_POINT ( 'NONE',  ( 35.05402655318504657, -1.025126265847089435, 82.56828755692798438 ) ) ;
#30532 = VERTEX_POINT ( 'NONE', #42243 ) ;
#30533 = EDGE_CURVE ( 'NONE', #34291, #9471, #30712, .T. ) ;
#30534 = CARTESIAN_POINT ( 'NONE',  ( 17.23491422248386584, -0.5912720620000816441, 8.727788335465566760 ) ) ;
#30535 = VERTEX_POINT ( 'NONE', #3481 ) ;
#30536 = CARTESIAN_POINT ( 'NONE',  ( -84.94597344681494633, 2.143131898507880377E-16, 119.0682875569279702 ) ) ;
#30537 = EDGE_CURVE ( 'NONE', #1161, #5556, #27360, .T. ) ;
#30538 = CARTESIAN_POINT ( 'NONE',  ( 74.32915281903215998, -1.750000000000009548, -38.15658617722494483 ) ) ;
#30539 = VECTOR ( 'NONE', #48987, 1000.000000000000000 ) ;
#30540 = VERTEX_POINT ( 'NONE', #50407 ) ;
#30541 = DIRECTION ( 'NONE',  ( 0.000000000000000000, 2.969158215481698263E-48, -1.000000000000000000 ) ) ;
#30542 = ORIENTED_EDGE ( 'NONE', *, *, #46578, .F. ) ;
#30543 = EDGE_CURVE ( 'NONE', #48807, #7917, #29323, .T. ) ;
#30544 = ADVANCED_FACE ( 'NONE', ( #50140 ), #3228, .T. ) ;
#30545 = ORIENTED_EDGE ( 'NONE', *, *, #39942, .T. ) ;
#30546 = LINE ( 'NONE', #6941, #40959 ) ;
#30547 = DIRECTION ( 'NONE',  ( 0.000000000000000000, -1.000000000000000000, 2.537652627714642000E-15 ) ) ;
#30548 = CIRCLE ( 'NONE', #37125, 40.00000000000000000 ) ;
#30549 = ORIENTED_EDGE ( 'NONE', *, *, #9629, .F. ) ;
#30550 = LINE ( 'NONE', #7201, #4925 ) ;
#30551 = CARTESIAN_POINT ( 'NONE',  ( 236.0000000000000000, -169.9999999999999716, 4.999999999999616307 ) ) ;
#30552 = AXIS2_PLACEMENT_3D ( 'NONE', #35660, #19973, #20474 ) ;
#30553 = DIRECTION ( 'NONE',  ( -1.000000000000000000, 0.000000000000000000, 0.000000000000000000 ) ) ;
#30554 = VERTEX_POINT ( 'NONE', #8125 ) ;
#30555 = ORIENTED_EDGE ( 'NONE', *, *, #30470, .F. ) ;
#30556 = CARTESIAN_POINT ( 'NONE',  ( 1.133908876584335257, 0.5183204401656757998, 9.981352469109932457 ) ) ;
#30557 = VECTOR ( 'NONE', #40760, 1000.000000000000000 ) ;
#30558 = LINE ( 'NONE', #15919, #19003 ) ;
#30559 = ORIENTED_EDGE ( 'NONE', *, *, #4042, .T. ) ;
#30560 = VECTOR ( 'NONE', #25894, 1000.000000000000000 ) ;
#30561 = LINE ( 'NONE', #22342, #4605 ) ;
#30562 = DIRECTION ( 'NONE',  ( -1.000000000000000000, 0.000000000000000000, 0.000000000000000000 ) ) ;
#30563 = ORIENTED_EDGE ( 'NONE', *, *, #6602, .F. ) ;
#30564 = DIRECTION ( 'NONE',  ( 1.000000000000000000, 0.000000000000000000, 0.000000000000000000 ) ) ;
#30565 = CARTESIAN_POINT ( 'NONE',  ( 154.3291528190321458, 1.750000000000010214, -80.20683870891910772 ) ) ;
#30566 = B_SPLINE_SURFACE_WITH_KNOTS ( 'NONE', 3, 3, ( 
 ( #43460, #15501, #31171, #46759 ),
 ( #35283, #11661, #27314, #24481 ),
 ( #24985, #21118, #36552, #44699 ),
 ( #44941, #20870, #17279, #29576 ) ),
 .UNSPECIFIED., .F., .F., .F.,
 ( 4, 4 ),
 ( 4, 4 ),
 ( 0.000000000000000000, 1.000000000000000000 ),
 ( 0.000000000000000000, 1.000000000000000000 ),
 .UNSPECIFIED. ) ;
#30567 = EDGE_CURVE ( 'NONE', #40195, #9063, #42485, .T. ) ;
#30568 = VERTEX_POINT ( 'NONE', #22986 ) ;
#30569 = EDGE_CURVE ( 'NONE', #18575, #13303, #7103, .T. ) ;
#30570 = FACE_OUTER_BOUND ( 'NONE', #40458, .T. ) ;
#30571 = CARTESIAN_POINT ( 'NONE',  ( 168.9999999999999716, -164.9999999999999432, -350.0000000000001705 ) ) ;
#30572 = CYLINDRICAL_SURFACE ( 'NONE', #24643, 2.000000000000001776 ) ;
#30573 = LINE ( 'NONE', #45679, #13247 ) ;
#30574 = EDGE_CURVE ( 'NONE', #48305, #30605, #50297, .T. ) ;
#30575 = ADVANCED_FACE ( 'NONE', ( #30449 ), #46052, .F. ) ;
#30576 = VECTOR ( 'NONE', #28121, 1000.000000000000000 ) ;
#30577 = ORIENTED_EDGE ( 'NONE', *, *, #27779, .F. ) ;
#30578 = CYLINDRICAL_SURFACE ( 'NONE', #25333, 1.750000000000015543 ) ;
#30579 = ADVANCED_FACE ( 'NONE', ( #22743 ), #23243, .T. ) ;
#30580 = CARTESIAN_POINT ( 'NONE',  ( 169.0000000000000000, 2.775557561562891351E-14, -99.00000000000014211 ) ) ;
#30581 = ADVANCED_FACE ( 'NONE', ( #7357 ), #38663, .T. ) ;
#30582 = ORIENTED_EDGE ( 'NONE', *, *, #24918, .F. ) ;
#30583 = ORIENTED_EDGE ( 'NONE', *, *, #30634, .T. ) ;
#30584 = LINE ( 'NONE', #26227, #43267 ) ;
#30585 = CARTESIAN_POINT ( 'NONE',  ( 155.0540265531850537, 2.143131898507880377E-16, 2.568287556927978166 ) ) ;
#30586 = FILL_AREA_STYLE ('',( #11593 ) ) ;
#30587 = CIRCLE ( 'NONE', #39719, 4.000000000000003553 ) ;
#30588 = FACE_OUTER_BOUND ( 'NONE', #11368, .T. ) ;
#30589 = VERTEX_POINT ( 'NONE', #39181 ) ;
#30590 = CARTESIAN_POINT ( 'NONE',  ( -0.3862712429686729343, -1.188820645368946050, 3.333333333333333481 ) ) ;
#30591 = AXIS2_PLACEMENT_3D ( 'NONE', #45507, #26546, #25791 ) ;
#30592 = CARTESIAN_POINT ( 'NONE',  ( -0.3862712429686809279, -1.188820645368943163, -3.333333333333333481 ) ) ;
#30593 = CARTESIAN_POINT ( 'NONE',  ( -0.2257686176856275040, 1.281370980887437838, 9.986087673579199020 ) ) ;
#30594 = EDGE_CURVE ( 'NONE', #302, #30568, #174, .T. ) ;
#30595 = VECTOR ( 'NONE', #2818, 1000.000000000000000 ) ;
#30596 = ADVANCED_FACE ( 'NONE', ( #5013 ), #9124, .F. ) ;
#30597 = ORIENTED_EDGE ( 'NONE', *, *, #24146, .T. ) ;
#30598 = EDGE_CURVE ( 'NONE', #23271, #47489, #50550, .T. ) ;
#30599 = VECTOR ( 'NONE', #10398, 1000.000000000000000 ) ;
#30600 = CARTESIAN_POINT ( 'NONE',  ( 7.129058724844953510, 15.30620660340485095, 9.178419661560148768 ) ) ;
#30601 = ORIENTED_EDGE ( 'NONE', *, *, #11386, .F. ) ;
#30602 = DIRECTION ( 'NONE',  ( -0.000000000000000000, -0.000000000000000000, -1.000000000000000000 ) ) ;
#30603 = CARTESIAN_POINT ( 'NONE',  ( 343.9999999999999432, -185.0000000000001421, 360.0000000000001137 ) ) ;
#30604 = CARTESIAN_POINT ( 'NONE',  ( -45.67084718096785423, 1.750000000000009548, 159.7931612910809065 ) ) ;
#30605 = VERTEX_POINT ( 'NONE', #48327 ) ;
#30606 = VECTOR ( 'NONE', #18562, 1000.000000000000000 ) ;
#30607 = FACE_OUTER_BOUND ( 'NONE', #16824, .T. ) ;
#30608 = CARTESIAN_POINT ( 'NONE',  ( -114.9999999999991047, 16.00000000000000000, -24.99999999999999289 ) ) ;
#30609 = ORIENTED_EDGE ( 'NONE', *, *, #13012, .T. ) ;
#30610 = CARTESIAN_POINT ( 'NONE',  ( 1.275994128725544741, -0.1230186051320594776, 9.948547179989619238 ) ) ;
#30611 =( BOUNDED_CURVE ( )  B_SPLINE_CURVE ( 3, ( #16350, #50442, #31259, #31513 ),
 .UNSPECIFIED., .F., .F. ) 
 B_SPLINE_CURVE_WITH_KNOTS ( ( 4, 4 ),
 ( 4.712388980384689674, 6.283185307179586232 ),
 .UNSPECIFIED. ) 
 CURVE ( )  GEOMETRIC_REPRESENTATION_ITEM ( )  RATIONAL_B_SPLINE_CURVE ( ( 1.000000000000000000, 0.8047378541243649375, 0.8047378541243649375, 1.000000000000000000 ) ) 
 REPRESENTATION_ITEM ( '' )  );
#30612 = CARTESIAN_POINT ( 'NONE',  ( 154.3291528190321458, -1.750000000000009548, -78.15658617722490931 ) ) ;
#30613 = LINE ( 'NONE', #42647, #13555 ) ;
#30614 = EDGE_CURVE ( 'NONE', #20642, #49743, #12954, .T. ) ;
#30615 = ORIENTED_EDGE ( 'NONE', *, *, #43218, .T. ) ;
#30616 = VERTEX_POINT ( 'NONE', #20160 ) ;
#30617 = CARTESIAN_POINT ( 'NONE',  ( -6.408332700304190332, -7.676800896350769676, 0.000000000000000000 ) ) ;
#30618 = PLANE ( 'NONE',  #28765 ) ;
#30619 = VERTEX_POINT ( 'NONE', #36091 ) ;
#30620 = EDGE_LOOP ( 'NONE', ( #4068, #46727, #915, #23818, #31006, #27951 ) ) ;
#30621 = CARTESIAN_POINT ( 'NONE',  ( 191.5540265531850537, 1.025126265847089435, -77.43171244307200141 ) ) ;
#30622 = DIRECTION ( 'NONE',  ( -1.000000000000000000, -0.000000000000000000, -0.000000000000000000 ) ) ;
#30623 = VECTOR ( 'NONE', #26699, 1000.000000000000000 ) ;
#30624 = CARTESIAN_POINT ( 'NONE',  ( 342.8284271247462698, 167.0000000000000000, 341.9999999999998863 ) ) ;
#30625 = EDGE_CURVE ( 'NONE', #41656, #14966, #16098, .T. ) ;
#30626 = VERTEX_POINT ( 'NONE', #32491 ) ;
#30627 = DIRECTION ( 'NONE',  ( -1.586032892321652236E-16, -1.000000000000000000, -2.288264760618012091E-48 ) ) ;
#30628 = VECTOR ( 'NONE', #27183, 1000.000000000000000 ) ;
#30629 = EDGE_LOOP ( 'NONE', ( #50678, #31988, #28079, #14485 ) ) ;
#30630 = CARTESIAN_POINT ( 'NONE',  ( 350.0000000000001137, 181.0000000000000284, 355.9999999999997726 ) ) ;
#30631 = CARTESIAN_POINT ( 'NONE',  ( 195.0540265531851105, 2.143131898507880377E-16, 82.56828755692798438 ) ) ;
#30632 = VECTOR ( 'NONE', #17936, 1000.000000000000000 ) ;
#30633 = CARTESIAN_POINT ( 'NONE',  ( -48.44597344681495343, 0.000000000000000000, -120.9317124430720725 ) ) ;
#30634 = EDGE_CURVE ( 'NONE', #30766, #40036, #11644, .T. ) ;
#30636 = VERTEX_POINT ( 'NONE', #32727 ) ;
#30635 = ADVANCED_FACE ( 'NONE', ( #24024, #28613, #17071, #9372, #1186 ), #4269, .T. ) ;
#30637 = ORIENTED_EDGE ( 'NONE', *, *, #44681, .T. ) ;
#30638 = EDGE_LOOP ( 'NONE', ( #31051, #50077, #29949, #20830, #34679, #29982 ) ) ;
#30639 = CARTESIAN_POINT ( 'NONE',  ( -64.99999999999815259, 17.00000000000000000, 90.00000000000000000 ) ) ;
#30640 = CARTESIAN_POINT ( 'NONE',  ( -206.6959734468149463, 0.000000000000000000, 165.0000000000000000 ) ) ;
#30641 = EDGE_CURVE ( 'NONE', #25157, #5959, #19905, .T. ) ;
#30642 = ORIENTED_EDGE ( 'NONE', *, *, #36594, .T. ) ;
#30644 = B_SPLINE_CURVE_WITH_KNOTS ( 'NONE', 3,
 ( #41230, #1248, #21231, #44546 ),
 .UNSPECIFIED., .F., .F.,
 ( 4, 4 ),
 ( 0.000000000000000000, 0.2545280377015989859 ),
 .UNSPECIFIED. ) ;
#30643 = CARTESIAN_POINT ( 'NONE',  ( -4.999999999999997335, 204.9999999999999716, -230.2499999999999716 ) ) ;
#30645 = ORIENTED_EDGE ( 'NONE', *, *, #10801, .F. ) ;
#30646 = EDGE_CURVE ( 'NONE', #17811, #18412, #5270, .T. ) ;
#30647 = CARTESIAN_POINT ( 'NONE',  ( 0.000000000000000000, 0.000000000000000000, 10.00000000000000000 ) ) ;
#30648 = EDGE_LOOP ( 'NONE', ( #48363, #20003, #26420, #33371, #5231, #27706 ) ) ;
#30649 = EDGE_CURVE ( 'NONE', #39727, #29268, #27681, .T. ) ;
#30650 = CARTESIAN_POINT ( 'NONE',  ( 33.30402655318503946, -1.750000000000009992, 160.8182875569279702 ) ) ;
#30651 = CARTESIAN_POINT ( 'NONE',  ( 177.5000000000000284, -112.5000000000000000, -10.00000000000000000 ) ) ;
#30652 = CARTESIAN_POINT ( 'NONE',  ( 5.888214538810389698, 16.20866436362417673, 8.727788335465566760 ) ) ;
#30653 = DIRECTION ( 'NONE',  ( 1.000000000000000000, 0.000000000000000000, 0.000000000000000000 ) ) ;
#30654 = VECTOR ( 'NONE', #38418, 1000.000000000000000 ) ;
#30655 = CARTESIAN_POINT ( 'NONE',  ( 0.000000000000000000, 181.0000000000000284, 341.9999999999997726 ) ) ;
#30656 = ORIENTED_EDGE ( 'NONE', *, *, #5208, .T. ) ;
#30657 = DIRECTION ( 'NONE',  ( -0.000000000000000000, -0.000000000000000000, -1.000000000000000000 ) ) ;
#30658 = CARTESIAN_POINT ( 'NONE',  ( 31.55402655318503236, 1.025126265847089213, -160.9317124430720014 ) ) ;
#30659 = ADVANCED_FACE ( 'NONE', ( #39679 ), #47325, .F. ) ;
#30660 = CARTESIAN_POINT ( 'NONE',  ( -5.000000000000000000, -184.7999999999999545, 359.7999999999997840 ) ) ;
#30661 = CARTESIAN_POINT ( 'NONE',  ( -210.0000000000000568, 0.000000000000000000, -159.1817124430720298 ) ) ;
#30662 = DIRECTION ( 'NONE',  ( 0.000000000000000000, 1.000000000000000000, -0.000000000000000000 ) ) ;
#30663 = VECTOR ( 'NONE', #11047, 1000.000000000000000 ) ;
#30664 = VECTOR ( 'NONE', #25069, 1000.000000000000000 ) ;
#30665 = FACE_OUTER_BOUND ( 'NONE', #16178, .T. ) ;
#30666 = AXIS2_PLACEMENT_3D ( 'NONE', #5755, #36839, #29615 ) ;
#30667 = CARTESIAN_POINT ( 'NONE',  ( 167.0000000000000284, 175.0000000000000284, 355.9999999999998863 ) ) ;
#30668 = FACE_OUTER_BOUND ( 'NONE', #46900, .T. ) ;
#30669 = VECTOR ( 'NONE', #12237, 1000.000000000000000 ) ;
#30670 = ORIENTED_EDGE ( 'NONE', *, *, #6252, .T. ) ;
#30671 =( BOUNDED_CURVE ( )  B_SPLINE_CURVE ( 3, ( #34228, #10857, #42912, #19057 ),
 .UNSPECIFIED., .F., .F. ) 
 B_SPLINE_CURVE_WITH_KNOTS ( ( 4, 4 ),
 ( 3.141592653589793116, 4.712388980384689674 ),
 .UNSPECIFIED. ) 
 CURVE ( )  GEOMETRIC_REPRESENTATION_ITEM ( )  RATIONAL_B_SPLINE_CURVE ( ( 1.000000000000000000, 0.8047378541243649375, 0.8047378541243649375, 1.000000000000000000 ) ) 
 REPRESENTATION_ITEM ( '' )  );
#30672 = CARTESIAN_POINT ( 'NONE',  ( 194.9999999999999432, 173.0000000000000000, 132.0000000000000000 ) ) ;
#30673 = CARTESIAN_POINT ( 'NONE',  ( 10.50000000000000178, -46.51315789473684248, -5.916985404131818171 ) ) ;
#30674 = DIRECTION ( 'NONE',  ( -0.4740998230350175202, 0.3386427307392980701, -0.8127425537743157014 ) ) ;
#30675 =( BOUNDED_CURVE ( )  B_SPLINE_CURVE ( 3, ( #6565, #17607, #45779, #21704 ),
 .UNSPECIFIED., .F., .F. ) 
 B_SPLINE_CURVE_WITH_KNOTS ( ( 4, 4 ),
 ( 3.141592653589793116, 4.712388980384689674 ),
 .UNSPECIFIED. ) 
 CURVE ( )  GEOMETRIC_REPRESENTATION_ITEM ( )  RATIONAL_B_SPLINE_CURVE ( ( 1.000000000000000000, 0.8047378541243649375, 0.8047378541243649375, 1.000000000000000000 ) ) 
 REPRESENTATION_ITEM ( '' )  );
#30676 = EDGE_LOOP ( 'NONE', ( #5153, #46016, #15571, #39408 ) ) ;
#30677 = B_SPLINE_SURFACE_WITH_KNOTS ( 'NONE', 3, 3, ( 
 ( #36096, #40438, #938, #9879 ),
 ( #17582, #9129, #9380, #6026 ),
 ( #44761, #24791, #40693, #33256 ),
 ( #32237, #24533, #20931, #48837 ) ),
 .UNSPECIFIED., .F., .F., .F.,
 ( 4, 4 ),
 ( 4, 4 ),
 ( 0.000000000000000000, 1.000000000000000000 ),
 ( 0.000000000000000000, 1.000000000000000000 ),
 .UNSPECIFIED. ) ;
#30678 = EDGE_LOOP ( 'NONE', ( #10869, #36050, #43095, #45747, #49617, #48978, #9511, #17688 ) ) ;
#30679 = LINE ( 'NONE', #7073, #11145 ) ;
#30680 = EDGE_CURVE ( 'NONE', #1904, #28356, #5034, .T. ) ;
#30681 = CARTESIAN_POINT ( 'NONE',  ( 6.174150299305392053, -50.00000000000000711, 8.807470649214879543 ) ) ;
#30682 = AXIS2_PLACEMENT_3D ( 'NONE', #40855, #5702, #10062 ) ;
#30683 = VERTEX_POINT ( 'NONE', #20406 ) ;
#30684 = ORIENTED_EDGE ( 'NONE', *, *, #8028, .F. ) ;
#30685 = CARTESIAN_POINT ( 'NONE',  ( -88.44597344681497475, 0.000000000000000000, -120.9317124430720725 ) ) ;
#30686 = CARTESIAN_POINT ( 'NONE',  ( -208.4459734468148611, 1.025126265847089435, -117.4317124430720156 ) ) ;
#30687 = ORIENTED_EDGE ( 'NONE', *, *, #36525, .F. ) ;
#30688 = ORIENTED_EDGE ( 'NONE', *, *, #19219, .F. ) ;
#30689 = ORIENTED_EDGE ( 'NONE', *, *, #4264, .T. ) ;
#30690 = CARTESIAN_POINT ( 'NONE',  ( 191.5540265531851105, 0.000000000000000000, 159.0682875569279702 ) ) ;
#30691 = DIRECTION ( 'NONE',  ( 0.000000000000000000, 0.000000000000000000, 1.000000000000000000 ) ) ;
#30692 = LINE ( 'NONE', #27090, #10364 ) ;
#30693 = ORIENTED_EDGE ( 'NONE', *, *, #19283, .T. ) ;
#30694 = EDGE_CURVE ( 'NONE', #33167, #25636, #8018, .T. ) ;
#30695 = FACE_OUTER_BOUND ( 'NONE', #8593, .T. ) ;
#30696 = ADVANCED_FACE ( 'NONE', ( #40178 ), #17322, .F. ) ;
#30697 = FACE_OUTER_BOUND ( 'NONE', #40711, .T. ) ;
#30698 = CARTESIAN_POINT ( 'NONE',  ( -128.4459734468149179, 0.000000000000000000, -77.43171244307204404 ) ) ;
#30699 = AXIS2_PLACEMENT_3D ( 'NONE', #47494, #14072, #13133 ) ;
#30700 = ORIENTED_EDGE ( 'NONE', *, *, #42110, .F. ) ;
#30701 = EDGE_LOOP ( 'NONE', ( #24308, #43392, #42965, #14094, #33267, #40532 ) ) ;
#30702 = DIRECTION ( 'NONE',  ( -3.469446951953611231E-16, -0.000000000000000000, -1.000000000000000000 ) ) ;
#30703 = DIRECTION ( 'NONE',  ( 0.000000000000000000, -0.000000000000000000, 1.000000000000000000 ) ) ;
#30704 = CARTESIAN_POINT ( 'NONE',  ( 113.3040265531850537, 1.749999999999997335, -79.18171244307201562 ) ) ;
#30705 = EDGE_CURVE ( 'NONE', #21132, #10463, #44781, .T. ) ;
#30706 = ORIENTED_EDGE ( 'NONE', *, *, #19863, .F. ) ;
#30707 = ORIENTED_EDGE ( 'NONE', *, *, #11067, .F. ) ;
#30708 = AXIS2_PLACEMENT_3D ( 'NONE', #15305, #22976, #7596 ) ;
#30709 = EDGE_CURVE ( 'NONE', #7258, #21648, #45501, .T. ) ;
#30710 = CARTESIAN_POINT ( 'NONE',  ( 7.241383964640743187, 3.469446951953614189E-15, 5.000000000000000000 ) ) ;
#30711 = EDGE_CURVE ( 'NONE', #2022, #46718, #6293, .T. ) ;
#30712 = LINE ( 'NONE', #23520, #47297 ) ;
#30713 = CARTESIAN_POINT ( 'NONE',  ( 35.05402655318504657, 2.143131898507880377E-16, -37.43171244307200141 ) ) ;
#30714 = CARTESIAN_POINT ( 'NONE',  ( -1.035950918207909632, -50.00000000000000711, -2.408242355805840784 ) ) ;
#30715 = ORIENTED_EDGE ( 'NONE', *, *, #38539, .F. ) ;
#30717 = ADVANCED_FACE ( 'NONE', ( #40685 ), #14217, .T. ) ;
#30716 = CARTESIAN_POINT ( 'NONE',  ( 344.0000000000000000, -169.0000000000001137, -349.9999999999998863 ) ) ;
#30718 = DIRECTION ( 'NONE',  ( 0.000000000000000000, 1.000000000000000000, -2.537652627714643577E-15 ) ) ;
#30719 = LINE ( 'NONE', #38421, #36356 ) ;
#30720 = CARTESIAN_POINT ( 'NONE',  ( 114.3291528190321173, 1.749999999999996669, 41.84341382277508359 ) ) ;
#30721 = FACE_OUTER_BOUND ( 'NONE', #13888, .T. ) ;
#30722 = VECTOR ( 'NONE', #50083, 1000.000000000000000 ) ;
#30723 = CARTESIAN_POINT ( 'NONE',  ( 355.9999999999998295, -165.0000000000001137, -110.0000000000002132 ) ) ;
#30724 = AXIS2_PLACEMENT_3D ( 'NONE', #5402, #32365, #16459 ) ;
#30725 = VERTEX_POINT ( 'NONE', #37856 ) ;
#30726 = CARTESIAN_POINT ( 'NONE',  ( 20.40054609052976531, -26.26366202847973597, -3.760136334089591248 ) ) ;
#30727 = LINE ( 'NONE', #27127, #26652 ) ;
#30728 = CARTESIAN_POINT ( 'NONE',  ( -206.6959734468149463, 1.750000000000009992, 160.8182875569279702 ) ) ;
#30729 = VERTEX_POINT ( 'NONE', #18314 ) ;
#30730 = CARTESIAN_POINT ( 'NONE',  ( 7.499999999999944045, -224.9999999999999716, -240.0000000000000000 ) ) ;
#30731 = DIRECTION ( 'NONE',  ( -1.000000000000000000, 0.000000000000000000, 0.000000000000000000 ) ) ;
#30732 = AXIS2_PLACEMENT_3D ( 'NONE', #40393, #5228, #36806 ) ;
#30733 = EDGE_LOOP ( 'NONE', ( #11438, #1293, #39023, #16820 ) ) ;
#30734 = CARTESIAN_POINT ( 'NONE',  ( 153.3040265531850537, 1.750000000000010214, -39.18171244307202983 ) ) ;
#30735 = CARTESIAN_POINT ( 'NONE',  ( 349.9999999999999432, -180.9999999999999716, 343.9999999999997726 ) ) ;
#30736 = DIRECTION ( 'NONE',  ( -1.000000000000000000, 4.996003610813203446E-16, 7.930164450086814785E-16 ) ) ;
#30737 = EDGE_CURVE ( 'NONE', #41895, #38277, #2675, .T. ) ;
#30738 = ORIENTED_EDGE ( 'NONE', *, *, #28369, .T. ) ;
#30739 = CARTESIAN_POINT ( 'NONE',  ( -1.011271242968688533, 0.7347315653655859258, -10.00000000000000000 ) ) ;
#30740 = ORIENTED_EDGE ( 'NONE', *, *, #22443, .T. ) ;
#30741 = ORIENTED_EDGE ( 'NONE', *, *, #30641, .F. ) ;
#30742 = VECTOR ( 'NONE', #22183, 1000.000000000000000 ) ;
#30743 = B_SPLINE_CURVE_WITH_KNOTS ( 'NONE', 3,
 ( #35656, #19968, #31543, #41167 ),
 .UNSPECIFIED., .F., .F.,
 ( 4, 4 ),
 ( 0.000000000000000000, 0.0002520763768929746781 ),
 .UNSPECIFIED. ) ;
#30744 = EDGE_CURVE ( 'NONE', #35238, #11684, #25038, .T. ) ;
#30745 = DIRECTION ( 'NONE',  ( 0.000000000000000000, 0.000000000000000000, 1.000000000000000000 ) ) ;
#30746 = VERTEX_POINT ( 'NONE', #49581 ) ;
#30747 = CARTESIAN_POINT ( 'NONE',  ( 360.0000000000000000, -165.0000000000001137, -94.00000000000019895 ) ) ;
#30748 = DIRECTION ( 'NONE',  ( 1.000000000000000000, 0.000000000000000000, 0.000000000000000000 ) ) ;
#30749 = CARTESIAN_POINT ( 'NONE',  ( 36.28567981536807707, 9.465698090293649614, -9.422646554964174470 ) ) ;
#30750 = FACE_OUTER_BOUND ( 'NONE', #2711, .T. ) ;
#30751 = ORIENTED_EDGE ( 'NONE', *, *, #16465, .F. ) ;
#30752 = LINE ( 'NONE', #39977, #11912 ) ;
#30753 = CARTESIAN_POINT ( 'NONE',  ( 115.0540265531850395, 2.143131898507847836E-16, -120.9317124430720156 ) ) ;
#30754 = CARTESIAN_POINT ( 'NONE',  ( -215.0000000000000568, 164.9999999999999716, 132.0000000000000000 ) ) ;
#30755 = AXIS2_PLACEMENT_3D ( 'NONE', #24547, #20188, #8656 ) ;
#30756 = ORIENTED_EDGE ( 'NONE', *, *, #4186, .T. ) ;
#30757 = CARTESIAN_POINT ( 'NONE',  ( -8.001683061421429599, -5.997755262142646870, 9.282506307616484875 ) ) ;
#30758 = DIRECTION ( 'NONE',  ( 1.000000000000000000, -0.000000000000000000, -0.000000000000000000 ) ) ;
#30759 = ORIENTED_EDGE ( 'NONE', *, *, #26229, .F. ) ;
#30760 = VECTOR ( 'NONE', #20243, 1000.000000000000000 ) ;
#30761 = VERTEX_POINT ( 'NONE', #22189 ) ;
#30762 = ORIENTED_EDGE ( 'NONE', *, *, #36282, .T. ) ;
#30763 = DIRECTION ( 'NONE',  ( -1.000000000000000000, -0.000000000000000000, -0.000000000000000000 ) ) ;
#30764 = AXIS2_PLACEMENT_3D ( 'NONE', #12099, #27245, #39559 ) ;
#30765 = DIRECTION ( 'NONE',  ( 1.000000000000000000, 0.000000000000000000, 0.000000000000000000 ) ) ;
#30766 = VERTEX_POINT ( 'NONE', #5521 ) ;
#30767 = CARTESIAN_POINT ( 'NONE',  ( -1.249999999999999778, 0.000000000000000000, -10.00000000000000000 ) ) ;
#30768 = CARTESIAN_POINT ( 'NONE',  ( -6.695973446814940111, 1.750000000000024203, -119.1817124430720440 ) ) ;
#30769 = CARTESIAN_POINT ( 'NONE',  ( 15.00000000000000000, -46.51315789473684248, 5.916985404131814619 ) ) ;
#30770 = CARTESIAN_POINT ( 'NONE',  ( -3.996390545799824334, 16.57371371864897469, 8.953103998512858652 ) ) ;
#30771 = CYLINDRICAL_SURFACE ( 'NONE', #15680, 1.750000000000001554 ) ;
#30772 = CARTESIAN_POINT ( 'NONE',  ( 73.30402655318508209, -1.750000000000010658, 80.81828755692798438 ) ) ;
#30773 = AXIS2_PLACEMENT_3D ( 'NONE', #36285, #869, #36538 ) ;
#30774 = AXIS2_PLACEMENT_3D ( 'NONE', #50716, #4066, #15867 ) ;
#30775 = CARTESIAN_POINT ( 'NONE',  ( -10.01251772323708522, 8.486842105263161073, -18.46084505325461578 ) ) ;
#30777 = EDGE_CURVE ( 'NONE', #9118, #50130, #16896, .T. ) ;
#30776 = CYLINDRICAL_SURFACE ( 'NONE', #16809, 1.750000000000015543 ) ;
#30778 = DIRECTION ( 'NONE',  ( -0.000000000000000000, -0.000000000000000000, -1.000000000000000000 ) ) ;
#30779 = CARTESIAN_POINT ( 'NONE',  ( 35.00000000000091660, 16.00000000000000000, 0.000000000000000000 ) ) ;
#30780 = AXIS2_PLACEMENT_3D ( 'NONE', #39557, #50527, #42615 ) ;
#30781 = VECTOR ( 'NONE', #43946, 1000.000000000000000 ) ;
#30782 = VERTEX_POINT ( 'NONE', #1682 ) ;
#30783 = CARTESIAN_POINT ( 'NONE',  ( 135.0000000000009663, 17.00000000000000000, 0.000000000000000000 ) ) ;
#30784 = CARTESIAN_POINT ( 'NONE',  ( -8.445973446814964092, -1.025126265847097429, -37.43171244307200851 ) ) ;
#30785 = LINE ( 'NONE', #19207, #50226 ) ;
#30786 = DIRECTION ( 'NONE',  ( 0.000000000000000000, 1.000000000000000000, -1.822804496942680012E-16 ) ) ;
#30787 = VERTEX_POINT ( 'NONE', #21672 ) ;
#30788 = CARTESIAN_POINT ( 'NONE',  ( -27.31081730472607561, -41.96092862852123773, 3.199614146704519602 ) ) ;
#30789 = DIRECTION ( 'NONE',  ( -1.586032892321651989E-16, -1.194346094642793337E-32, -1.000000000000000000 ) ) ;
#30790 = CARTESIAN_POINT ( 'NONE',  ( 1.655083087279030529, -7.799304763725482204, 1.626303258728256651E-16 ) ) ;
#30791 = CARTESIAN_POINT ( 'NONE',  ( 355.9999999999999432, -183.0000000000001421, 358.0000000000001705 ) ) ;
#30792 = DIRECTION ( 'NONE',  ( 0.000000000000000000, -1.000000000000000000, -3.186989995019654210E-49 ) ) ;
#30793 = ORIENTED_EDGE ( 'NONE', *, *, #37131, .F. ) ;
#30794 = AXIS2_PLACEMENT_3D ( 'NONE', #44219, #36056, #638 ) ;
#30795 = CARTESIAN_POINT ( 'NONE',  ( -119.9999999999997158, 16.00000000000000000, -84.99999999999998579 ) ) ;
#30796 = ORIENTED_EDGE ( 'NONE', *, *, #14065, .F. ) ;
#30797 = CARTESIAN_POINT ( 'NONE',  ( 0.3862712429686727678, 1.188820645368945605, 10.00000000000000000 ) ) ;
#30798 = AXIS2_PLACEMENT_3D ( 'NONE', #26781, #31141, #46236 ) ;
#30799 = ORIENTED_EDGE ( 'NONE', *, *, #33841, .F. ) ;
#30800 = PLANE ( 'NONE',  #7424 ) ;
#30801 = CARTESIAN_POINT ( 'NONE',  ( -19.99999999999783995, 17.00000000000000000, 95.00000000000000000 ) ) ;
#30802 = VECTOR ( 'NONE', #34631, 1000.000000000000000 ) ;
#30803 = ORIENTED_EDGE ( 'NONE', *, *, #28107, .T. ) ;
#30804 = CARTESIAN_POINT ( 'NONE',  ( 155.0540265531850537, 1.025126265847089435, 159.0682875569279418 ) ) ;
#30805 = VERTEX_POINT ( 'NONE', #37103 ) ;
#30806 = EDGE_CURVE ( 'NONE', #25400, #27666, #6527, .T. ) ;
#30807 = VECTOR ( 'NONE', #30238, 1000.000000000000000 ) ;
#30808 = ORIENTED_EDGE ( 'NONE', *, *, #16083, .T. ) ;
#30809 = CARTESIAN_POINT ( 'NONE',  ( 168.9999999999999716, -77.49999999999997158, -350.0000000000001705 ) ) ;
#30810 = ORIENTED_EDGE ( 'NONE', *, *, #32807, .F. ) ;
#30811 = CARTESIAN_POINT ( 'NONE',  ( -17.51065725283106289, 28.41934970907792746, -9.367992836599954742 ) ) ;
#30812 = LINE ( 'NONE', #3334, #43920 ) ;
#30813 = DIRECTION ( 'NONE',  ( -1.000000000000000000, -0.000000000000000000, -0.000000000000000000 ) ) ;
#30814 = ORIENTED_EDGE ( 'NONE', *, *, #41962, .T. ) ;
#30815 = ORIENTED_EDGE ( 'NONE', *, *, #46532, .T. ) ;
#30816 = DIRECTION ( 'NONE',  ( -1.000000000000000000, -0.000000000000000000, -0.000000000000000000 ) ) ;
#30817 = AXIS2_PLACEMENT_3D ( 'NONE', #21644, #36822, #41141 ) ;
#30818 = DIRECTION ( 'NONE',  ( -1.000000000000000000, 0.000000000000000000, -0.000000000000000000 ) ) ;
#30819 =( BOUNDED_CURVE ( )  B_SPLINE_CURVE ( 3, ( #44278, #5551, #47607, #1468 ),
 .UNSPECIFIED., .F., .F. ) 
 B_SPLINE_CURVE_WITH_KNOTS ( ( 4, 4 ),
 ( 0.000000000000000000, 1.570796326794896558 ),
 .UNSPECIFIED. ) 
 CURVE ( )  GEOMETRIC_REPRESENTATION_ITEM ( )  RATIONAL_B_SPLINE_CURVE ( ( 1.000000000000000000, 0.8047378541243649375, 0.8047378541243649375, 1.000000000000000000 ) ) 
 REPRESENTATION_ITEM ( '' )  );
#30820 = ORIENTED_EDGE ( 'NONE', *, *, #7027, .T. ) ;
#30821 = LINE ( 'NONE', #22095, #4644 ) ;
#30822 = CARTESIAN_POINT ( 'NONE',  ( -9.563755223200868016, -2.971660568388000634, 3.215106848023638886 ) ) ;
#30823 = VERTEX_POINT ( 'NONE', #17822 ) ;
#30824 = CARTESIAN_POINT ( 'NONE',  ( 1.317555876316863994, 0.4584864758885041081, 9.955131761384825140 ) ) ;
#30825 =( BOUNDED_CURVE ( )  B_SPLINE_CURVE ( 3, ( #3993, #14782, #10928, #26586 ),
 .UNSPECIFIED., .F., .F. ) 
 B_SPLINE_CURVE_WITH_KNOTS ( ( 4, 4 ),
 ( 1.570796326794896558, 3.141592653589793116 ),
 .UNSPECIFIED. ) 
 CURVE ( )  GEOMETRIC_REPRESENTATION_ITEM ( )  RATIONAL_B_SPLINE_CURVE ( ( 1.000000000000000000, 0.8047378541243649375, 0.8047378541243649375, 1.000000000000000000 ) ) 
 REPRESENTATION_ITEM ( '' )  );
#30826 = CARTESIAN_POINT ( 'NONE',  ( 34.38425513258721367, -36.82177522737820397, 8.807470649214879543 ) ) ;
#30827 = ORIENTED_EDGE ( 'NONE', *, *, #189, .T. ) ;
#30828 = B_SPLINE_CURVE_WITH_KNOTS ( 'NONE', 3,
 ( #23052, #3545, #46619, #19194 ),
 .UNSPECIFIED., .F., .F.,
 ( 4, 4 ),
 ( 0.000000000000000000, 0.0003726855806051463586 ),
 .UNSPECIFIED. ) ;
#30829 = CARTESIAN_POINT ( 'NONE',  ( 192.2789002873380184, 1.750000000000009548, -160.2068387089191219 ) ) ;
#30830 = DIRECTION ( 'NONE',  ( -0.000000000000000000, -0.000000000000000000, -1.000000000000000000 ) ) ;
#30831 = LINE ( 'NONE', #34183, #44372 ) ;
#30832 = VECTOR ( 'NONE', #34665, 1000.000000000000000 ) ;
#30833 = VECTOR ( 'NONE', #46424, 1000.000000000000000 ) ;
#30834 = EDGE_LOOP ( 'NONE', ( #3013, #18921 ) ) ;
#30835 = CARTESIAN_POINT ( 'NONE',  ( 0.3370904143228959926, -0.2449105217885284291, 10.00000000000000000 ) ) ;
#30836 = AXIS2_PLACEMENT_3D ( 'NONE', #3930, #19572, #40108 ) ;
#30838 = EDGE_CURVE ( 'NONE', #27903, #48546, #1932, .T. ) ;
#30837 = FILL_AREA_STYLE_COLOUR ( '', #19331 ) ;
#30839 =( BOUNDED_CURVE ( )  B_SPLINE_CURVE ( 3, ( #1793, #5884, #28488, #5627 ),
 .UNSPECIFIED., .F., .F. ) 
 B_SPLINE_CURVE_WITH_KNOTS ( ( 4, 4 ),
 ( 4.712388980384689674, 6.283185307179586232 ),
 .UNSPECIFIED. ) 
 CURVE ( )  GEOMETRIC_REPRESENTATION_ITEM ( )  RATIONAL_B_SPLINE_CURVE ( ( 1.000000000000000000, 0.8047378541243649375, 0.8047378541243649375, 1.000000000000000000 ) ) 
 REPRESENTATION_ITEM ( '' )  );
#30840 = CARTESIAN_POINT ( 'NONE',  ( 0.000000000000000000, 175.0000000000000000, 500.0000000000001137 ) ) ;
#30841 = ORIENTED_EDGE ( 'NONE', *, *, #36336, .T. ) ;
#30842 = ADVANCED_FACE ( 'NONE', ( #30138 ), #33747, .F. ) ;
#30843 = ORIENTED_EDGE ( 'NONE', *, *, #14058, .F. ) ;
#30844 = CARTESIAN_POINT ( 'NONE',  ( 868.6368495446481575, 1209.409171512002558, 1561.339110346518510 ) ) ;
#30845 = ADVANCED_FACE ( 'NONE', ( #13470 ), #9873, .T. ) ;
#30846 = CARTESIAN_POINT ( 'NONE',  ( -125.6708471809678542, -1.749999999999996669, 81.84341382277506227 ) ) ;
#30847 = VECTOR ( 'NONE', #15791, 1000.000000000000000 ) ;
#30848 = CARTESIAN_POINT ( 'NONE',  ( -125.6708471809678542, -1.749999999999996891, -40.20683870891911482 ) ) ;
#30849 = FACE_OUTER_BOUND ( 'NONE', #36786, .T. ) ;
#30850 = LINE ( 'NONE', #26982, #6134 ) ;
#30851 = CARTESIAN_POINT ( 'NONE',  ( 15.73090589902275482, 29.60029367929053024, 1.847720168420772691 ) ) ;
#30852 = ORIENTED_EDGE ( 'NONE', *, *, #44739, .T. ) ;
#30853 = DIRECTION ( 'NONE',  ( 0.000000000000000000, 5.664403186863042467E-17, 1.000000000000000000 ) ) ;
#30854 = ADVANCED_FACE ( 'NONE', ( #49330 ), #2186, .F. ) ;
#30855 = ADVANCED_FACE ( 'NONE', ( #45245 ), #10125, .T. ) ;
#30856 = DIRECTION ( 'NONE',  ( -0.000000000000000000, -1.000000000000000000, -0.000000000000000000 ) ) ;
#30857 = CARTESIAN_POINT ( 'NONE',  ( 115.0540265531850395, 2.143131898507847836E-16, -40.93171244307202983 ) ) ;
#30858 = VECTOR ( 'NONE', #9287, 1000.000000000000000 ) ;
#30859 = EDGE_CURVE ( 'NONE', #16290, #39670, #19593, .T. ) ;
#30860 = DIRECTION ( 'NONE',  ( -1.000000000000000000, 0.000000000000000000, 0.000000000000000000 ) ) ;
#30861 = ORIENTED_EDGE ( 'NONE', *, *, #13656, .T. ) ;
#30862 = CARTESIAN_POINT ( 'NONE',  ( 341.6568542494922553, 165.0000000000001705, -340.0000000000002842 ) ) ;
#30863 = CARTESIAN_POINT ( 'NONE',  ( 210.0000000000000568, 2.143131898507880377E-16, -0.9317124430720331585 ) ) ;
#30864 = VERTEX_POINT ( 'NONE', #15494 ) ;
#30865 = DIRECTION ( 'NONE',  ( -0.000000000000000000, -0.000000000000000000, -1.000000000000000000 ) ) ;
#30866 = LINE ( 'NONE', #14686, #3619 ) ;
#30867 = EDGE_CURVE ( 'NONE', #13154, #38075, #3946, .T. ) ;
#30868 = LINE ( 'NONE', #46458, #47626 ) ;
#30869 = ADVANCED_FACE ( 'NONE', ( #6784 ), #20360, .T. ) ;
#30870 = VERTEX_POINT ( 'NONE', #42178 ) ;
#30871 = ADVANCED_FACE ( 'NONE', ( #10884 ), #26796, .F. ) ;
#30872 = ADVANCED_FACE ( 'NONE', ( #41937 ), #19345, .T. ) ;
#30873 = DIRECTION ( 'NONE',  ( 0.1671032855531282557, 0.5142910309547750192, 0.8411784753765542133 ) ) ;
#30874 = VECTOR ( 'NONE', #29181, 1000.000000000000000 ) ;
#30875 = CARTESIAN_POINT ( 'NONE',  ( 35.05402655318504657, 1.025126265847089435, -40.93171244307204404 ) ) ;
#30876 = ORIENTED_EDGE ( 'NONE', *, *, #24387, .F. ) ;
#30877 = CARTESIAN_POINT ( 'NONE',  ( 181.0000000000000568, 165.0000000000000000, 341.9999999999998863 ) ) ;
#30878 = VECTOR ( 'NONE', #16816, 1000.000000000000000 ) ;
#30879 = CARTESIAN_POINT ( 'NONE',  ( 181.0000000000000000, 175.0000000000000284, -340.0000000000001137 ) ) ;
#30880 = EDGE_CURVE ( 'NONE', #39755, #24104, #41456, .T. ) ;
#30881 = CARTESIAN_POINT ( 'NONE',  ( 342.0000000000000568, 169.0000000000000000, 349.9999999999998863 ) ) ;
#30882 = ADVANCED_FACE ( 'NONE', ( #11652 ), #39204, .T. ) ;
#30883 = ORIENTED_EDGE ( 'NONE', *, *, #31938, .F. ) ;
#30884 = ORIENTED_EDGE ( 'NONE', *, *, #2044, .T. ) ;
#30885 = CARTESIAN_POINT ( 'NONE',  ( -166.6959734468149463, 0.000000000000000000, -165.0000000000000000 ) ) ;
#30886 = DIRECTION ( 'NONE',  ( 1.000000000000000000, -4.758098676964957447E-16, 2.958228394578795584E-31 ) ) ;
#30887 = VERTEX_POINT ( 'NONE', #11392 ) ;
#30888 = EDGE_LOOP ( 'NONE', ( #8565, #8884, #26950, #32641 ) ) ;
#30889 = CARTESIAN_POINT ( 'NONE',  ( 35.35872492446288362, -12.59883863067502929, -2.490396854064191423 ) ) ;
#30890 = CARTESIAN_POINT ( 'NONE',  ( -88.44597344681497475, 0.000000000000000000, 119.0682875569279418 ) ) ;
#30891 = ORIENTED_EDGE ( 'NONE', *, *, #31009, .T. ) ;
#30892 = CARTESIAN_POINT ( 'NONE',  ( 30.00000000000218492, 17.00000000000000000, 115.0000000000000142 ) ) ;
#30893 = ORIENTED_EDGE ( 'NONE', *, *, #48338, .F. ) ;
#30894 = CARTESIAN_POINT ( 'NONE',  ( -47.22310614333779455, -16.46562252335923660, -3.760136334089591248 ) ) ;
#30895 = EDGE_CURVE ( 'NONE', #25557, #24452, #17484, .T. ) ;
#30896 = CIRCLE ( 'NONE', #22666, 2.000000000000001776 ) ;
#30897 = CARTESIAN_POINT ( 'NONE',  ( -69.99999999999847944, 16.00000000000000000, 35.00000000000000000 ) ) ;
#30898 = CARTESIAN_POINT ( 'NONE',  ( 8.277096487746778308, -33.14818118907697198, 7.455576670931136185 ) ) ;
#30899 = EDGE_CURVE ( 'NONE', #10372, #5041, #1754, .T. ) ;
#30900 = EDGE_LOOP ( 'NONE', ( #13117, #26769, #30954, #15385 ) ) ;
#30901 = EDGE_CURVE ( 'NONE', #7812, #32944, #22724, .T. ) ;
#30902 = ORIENTED_EDGE ( 'NONE', *, *, #23146, .T. ) ;
#30903 = ORIENTED_EDGE ( 'NONE', *, *, #9883, .F. ) ;
#30904 = CARTESIAN_POINT ( 'NONE',  ( -7.721099712662037540, 1.750000000000023315, 161.8434138227750907 ) ) ;
#30906 = EDGE_CURVE ( 'NONE', #34157, #30766, #43700, .T. ) ;
#30905 = CARTESIAN_POINT ( 'NONE',  ( -6.695973446814940111, 1.750000000000024203, -79.18171244307201562 ) ) ;
#30907 = CARTESIAN_POINT ( 'NONE',  ( -15.42815683172655028, -34.17926237904570996, 7.697694107796190899 ) ) ;
#30908 = ORIENTED_EDGE ( 'NONE', *, *, #19035, .F. ) ;
#30909 = DIRECTION ( 'NONE',  ( 1.000000000000000000, 0.000000000000000000, 0.000000000000000000 ) ) ;
#30910 = EDGE_LOOP ( 'NONE', ( #14591, #26493, #19073, #27392 ) ) ;
#30911 = ADVANCED_FACE ( 'NONE', ( #28312, #11910 ), #43949, .F. ) ;
#30912 = FACE_OUTER_BOUND ( 'NONE', #34380, .T. ) ;
#30913 = ORIENTED_EDGE ( 'NONE', *, *, #14284, .T. ) ;
#30914 =( NAMED_UNIT ( * ) SI_UNIT ( $, .STERADIAN. ) SOLID_ANGLE_UNIT ( ) );
#30915 = LINE ( 'NONE', #39123, #8034 ) ;
#30916 = CARTESIAN_POINT ( 'NONE',  ( -0.3862712429686809279, -1.188820645368943163, -3.333333333333333481 ) ) ;
#30917 = CARTESIAN_POINT ( 'NONE',  ( -225.0000000000000568, -153.6999999999999602, 250.3600000000000136 ) ) ;
#30918 = VECTOR ( 'NONE', #10438, 1000.000000000000000 ) ;
#30919 = CARTESIAN_POINT ( 'NONE',  ( 0.000000000000000000, 13.48684210526315930, 0.000000000000000000 ) ) ;
#30920 = ORIENTED_EDGE ( 'NONE', *, *, #49745, .T. ) ;
#30921 = VERTEX_POINT ( 'NONE', #8567 ) ;
#30922 = LINE ( 'NONE', #38872, #18162 ) ;
#30923 = CARTESIAN_POINT ( 'NONE',  ( -126.6959734468149321, -1.749999999999997335, 80.81828755692798438 ) ) ;
#30924 = CARTESIAN_POINT ( 'NONE',  ( -168.4459734468149747, 0.000000000000000000, 162.5682875569279702 ) ) ;
#30925 = CARTESIAN_POINT ( 'NONE',  ( -84.94597344681494633, 2.143131898507880377E-16, 165.0000000000000000 ) ) ;
#30926 = ADVANCED_FACE ( 'NONE', ( #27812 ), #39374, .F. ) ;
#30927 = CARTESIAN_POINT ( 'NONE',  ( -2.216591765714429396, 1.436486588196063119, 9.847478953136933555 ) ) ;
#30928 =( BOUNDED_CURVE ( )  B_SPLINE_CURVE ( 3, ( #19258, #34949, #31605, #20284 ),
 .UNSPECIFIED., .F., .F. ) 
 B_SPLINE_CURVE_WITH_KNOTS ( ( 4, 4 ),
 ( 3.141592653589793116, 4.712388980384689674 ),
 .UNSPECIFIED. ) 
 CURVE ( )  GEOMETRIC_REPRESENTATION_ITEM ( )  RATIONAL_B_SPLINE_CURVE ( ( 1.000000000000000000, 0.8047378541243649375, 0.8047378541243649375, 1.000000000000000000 ) ) 
 REPRESENTATION_ITEM ( '' )  );
#30929 = ADVANCED_FACE ( 'NONE', ( #43447 ), #4951, .F. ) ;
#30930 = CARTESIAN_POINT ( 'NONE',  ( -14.29087950072019098, -9.652079258044555132, 8.727788335465566760 ) ) ;
#30931 = ORIENTED_EDGE ( 'NONE', *, *, #2896, .T. ) ;
#30932 = CARTESIAN_POINT ( 'NONE',  ( 0.000000000000000000, 0.000000000000000000, 15.00000000000000000 ) ) ;
#30933 = DIRECTION ( 'NONE',  ( 1.000000000000000000, 0.000000000000000000, -0.000000000000000000 ) ) ;
#30934 = ORIENTED_EDGE ( 'NONE', *, *, #43209, .F. ) ;
#30935 = EDGE_CURVE ( 'NONE', #14506, #3878, #12901, .T. ) ;
#30936 = EDGE_CURVE ( 'NONE', #28855, #9657, #35792, .T. ) ;
#30937 = CARTESIAN_POINT ( 'NONE',  ( -166.6959734468149463, 0.000000000000000000, 165.0000000000000000 ) ) ;
#30938 = CARTESIAN_POINT ( 'NONE',  ( 153.3040265531850537, -1.750000000000010658, 120.8182875569279702 ) ) ;
#30939 = EDGE_CURVE ( 'NONE', #46399, #38860, #31924, .T. ) ;
#30940 = CARTESIAN_POINT ( 'NONE',  ( -88.44597344681497475, 0.000000000000000000, 39.06828755692795596 ) ) ;
#30941 = EDGE_CURVE ( 'NONE', #42239, #41021, #10539, .T. ) ;
#30942 = EDGE_LOOP ( 'NONE', ( #22933, #41847, #3268, #36742, #42402, #31897, #14087, #11136 ) ) ;
#30943 = ORIENTED_EDGE ( 'NONE', *, *, #1719, .F. ) ;
#30944 = CARTESIAN_POINT ( 'NONE',  ( 8.001683061421385190, 5.997755262142701937, 9.282506307616484875 ) ) ;
#30945 = ADVANCED_FACE ( 'NONE', ( #4211 ), #43201, .T. ) ;
#30946 = CARTESIAN_POINT ( 'NONE',  ( 6.875132362119187768, -33.14667368551891258, 8.356839323120299312 ) ) ;
#30947 = VECTOR ( 'NONE', #32231, 1000.000000000000000 ) ;
#30948 = ORIENTED_EDGE ( 'NONE', *, *, #13368, .F. ) ;
#30949 = ORIENTED_EDGE ( 'NONE', *, *, #27379, .F. ) ;
#30950 = CARTESIAN_POINT ( 'NONE',  ( 14.76429217231961566, 8.192625680377691566, 9.178419661560148768 ) ) ;
#30951 = CARTESIAN_POINT ( 'NONE',  ( -6.174150299305392053, 50.00000000000000711, 8.807470649214879543 ) ) ;
#30952 = ORIENTED_EDGE ( 'NONE', *, *, #49111, .T. ) ;
#30953 = ORIENTED_EDGE ( 'NONE', *, *, #42907, .T. ) ;
#30954 = ORIENTED_EDGE ( 'NONE', *, *, #32505, .F. ) ;
#30955 = CARTESIAN_POINT ( 'NONE',  ( 166.9999999999999716, -174.9999999999999716, -344.0000000000001137 ) ) ;
#30956 = CARTESIAN_POINT ( 'NONE',  ( 339.9999999999999432, -164.9999999999999432, -356.0000000000002274 ) ) ;
#30957 = ORIENTED_EDGE ( 'NONE', *, *, #45939, .F. ) ;
#30958 = CARTESIAN_POINT ( 'NONE',  ( 6.408332700304398166, 7.676800896350598258, 0.000000000000000000 ) ) ;
#30959 = EDGE_CURVE ( 'NONE', #22969, #27078, #871, .T. ) ;
#30960 = CARTESIAN_POINT ( 'NONE',  ( 167.0000000000000000, -174.9999999999999716, -111.0000000000001563 ) ) ;
#30961 = CARTESIAN_POINT ( 'NONE',  ( 18.37190376999591024, 32.73290680288470611, 1.982731392810408444 ) ) ;
#30962 = EDGE_LOOP ( 'NONE', ( #50393, #21665, #21434, #29342 ) ) ;
#30963 = ORIENTED_EDGE ( 'NONE', *, *, #38474, .F. ) ;
#30964 = DIRECTION ( 'NONE',  ( 1.000000000000000000, 0.000000000000000000, -0.000000000000000000 ) ) ;
#30965 = DIRECTION ( 'NONE',  ( 0.000000000000000000, 0.000000000000000000, 1.000000000000000000 ) ) ;
#30966 = LINE ( 'NONE', #16064, #5221 ) ;
#30967 = ORIENTED_EDGE ( 'NONE', *, *, #4639, .F. ) ;
#30968 = VERTEX_POINT ( 'NONE', #32168 ) ;
#30969 = DIRECTION ( 'NONE',  ( 1.000000000000000000, 0.000000000000000000, -0.000000000000000000 ) ) ;
#30970 = FILL_AREA_STYLE ('',( #6340 ) ) ;
#30971 = LINE ( 'NONE', #4268, #42726 ) ;
#30972 = DIRECTION ( 'NONE',  ( 0.000000000000000000, 0.000000000000000000, 1.000000000000000000 ) ) ;
#30973 = PLANE ( 'NONE',  #9743 ) ;
#30974 = CARTESIAN_POINT ( 'NONE',  ( 153.3040265531850537, -1.750000000000010214, -39.18171244307202983 ) ) ;
#30975 = VERTEX_POINT ( 'NONE', #35525 ) ;
#30976 = EDGE_CURVE ( 'NONE', #31422, #31585, #47763, .T. ) ;
#30977 = CARTESIAN_POINT ( 'NONE',  ( 71.55402655318505367, 0.000000000000000000, 165.0000000000000000 ) ) ;
#30978 = PLANE ( 'NONE',  #19103 ) ;
#30979 = FACE_OUTER_BOUND ( 'NONE', #17623, .T. ) ;
#30980 = CARTESIAN_POINT ( 'NONE',  ( 32.65539107884896453, 7.204654279306055287, -8.917361510505369182 ) ) ;
#30981 =( BOUNDED_CURVE ( )  B_SPLINE_CURVE ( 3, ( #41660, #22161, #17303, #25254 ),
 .UNSPECIFIED., .F., .F. ) 
 B_SPLINE_CURVE_WITH_KNOTS ( ( 4, 4 ),
 ( 0.000000000000000000, 1.570796326794896558 ),
 .UNSPECIFIED. ) 
 CURVE ( )  GEOMETRIC_REPRESENTATION_ITEM ( )  RATIONAL_B_SPLINE_CURVE ( ( 1.000000000000000000, 0.8047378541243649375, 0.8047378541243649375, 1.000000000000000000 ) ) 
 REPRESENTATION_ITEM ( '' )  );
#30982 = VECTOR ( 'NONE', #42002, 1000.000000000000000 ) ;
#30983 = VERTEX_POINT ( 'NONE', #369 ) ;
#30984 = CARTESIAN_POINT ( 'NONE',  ( 1.249999999999999778, 0.000000000000000000, 10.00000000000000000 ) ) ;
#30985 =( BOUNDED_CURVE ( )  B_SPLINE_CURVE ( 3, ( #8636, #40184, #24534, #44503 ),
 .UNSPECIFIED., .F., .F. ) 
 B_SPLINE_CURVE_WITH_KNOTS ( ( 4, 4 ),
 ( 1.570796326794896558, 3.141592653589793116 ),
 .UNSPECIFIED. ) 
 CURVE ( )  GEOMETRIC_REPRESENTATION_ITEM ( )  RATIONAL_B_SPLINE_CURVE ( ( 1.000000000000000000, 0.8047378541243649375, 0.8047378541243649375, 1.000000000000000000 ) ) 
 REPRESENTATION_ITEM ( '' )  );
#30986 = CARTESIAN_POINT ( 'NONE',  ( 344.0000000000001705, 167.0000000000000000, -342.0000000000001137 ) ) ;
#30987 = CARTESIAN_POINT ( 'NONE',  ( -0.8784099037133121790, -0.8517617868932445546, 9.993783931180535873 ) ) ;
#30988 = VERTEX_POINT ( 'NONE', #23707 ) ;
#30989 = EDGE_CURVE ( 'NONE', #36488, #30988, #19844, .T. ) ;
#30990 = EDGE_CURVE ( 'NONE', #34175, #5984, #32422, .T. ) ;
#30991 = CARTESIAN_POINT ( 'NONE',  ( 72.27890028733797578, -1.750000000000009548, -0.2068387089191121020 ) ) ;
#30992 = ORIENTED_EDGE ( 'NONE', *, *, #38681, .F. ) ;
#30993 = DIRECTION ( 'NONE',  ( 0.000000000000000000, 0.000000000000000000, -1.000000000000000000 ) ) ;
#30994 = CARTESIAN_POINT ( 'NONE',  ( 224.9999999999999716, -164.9999999999999716, 32.29650858650035161 ) ) ;
#30995 = CARTESIAN_POINT ( 'NONE',  ( -19.99999999999971223, 17.00000000000000000, -84.99999999999998579 ) ) ;
#30996 = CARTESIAN_POINT ( 'NONE',  ( -0.9772698688233778519, 0.8109225331901841471, 9.975314328424618182 ) ) ;
#30997 = ADVANCED_FACE ( 'NONE', ( #9568 ), #45436, .T. ) ;
#30998 = EDGE_LOOP ( 'NONE', ( #10376, #22029, #28835, #12394, #50494 ) ) ;
#30999 = CARTESIAN_POINT ( 'NONE',  ( -20.37409433808010562, -26.28007012093468475, -2.408242355805840784 ) ) ;
#31000 = B_SPLINE_SURFACE_WITH_KNOTS ( 'NONE', 3, 3, ( 
 ( #42381, #26492, #35221, #42633 ),
 ( #15203, #34980, #30600, #11345 ),
 ( #50546, #6991, #7766, #65 ),
 ( #50292, #50034, #34455, #7244 ) ),
 .UNSPECIFIED., .F., .F., .F.,
 ( 4, 4 ),
 ( 4, 4 ),
 ( 0.000000000000000000, 1.000000000000000000 ),
 ( 0.000000000000000000, 1.000000000000000000 ),
 .UNSPECIFIED. ) ;
#31001 = EDGE_LOOP ( 'NONE', ( #37450, #3263, #14248, #31772 ) ) ;
#31002 = ORIENTED_EDGE ( 'NONE', *, *, #45602, .F. ) ;
#31003 = EDGE_CURVE ( 'NONE', #1016, #1211, #14153, .T. ) ;
#31004 = FACE_OUTER_BOUND ( 'NONE', #42056, .T. ) ;
#31005 = EDGE_CURVE ( 'NONE', #48177, #32004, #41371, .T. ) ;
#31006 = ORIENTED_EDGE ( 'NONE', *, *, #24668, .F. ) ;
#31007 = CARTESIAN_POINT ( 'NONE',  ( 210.0000000000000568, 0.000000000000000000, -77.43171244307200141 ) ) ;
#31008 = DIRECTION ( 'NONE',  ( -1.000000000000000000, -0.000000000000000000, -0.000000000000000000 ) ) ;
#31009 = EDGE_CURVE ( 'NONE', #44375, #30554, #6464, .T. ) ;
#31010 = CARTESIAN_POINT ( 'NONE',  ( 35.00000000000152767, 17.00000000000000000, 35.00000000000000000 ) ) ;
#31011 = ORIENTED_EDGE ( 'NONE', *, *, #9531, .F. ) ;
#31012 = CARTESIAN_POINT ( 'NONE',  ( 194.9999999999999432, -173.0000000000000000, 112.0000000000000284 ) ) ;
#31013 = CARTESIAN_POINT ( 'NONE',  ( -34.66007756064415446, 14.33302383662612556, -9.011255500499645521 ) ) ;
#31014 = LINE ( 'NONE', #31523, #22584 ) ;
#31015 = ORIENTED_EDGE ( 'NONE', *, *, #20884, .T. ) ;
#31016 = CYLINDRICAL_SURFACE ( 'NONE', #3824, 1.750000000000015543 ) ;
#31017 = CARTESIAN_POINT ( 'NONE',  ( 0.9772698688233751874, -0.8109225331901837031, 9.975314328424616406 ) ) ;
#31018 = ORIENTED_EDGE ( 'NONE', *, *, #43738, .F. ) ;
#31019 = ORIENTED_EDGE ( 'NONE', *, *, #39589, .F. ) ;
#31020 = VERTEX_POINT ( 'NONE', #22122 ) ;
#31021 = CARTESIAN_POINT ( 'NONE',  ( -567.5000000000000000, -72.50000000000001421, -183.5999999999997954 ) ) ;
#31022 = FACE_OUTER_BOUND ( 'NONE', #25877, .T. ) ;
#31023 = ORIENTED_EDGE ( 'NONE', *, *, #48140, .T. ) ;
#31024 = CARTESIAN_POINT ( 'NONE',  ( -36.08557433729205144, 35.58569447144795816, 7.455576670931136185 ) ) ;
#31025 = CARTESIAN_POINT ( 'NONE',  ( -4.999999999999997335, 214.9999999999999716, -230.2499999999999716 ) ) ;
#31026 = CARTESIAN_POINT ( 'NONE',  ( -28.96803024440907137, -18.11533787072017176, 7.455576670931136185 ) ) ;
#31027 = CARTESIAN_POINT ( 'NONE',  ( 181.0000000000000000, -81.49999999999997158, -350.0000000000001705 ) ) ;
#31028 = CARTESIAN_POINT ( 'NONE',  ( -5.647304616913629616, -61.66198943095990614, 22.84256005001721945 ) ) ;
#31029 = CARTESIAN_POINT ( 'NONE',  ( 31.55402655318503236, 0.000000000000000000, -37.43171244307200141 ) ) ;
#31030 = CARTESIAN_POINT ( 'NONE',  ( -206.6959734468149463, 1.750000000000010658, -79.18171244307201562 ) ) ;
#31031 = FACE_OUTER_BOUND ( 'NONE', #35409, .T. ) ;
#31032 = CARTESIAN_POINT ( 'NONE',  ( -114.9999999999984652, 17.00000000000000000, 60.00000000000000000 ) ) ;
#31033 = PLANE ( 'NONE',  #240 ) ;
#31034 = EDGE_CURVE ( 'NONE', #12974, #42730, #28817, .T. ) ;
#31035 = ORIENTED_EDGE ( 'NONE', *, *, #15969, .T. ) ;
#31036 = DIRECTION ( 'NONE',  ( -1.000000000000000000, 0.000000000000000000, 0.000000000000000000 ) ) ;
#31037 = DIRECTION ( 'NONE',  ( -1.000000000000000000, -0.000000000000000000, -0.000000000000000000 ) ) ;
#31038 = CARTESIAN_POINT ( 'NONE',  ( -210.0000000000000568, 0.000000000000000000, 0.8182875569279768335 ) ) ;
#31039 = DIRECTION ( 'NONE',  ( -1.000000000000000000, 0.000000000000000000, -7.793956916774525800E-48 ) ) ;
#31040 = ORIENTED_EDGE ( 'NONE', *, *, #37121, .T. ) ;
#31041 = CARTESIAN_POINT ( 'NONE',  ( 181.0000000000000000, -164.9999999999999432, 359.9999999999997726 ) ) ;
#31042 = DIRECTION ( 'NONE',  ( 1.000000000000000000, 0.000000000000000000, 0.000000000000000000 ) ) ;
#31043 = FACE_OUTER_BOUND ( 'NONE', #10621, .T. ) ;
#31044 = CARTESIAN_POINT ( 'NONE',  ( 2.500000000000050182, -204.9999999999999716, -234.7500000000000000 ) ) ;
#31045 = LINE ( 'NONE', #43834, #11530 ) ;
#31046 = AXIS2_PLACEMENT_3D ( 'NONE', #3755, #8126, #31473 ) ;
#31047 = ORIENTED_EDGE ( 'NONE', *, *, #37602, .F. ) ;
#31048 = CARTESIAN_POINT ( 'NONE',  ( 80.00000000000092371, 17.00000000000000000, 0.000000000000000000 ) ) ;
#31049 = VERTEX_POINT ( 'NONE', #9314 ) ;
#31050 = FACE_OUTER_BOUND ( 'NONE', #30888, .T. ) ;
#31051 = ORIENTED_EDGE ( 'NONE', *, *, #40472, .F. ) ;
#31052 = DIRECTION ( 'NONE',  ( 1.132880637372608740E-16, 4.718402560806925739E-50, 1.000000000000000000 ) ) ;
#31053 = DIRECTION ( 'NONE',  ( -1.612977847700450206E-50, 0.000000000000000000, -1.000000000000000000 ) ) ;
#31054 = VERTEX_POINT ( 'NONE', #33188 ) ;
#31055 = SURFACE_SIDE_STYLE ('',( #15138 ) ) ;
#31056 = VERTEX_POINT ( 'NONE', #49271 ) ;
#31057 = ADVANCED_FACE ( 'NONE', ( #37792 ), #2607, .F. ) ;
#31058 = EDGE_CURVE ( 'NONE', #24452, #27194, #40864, .T. ) ;
#31059 = VERTEX_POINT ( 'NONE', #37047 ) ;
#31060 = DIRECTION ( 'NONE',  ( -0.000000000000000000, -0.000000000000000000, -1.000000000000000000 ) ) ;
#31061 = DIRECTION ( 'NONE',  ( 1.000000000000000000, 0.000000000000000000, 0.000000000000000000 ) ) ;
#31062 = ORIENTED_EDGE ( 'NONE', *, *, #47865, .F. ) ;
#31063 = DIRECTION ( 'NONE',  ( 0.000000000000000000, 0.000000000000000000, -1.000000000000000000 ) ) ;
#31064 = CARTESIAN_POINT ( 'NONE',  ( 356.0000000000000568, -183.0000000000001421, 358.0000000000001705 ) ) ;
#31065 = ADVANCED_FACE ( 'NONE', ( #48774 ), #29825, .T. ) ;
#31066 = ORIENTED_EDGE ( 'NONE', *, *, #47279, .T. ) ;
#31067 = CARTESIAN_POINT ( 'NONE',  ( 210.0000000000000568, 0.000000000000000000, 162.5682875569279702 ) ) ;
#31068 = CARTESIAN_POINT ( 'NONE',  ( 357.9999999999999432, 181.0000000000002558, -356.0000000000003411 ) ) ;
#31069 = ORIENTED_EDGE ( 'NONE', *, *, #29090, .T. ) ;
#31070 = CARTESIAN_POINT ( 'NONE',  ( 37.52258785160491783, 18.42740426802386722, 8.846626183609803462 ) ) ;
#31071 = CARTESIAN_POINT ( 'NONE',  ( -26.64049824243113918, 26.44234984024230073, 4.835783797351798086 ) ) ;
#31072 = ORIENTED_EDGE ( 'NONE', *, *, #27876, .F. ) ;
#31073 = CARTESIAN_POINT ( 'NONE',  ( 1.721971274562253740, 0.09408549481334846365, 9.928159647716247704 ) ) ;
#31074 = CARTESIAN_POINT ( 'NONE',  ( 185.0000000000000000, -93.49999999999998579, -115.0000000000001563 ) ) ;
#31075 = ORIENTED_EDGE ( 'NONE', *, *, #44953, .T. ) ;
#31076 = LINE ( 'NONE', #43361, #33296 ) ;
#31077 = AXIS2_PLACEMENT_3D ( 'NONE', #34718, #31368, #38815 ) ;
#31078 = CARTESIAN_POINT ( 'NONE',  ( 71.55402655318505367, 0.000000000000000000, 159.0682875569279702 ) ) ;
#31079 = CARTESIAN_POINT ( 'NONE',  ( -86.69597344681494633, 1.750000000000009992, 160.8182875569279702 ) ) ;
#31080 = CARTESIAN_POINT ( 'NONE',  ( 0.5107275442771160856, 1.175643901748075537, 9.976582533991678048 ) ) ;
#31081 = AXIS2_PLACEMENT_3D ( 'NONE', #17717, #14103, #17216 ) ;
#31082 = ORIENTED_EDGE ( 'NONE', *, *, #12567, .F. ) ;
#31083 = DIRECTION ( 'NONE',  ( 1.000000000000000000, 0.000000000000000000, 2.958228394578794270E-31 ) ) ;
#31084 = VECTOR ( 'NONE', #3530, 1000.000000000000000 ) ;
#31085 = AXIS2_PLACEMENT_3D ( 'NONE', #22819, #38500, #3313 ) ;
#31086 = DIRECTION ( 'NONE',  ( -0.000000000000000000, -0.000000000000000000, 1.000000000000000000 ) ) ;
#31087 = ORIENTED_EDGE ( 'NONE', *, *, #6372, .F. ) ;
#31088 = EDGE_CURVE ( 'NONE', #47244, #3216, #41116, .T. ) ;
#31089 = VERTEX_POINT ( 'NONE', #44932 ) ;
#31091 = CARTESIAN_POINT ( 'NONE',  ( -4.999999999999997335, 204.9999999999999716, -234.7500000000000000 ) ) ;
#31090 = AXIS2_PLACEMENT_3D ( 'NONE', #9886, #6304, #25796 ) ;
#31092 = CARTESIAN_POINT ( 'NONE',  ( 6.204997580903516941, -7.388441598285492518, 229.0000000000000000 ) ) ;
#31093 = DIRECTION ( 'NONE',  ( -1.000000000000000000, -0.000000000000000000, -0.000000000000000000 ) ) ;
#31094 = CARTESIAN_POINT ( 'NONE',  ( 31.55402655318503236, 1.025126265847089435, -40.93171244307204404 ) ) ;
#31095 = ORIENTED_EDGE ( 'NONE', *, *, #23748, .T. ) ;
#31096 = CARTESIAN_POINT ( 'NONE',  ( 41.59994237955810803, -5.070535260985374215, 7.544061037322996377 ) ) ;
#31097 = PRODUCT_DEFINITION_SHAPE ( 'NONE', 'NONE',  #50732 ) ;
#31098 = DIRECTION ( 'NONE',  ( 0.000000000000000000, 0.000000000000000000, 1.000000000000000000 ) ) ;
#31099 = DIRECTION ( 'NONE',  ( 0.000000000000000000, -0.000000000000000000, -1.000000000000000000 ) ) ;
#31100 = CARTESIAN_POINT ( 'NONE',  ( -206.6959734468149463, 1.750000000000010658, 80.81828755692798438 ) ) ;
#31101 = ORIENTED_EDGE ( 'NONE', *, *, #37898, .F. ) ;
#31102 = FILL_AREA_STYLE ('',( #6730 ) ) ;
#31103 = ORIENTED_EDGE ( 'NONE', *, *, #40374, .T. ) ;
#31104 = CARTESIAN_POINT ( 'NONE',  ( -14.48769039275601145, -30.44468701195584970, 8.807470649214879543 ) ) ;
#31105 = ORIENTED_EDGE ( 'NONE', *, *, #33791, .T. ) ;
#31106 = CYLINDRICAL_SURFACE ( 'NONE', #28733, 1.750000000000008438 ) ;
#31107 = CARTESIAN_POINT ( 'NONE',  ( -119.9999999999990905, 17.00000000000000000, -24.99999999999999289 ) ) ;
#31108 = CARTESIAN_POINT ( 'NONE',  ( 79.99999999999995737, 16.00000000000000000, -114.9999999999999858 ) ) ;
#31109 = VECTOR ( 'NONE', #28720, 1000.000000000000000 ) ;
#31110 = ORIENTED_EDGE ( 'NONE', *, *, #19676, .F. ) ;
#31111 = VECTOR ( 'NONE', #27385, 1000.000000000000000 ) ;
#31112 =( BOUNDED_CURVE ( )  B_SPLINE_CURVE ( 3, ( #4804, #32787, #21219, #44297 ),
 .UNSPECIFIED., .F., .F. ) 
 B_SPLINE_CURVE_WITH_KNOTS ( ( 4, 4 ),
 ( 4.712388980384689674, 6.283185307179586232 ),
 .UNSPECIFIED. ) 
 CURVE ( )  GEOMETRIC_REPRESENTATION_ITEM ( )  RATIONAL_B_SPLINE_CURVE ( ( 1.000000000000000000, 0.8047378541243649375, 0.8047378541243649375, 1.000000000000000000 ) ) 
 REPRESENTATION_ITEM ( '' )  );
#31113 = CIRCLE ( 'NONE', #15545, 33.33601305720110020 ) ;
#31114 = CARTESIAN_POINT ( 'NONE',  ( 210.0000000000000568, 0.000000000000000000, 160.8182875569279702 ) ) ;
#31115 = CARTESIAN_POINT ( 'NONE',  ( 34.32915281903212446, 1.750000000000009548, -40.20683870891912193 ) ) ;
#31116 = ORIENTED_EDGE ( 'NONE', *, *, #33825, .T. ) ;
#31117 = CARTESIAN_POINT ( 'NONE',  ( 80.00000000000092371, 16.00000000000000000, -24.99999999999999289 ) ) ;
#31118 = DIRECTION ( 'NONE',  ( -0.000000000000000000, -0.000000000000000000, -1.000000000000000000 ) ) ;
#31119 = UNCERTAINTY_MEASURE_WITH_UNIT (LENGTH_MEASURE( 1.000000000000000082E-05 ), #19591, 'distance_accuracy_value', 'NONE');
#31120 = DIRECTION ( 'NONE',  ( -0.000000000000000000, -0.000000000000000000, -1.000000000000000000 ) ) ;
#31121 = EDGE_CURVE ( 'NONE', #42239, #13694, #17888, .T. ) ;
#31122 = CIRCLE ( 'NONE', #840, 1.750000000000001554 ) ;
#31123 =( BOUNDED_CURVE ( )  B_SPLINE_CURVE ( 3, ( #23057, #23314, #38988, #15377 ),
 .UNSPECIFIED., .F., .F. ) 
 B_SPLINE_CURVE_WITH_KNOTS ( ( 4, 4 ),
 ( 0.000000000000000000, 1.570796326794896558 ),
 .UNSPECIFIED. ) 
 CURVE ( )  GEOMETRIC_REPRESENTATION_ITEM ( )  RATIONAL_B_SPLINE_CURVE ( ( 1.000000000000000000, 0.8047378541243649375, 0.8047378541243649375, 1.000000000000000000 ) ) 
 REPRESENTATION_ITEM ( '' )  );
#31124 = ORIENTED_EDGE ( 'NONE', *, *, #19694, .F. ) ;
#31125 = EDGE_LOOP ( 'NONE', ( #48244, #20921, #30134, #47113 ) ) ;
#31126 = FACE_OUTER_BOUND ( 'NONE', #14452, .T. ) ;
#31127 = CARTESIAN_POINT ( 'NONE',  ( 0.4426377647354858835, 1.666766018367784596, 9.928159647716132241 ) ) ;
#31128 = VECTOR ( 'NONE', #50620, 1000.000000000000000 ) ;
#31129 = ORIENTED_EDGE ( 'NONE', *, *, #2659, .F. ) ;
#31130 = ORIENTED_EDGE ( 'NONE', *, *, #25699, .F. ) ;
#31131 = CYLINDRICAL_SURFACE ( 'NONE', #19206, 2.000000000000001776 ) ;
#31132 = CARTESIAN_POINT ( 'NONE',  ( 181.0000000000000000, -168.9999999999999432, -340.0000000000001137 ) ) ;
#31133 = CARTESIAN_POINT ( 'NONE',  ( 342.0000000000000568, 167.8284271247462129, 342.8284271247459856 ) ) ;
#31134 = EDGE_LOOP ( 'NONE', ( #44125, #22361, #10381 ) ) ;
#31135 = DIRECTION ( 'NONE',  ( -0.000000000000000000, -1.000000000000000000, -0.000000000000000000 ) ) ;
#31136 = ORIENTED_EDGE ( 'NONE', *, *, #28494, .F. ) ;
#31137 = ADVANCED_FACE ( 'NONE', ( #10332 ), #25984, .T. ) ;
#31138 =( BOUNDED_CURVE ( )  B_SPLINE_CURVE ( 3, ( #4403, #50539, #3890, #28001 ),
 .UNSPECIFIED., .F., .F. ) 
 B_SPLINE_CURVE_WITH_KNOTS ( ( 4, 4 ),
 ( 1.570796326794896558, 3.141592653589793116 ),
 .UNSPECIFIED. ) 
 CURVE ( )  GEOMETRIC_REPRESENTATION_ITEM ( )  RATIONAL_B_SPLINE_CURVE ( ( 1.000000000000000000, 0.8047378541243649375, 0.8047378541243649375, 1.000000000000000000 ) ) 
 REPRESENTATION_ITEM ( '' )  );
#31139 = DIRECTION ( 'NONE',  ( -1.000000000000000000, 0.000000000000000000, 0.000000000000000000 ) ) ;
#31140 = EDGE_CURVE ( 'NONE', #18060, #10849, #6229, .T. ) ;
#31141 = DIRECTION ( 'NONE',  ( -6.765175596986472868E-16, 0.9749645535258953943, 0.2223603367690637489 ) ) ;
#31142 = EDGE_CURVE ( 'NONE', #21789, #7928, #5460, .T. ) ;
#31143 = DIRECTION ( 'NONE',  ( 1.000000000000000000, 0.000000000000000000, 0.000000000000000000 ) ) ;
#31144 = ORIENTED_EDGE ( 'NONE', *, *, #16711, .F. ) ;
#31145 = ORIENTED_EDGE ( 'NONE', *, *, #42484, .T. ) ;
#31146 = ORIENTED_EDGE ( 'NONE', *, *, #2256, .T. ) ;
#31147 = DIRECTION ( 'NONE',  ( -1.000000000000000000, -0.000000000000000000, -0.000000000000000000 ) ) ;
#31148 = CARTESIAN_POINT ( 'NONE',  ( 191.5540265531850537, -1.025126265847089213, 162.5682875569279133 ) ) ;
#31149 = DIRECTION ( 'NONE',  ( -0.000000000000000000, -0.000000000000000000, -1.000000000000000000 ) ) ;
#31150 = ORIENTED_EDGE ( 'NONE', *, *, #19095, .T. ) ;
#31151 = CARTESIAN_POINT ( 'NONE',  ( 0.8282505383454039638, 1.889063466747038289, 9.894754715216722118 ) ) ;
#31152 = EDGE_CURVE ( 'NONE', #44363, #29337, #29067, .T. ) ;
#31153 = ADVANCED_FACE ( 'NONE', ( #2126 ), #49012, .T. ) ;
#31155 = VERTEX_POINT ( 'NONE', #496 ) ;
#31154 = AXIS2_PLACEMENT_3D ( 'NONE', #8902, #48361, #13500 ) ;
#31156 = DIRECTION ( 'NONE',  ( -1.000000000000000000, 0.000000000000000000, 0.000000000000000000 ) ) ;
#31158 = ORIENTED_EDGE ( 'NONE', *, *, #46143, .F. ) ;
#31157 = VECTOR ( 'NONE', #41135, 1000.000000000000000 ) ;
#31159 = ADVANCED_FACE ( 'NONE', ( #24097 ), #244, .F. ) ;
#31160 = CARTESIAN_POINT ( 'NONE',  ( -48.44597344681495343, 0.000000000000000000, 82.56828755692798438 ) ) ;
#31161 = CARTESIAN_POINT ( 'NONE',  ( 0.3370904143228981575, -0.2449105217885261532, 10.00000000000000000 ) ) ;
#31162 = LINE ( 'NONE', #43202, #17675 ) ;
#31163 = VECTOR ( 'NONE', #28831, 1000.000000000000000 ) ;
#31164 = CARTESIAN_POINT ( 'NONE',  ( 8.277096487746778308, -33.14818118907697198, 7.455576670931136185 ) ) ;
#31165 = ORIENTED_EDGE ( 'NONE', *, *, #4981, .F. ) ;
#31166 = ORIENTED_EDGE ( 'NONE', *, *, #8134, .T. ) ;
#31167 = CARTESIAN_POINT ( 'NONE',  ( -1.228394325311288560, 1.341866297401936636, 9.903764339332077782 ) ) ;
#31168 = AXIS2_PLACEMENT_3D ( 'NONE', #35894, #8433, #24086 ) ;
#31169 = CARTESIAN_POINT ( 'NONE',  ( 31.55402655318506788, 2.143131898507880377E-16, -160.9317124430720298 ) ) ;
#31170 = CARTESIAN_POINT ( 'NONE',  ( -206.6959734468149463, 0.000000000000000000, 165.0000000000000000 ) ) ;
#31171 = CARTESIAN_POINT ( 'NONE',  ( -16.73672383626882976, -2.341008440547994063, -9.008049429158100807 ) ) ;
#31172 = VECTOR ( 'NONE', #46213, 1000.000000000000000 ) ;
#31173 = CARTESIAN_POINT ( 'NONE',  ( -16.99749102614300966, 1.320765928724422222, 8.953103998512858652 ) ) ;
#31174 = DIRECTION ( 'NONE',  ( -1.000000000000000000, 0.000000000000000000, -1.612977847700450206E-50 ) ) ;
#31175 = ORIENTED_EDGE ( 'NONE', *, *, #16465, .T. ) ;
#31176 = DIRECTION ( 'NONE',  ( 0.000000000000000000, -0.2223603367690656640, -0.9749645535258950613 ) ) ;
#31177 = EDGE_CURVE ( 'NONE', #31585, #46422, #18253, .T. ) ;
#31178 = CARTESIAN_POINT ( 'NONE',  ( 210.0000000000000568, 0.000000000000000000, -119.1817124430720440 ) ) ;
#31179 = B_SPLINE_CURVE_WITH_KNOTS ( 'NONE', 3,
 ( #44509, #24795, #6035, #37376 ),
 .UNSPECIFIED., .F., .F.,
 ( 4, 4 ),
 ( 0.0004299334430849653297, 0.0007706806524480538500 ),
 .UNSPECIFIED. ) ;
#31180 = ORIENTED_EDGE ( 'NONE', *, *, #1775, .F. ) ;
#31181 = ADVANCED_FACE ( 'NONE', ( #38304 ), #42112, .T. ) ;
#31182 = EDGE_CURVE ( 'NONE', #14966, #23429, #6913, .T. ) ;
#31183 = CARTESIAN_POINT ( 'NONE',  ( 224.9999999999999432, 175.0000000000000000, 0.000000000000000000 ) ) ;
#31184 = LINE ( 'NONE', #19866, #47452 ) ;
#31185 = DIRECTION ( 'NONE',  ( 0.000000000000000000, 1.000000000000000000, 0.000000000000000000 ) ) ;
#31186 = EDGE_CURVE ( 'NONE', #45850, #46718, #3383, .T. ) ;
#31187 = ORIENTED_EDGE ( 'NONE', *, *, #22020, .T. ) ;
#31188 = ORIENTED_EDGE ( 'NONE', *, *, #42484, .F. ) ;
#31189 = LINE ( 'NONE', #43725, #42262 ) ;
#31190 = EDGE_CURVE ( 'NONE', #33167, #28808, #16136, .T. ) ;
#31191 = DIRECTION ( 'NONE',  ( -1.612977847700450206E-50, 0.000000000000000000, -1.000000000000000000 ) ) ;
#31192 = AXIS2_PLACEMENT_3D ( 'NONE', #29469, #21508, #41022 ) ;
#31193 = CIRCLE ( 'NONE', #49150, 2.000000000000001776 ) ;
#31194 = EDGE_LOOP ( 'NONE', ( #9309, #15860, #28749, #22163 ) ) ;
#31195 = ORIENTED_EDGE ( 'NONE', *, *, #16147, .F. ) ;
#31196 = CARTESIAN_POINT ( 'NONE',  ( -2.462075149652696027, 16.57295996686994499, 9.403735324607438884 ) ) ;
#31197 = CARTESIAN_POINT ( 'NONE',  ( 113.3040265531850537, -1.749999999999997113, 40.81828755692798438 ) ) ;
#31198 = ORIENTED_EDGE ( 'NONE', *, *, #7409, .T. ) ;
#31199 = EDGE_LOOP ( 'NONE', ( #29037, #13187, #20686, #35924 ) ) ;
#31200 = VECTOR ( 'NONE', #41315, 1000.000000000000000 ) ;
#31201 = ORIENTED_EDGE ( 'NONE', *, *, #44153, .T. ) ;
#31202 = VECTOR ( 'NONE', #12446, 999.9999999999998863 ) ;
#31203 = CIRCLE ( 'NONE', #33651, 4.000000000000003553 ) ;
#31204 = CARTESIAN_POINT ( 'NONE',  ( 111.5540265531850537, -1.025126265847082108, -37.43171244307203693 ) ) ;
#31205 = CARTESIAN_POINT ( 'NONE',  ( 1.320835335343329753, -0.01943189459118491516, 9.943883492372847854 ) ) ;
#31206 = VERTEX_POINT ( 'NONE', #26737 ) ;
#31207 = CARTESIAN_POINT ( 'NONE',  ( 1.066995270233474624, -50.00000000000000711, -3.760136334089591248 ) ) ;
#31208 = CARTESIAN_POINT ( 'NONE',  ( -164.9999999999981526, 17.00000000000000000, 90.00000000000000000 ) ) ;
#31209 = CARTESIAN_POINT ( 'NONE',  ( -215.0000000000000568, -175.0000000000000000, 500.0000000000000000 ) ) ;
#31210 = VERTEX_POINT ( 'NONE', #18761 ) ;
#31211 = ORIENTED_EDGE ( 'NONE', *, *, #22080, .F. ) ;
#31212 = CARTESIAN_POINT ( 'NONE',  ( 35.05402655318504657, 1.025126265847089657, -37.43171244307202272 ) ) ;
#31213 = CARTESIAN_POINT ( 'NONE',  ( -15.00000000000000000, -46.01315789473684248, 6.315789473684215949 ) ) ;
#31214 = UNCERTAINTY_MEASURE_WITH_UNIT (LENGTH_MEASURE( 1.000000000000000082E-05 ), #46703, 'distance_accuracy_value', 'NONE');
#31215 = ORIENTED_EDGE ( 'NONE', *, *, #37764, .T. ) ;
#31216 = EDGE_CURVE ( 'NONE', #11317, #22983, #47134, .T. ) ;
#31217 = EDGE_CURVE ( 'NONE', #7144, #45646, #42976, .T. ) ;
#31218 = ORIENTED_EDGE ( 'NONE', *, *, #44670, .T. ) ;
#31219 = CARTESIAN_POINT ( 'NONE',  ( 32.43949840348898306, 7.871562655726499713, -9.367992836599954742 ) ) ;
#31220 = CARTESIAN_POINT ( 'NONE',  ( -124.9459734468149463, 2.143131898507847836E-16, 79.06828755692798438 ) ) ;
#31221 = ORIENTED_EDGE ( 'NONE', *, *, #11097, .T. ) ;
#31222 = ADVANCED_FACE ( 'NONE', ( #23839, #39749 ), #34442, .T. ) ;
#31223 = DIRECTION ( 'NONE',  ( 0.000000000000000000, 0.000000000000000000, 1.000000000000000000 ) ) ;
#31224 = CARTESIAN_POINT ( 'NONE',  ( -48.44597344681495343, 0.000000000000000000, -0.9317124430720247208 ) ) ;
#31225 = LINE ( 'NONE', #175, #44951 ) ;
#31226 = EDGE_CURVE ( 'NONE', #29259, #46163, #7231, .T. ) ;
#31227 = LINE ( 'NONE', #35090, #12608 ) ;
#31228 = EDGE_LOOP ( 'NONE', ( #45102, #5457, #12707, #38184 ) ) ;
#31229 = EDGE_CURVE ( 'NONE', #22165, #13210, #50193, .T. ) ;
#31230 = DIRECTION ( 'NONE',  ( 1.000000000000000000, 0.000000000000000000, 0.000000000000000000 ) ) ;
#31231 = ADVANCED_FACE ( 'NONE', ( #19974 ), #31799, .T. ) ;
#31232 = DIRECTION ( 'NONE',  ( -0.000000000000000000, -0.000000000000000000, 1.000000000000000000 ) ) ;
#31233 = DIRECTION ( 'NONE',  ( -1.586032892321652236E-16, -1.000000000000000000, -2.288264760618012091E-48 ) ) ;
#31234 = VECTOR ( 'NONE', #33717, 1000.000000000000000 ) ;
#31235 = CARTESIAN_POINT ( 'NONE',  ( -88.44597344681497475, 0.000000000000000000, -77.43171244307198720 ) ) ;
#31236 = AXIS2_PLACEMENT_3D ( 'NONE', #36053, #34850, #23266 ) ;
#31237 = ORIENTED_EDGE ( 'NONE', *, *, #29341, .T. ) ;
#31238 = CARTESIAN_POINT ( 'NONE',  ( -225.0000000000000568, 164.9999999999999716, 252.0000000000000000 ) ) ;
#31239 = VECTOR ( 'NONE', #22203, 1000.000000000000000 ) ;
#31240 = CARTESIAN_POINT ( 'NONE',  ( -0.9989200098981521059, -1.123829893718962802, 9.927319414211225990 ) ) ;
#31241 = EDGE_LOOP ( 'NONE', ( #39556, #25122, #6112, #12546 ) ) ;
#31242 = CARTESIAN_POINT ( 'NONE',  ( -164.9459734468149463, 2.143131898507880377E-16, 165.0000000000000000 ) ) ;
#31243 = ADVANCED_FACE ( 'NONE', ( #30086 ), #12276, .T. ) ;
#31244 = EDGE_CURVE ( 'NONE', #36272, #953, #30584, .T. ) ;
#31245 = CARTESIAN_POINT ( 'NONE',  ( -166.6959734468149463, 1.750000000000010658, 120.8182875569279702 ) ) ;
#31246 = ORIENTED_EDGE ( 'NONE', *, *, #6824, .T. ) ;
#31247 = CARTESIAN_POINT ( 'NONE',  ( 0.000000000000000000, 13.98684210526316107, 0.000000000000000000 ) ) ;
#31248 = LINE ( 'NONE', #46838, #29449 ) ;
#31249 = PLANE ( 'NONE',  #10903 ) ;
#31250 = CARTESIAN_POINT ( 'NONE',  ( 0.000000000000000000, 0.000000000000000000, 910.0000000000000000 ) ) ;
#31251 = VERTEX_POINT ( 'NONE', #10821 ) ;
#31252 = CARTESIAN_POINT ( 'NONE',  ( 0.7479701569602201783, 0.9668092547198030573, 9.969517326151114744 ) ) ;
#31253 = ORIENTED_EDGE ( 'NONE', *, *, #10622, .F. ) ;
#31254 = VERTEX_POINT ( 'NONE', #38553 ) ;
#31255 = DIRECTION ( 'NONE',  ( 0.000000000000000000, -1.000000000000000000, -1.544785076050074834E-48 ) ) ;
#31256 = CARTESIAN_POINT ( 'NONE',  ( 350.0000000000001137, 183.0000000000000284, 343.9999999999997726 ) ) ;
#31257 = VERTEX_POINT ( 'NONE', #34698 ) ;
#31258 = CARTESIAN_POINT ( 'NONE',  ( -124.9459734468149463, 2.143131898507847836E-16, 122.5682875569279560 ) ) ;
#31259 = CARTESIAN_POINT ( 'NONE',  ( -128.4459734468149463, 1.025126265847081442, 162.5682875569279133 ) ) ;
#31260 = ADVANCED_FACE ( 'NONE', ( #9436 ), #25101, .F. ) ;
#31261 = VECTOR ( 'NONE', #18956, 1000.000000000000000 ) ;
#31262 = LINE ( 'NONE', #46853, #12855 ) ;
#31263 = ORIENTED_EDGE ( 'NONE', *, *, #6529, .F. ) ;
#31264 = AXIS2_PLACEMENT_3D ( 'NONE', #44063, #32043, #15875 ) ;
#31265 = DIRECTION ( 'NONE',  ( -1.000000000000000000, 0.000000000000000000, 0.000000000000000000 ) ) ;
#31266 = PLANE ( 'NONE',  #23444 ) ;
#31267 = LINE ( 'NONE', #26891, #38180 ) ;
#31268 = ORIENTED_EDGE ( 'NONE', *, *, #43538, .T. ) ;
#31269 = DIRECTION ( 'NONE',  ( -7.793956916774524585E-48, 0.000000000000000000, -1.000000000000000000 ) ) ;
#31270 = CARTESIAN_POINT ( 'NONE',  ( -214.9999999999999432, 173.0000000000000000, 231.9999999999999716 ) ) ;
#31271 = ORIENTED_EDGE ( 'NONE', *, *, #34700, .F. ) ;
#31272 = EDGE_CURVE ( 'NONE', #16751, #45714, #20994, .T. ) ;
#31273 = ORIENTED_EDGE ( 'NONE', *, *, #35548, .F. ) ;
#31274 = VERTEX_POINT ( 'NONE', #9183 ) ;
#31275 = CARTESIAN_POINT ( 'NONE',  ( -31.84561714023301349, 33.32763979208128546, 8.807470649214879543 ) ) ;
#31276 = AXIS2_PLACEMENT_3D ( 'NONE', #38178, #34311, #38936 ) ;
#31277 = DIRECTION ( 'NONE',  ( 0.000000000000000000, -0.4436251537532894806, -0.8962124318248270161 ) ) ;
#31278 = VECTOR ( 'NONE', #32684, 1000.000000000000000 ) ;
#31279 = VERTEX_POINT ( 'NONE', #13025 ) ;
#31280 = B_SPLINE_CURVE_WITH_KNOTS ( 'NONE', 3,
 ( #46060, #2495, #29692, #45313 ),
 .UNSPECIFIED., .F., .F.,
 ( 4, 4 ),
 ( 0.9895749839358300992, 1.000000000000000000 ),
 .UNSPECIFIED. ) ;
#31281 = CARTESIAN_POINT ( 'NONE',  ( -165.6708471809677974, -1.750000000000009548, -78.15658617722490931 ) ) ;
#31282 = DIRECTION ( 'NONE',  ( 0.000000000000000000, 1.000000000000000000, 0.000000000000000000 ) ) ;
#31283 = DIRECTION ( 'NONE',  ( 0.000000000000000000, 0.000000000000000000, 1.000000000000000000 ) ) ;
#31284 =( BOUNDED_CURVE ( )  B_SPLINE_CURVE ( 3, ( #49270, #6716, #25727, #49768 ),
 .UNSPECIFIED., .F., .F. ) 
 B_SPLINE_CURVE_WITH_KNOTS ( ( 4, 4 ),
 ( 0.000000000000000000, 1.570796326794896558 ),
 .UNSPECIFIED. ) 
 CURVE ( )  GEOMETRIC_REPRESENTATION_ITEM ( )  RATIONAL_B_SPLINE_CURVE ( ( 1.000000000000000000, 0.8047378541243649375, 0.8047378541243649375, 1.000000000000000000 ) ) 
 REPRESENTATION_ITEM ( '' )  );
#31285 = EDGE_CURVE ( 'NONE', #32625, #35472, #8701, .T. ) ;
#31286 = CARTESIAN_POINT ( 'NONE',  ( 31.55402655318503236, 0.000000000000000000, -80.93171244307204404 ) ) ;
#31287 = LINE ( 'NONE', #16627, #17333 ) ;
#31288 = EDGE_CURVE ( 'NONE', #10041, #44104, #12147, .T. ) ;
#31289 = DIRECTION ( 'NONE',  ( -0.000000000000000000, -0.000000000000000000, -1.000000000000000000 ) ) ;
#31290 = DIRECTION ( 'NONE',  ( -1.000000000000000000, 0.000000000000000000, 0.000000000000000000 ) ) ;
#31291 =( BOUNDED_CURVE ( )  B_SPLINE_CURVE ( 3, ( #23308, #11771, #42797, #50464 ),
 .UNSPECIFIED., .F., .F. ) 
 B_SPLINE_CURVE_WITH_KNOTS ( ( 4, 4 ),
 ( 3.141592653589793116, 4.712388980384689674 ),
 .UNSPECIFIED. ) 
 CURVE ( )  GEOMETRIC_REPRESENTATION_ITEM ( )  RATIONAL_B_SPLINE_CURVE ( ( 1.000000000000000000, 0.8047378541243649375, 0.8047378541243649375, 1.000000000000000000 ) ) 
 REPRESENTATION_ITEM ( '' )  );
#31292 = EDGE_CURVE ( 'NONE', #27788, #12513, #8657, .T. ) ;
#31293 = CARTESIAN_POINT ( 'NONE',  ( 169.0000000000000000, -180.9999999999999716, -115.0000000000001279 ) ) ;
#31294 = ORIENTED_EDGE ( 'NONE', *, *, #6429, .T. ) ;
#31295 = EDGE_CURVE ( 'NONE', #48700, #15604, #35905, .T. ) ;
#31296 = EDGE_CURVE ( 'NONE', #32935, #27742, #40025, .T. ) ;
#31297 = DIRECTION ( 'NONE',  ( 0.000000000000000000, 0.000000000000000000, 1.000000000000000000 ) ) ;
#31298 = DIRECTION ( 'NONE',  ( -1.000000000000000000, -0.000000000000000000, -0.000000000000000000 ) ) ;
#31299 = DIRECTION ( 'NONE',  ( 1.000000000000000000, 0.000000000000000000, -0.000000000000000000 ) ) ;
#31300 = CARTESIAN_POINT ( 'NONE',  ( 9.970345420962653193, -0.8985218257325291447, 2.778652340038831436 ) ) ;
#31301 = ORIENTED_EDGE ( 'NONE', *, *, #47216, .T. ) ;
#31302 = CARTESIAN_POINT ( 'NONE',  ( 0.000000000000000000, 0.000000000000000000, -10.00000000000000000 ) ) ;
#31303 = AXIS2_PLACEMENT_3D ( 'NONE', #35971, #16457, #32108 ) ;
#31304 = ADVANCED_FACE ( 'NONE', ( #48138 ), #17141, .F. ) ;
#31305 = CARTESIAN_POINT ( 'NONE',  ( 0.000000000000000000, 185.0000000000000284, 343.9999999999997726 ) ) ;
#31306 = LINE ( 'NONE', #31559, #47114 ) ;
#31307 = CARTESIAN_POINT ( 'NONE',  ( 44.99506233596247995, 23.32283626942318833, 7.455576670931136185 ) ) ;
#31308 = ORIENTED_EDGE ( 'NONE', *, *, #40671, .F. ) ;
#31309 = DIRECTION ( 'NONE',  ( 1.000000000000000000, 0.000000000000000000, 0.000000000000000000 ) ) ;
#31310 = ORIENTED_EDGE ( 'NONE', *, *, #24201, .F. ) ;
#31311 = AXIS2_PLACEMENT_3D ( 'NONE', #29329, #37553, #21365 ) ;
#31312 = PLANE ( 'NONE',  #8989 ) ;
#31313 = VERTEX_POINT ( 'NONE', #40243 ) ;
#31314 = CARTESIAN_POINT ( 'NONE',  ( 153.3040265531850537, -1.750000000000010214, 40.81828755692798438 ) ) ;
#31315 = LINE ( 'NONE', #11802, #6804 ) ;
#31316 = ORIENTED_EDGE ( 'NONE', *, *, #43479, .F. ) ;
#31317 = CARTESIAN_POINT ( 'NONE',  ( -19.99999999999940670, 16.00000000000000000, -54.99999999999999289 ) ) ;
#31318 = ORIENTED_EDGE ( 'NONE', *, *, #24892, .F. ) ;
#31319 = EDGE_LOOP ( 'NONE', ( #24971, #19590, #1585 ) ) ;
#31320 = CARTESIAN_POINT ( 'NONE',  ( -85.67084718096784002, 1.750000000000009548, -38.15658617722494483 ) ) ;
#31321 = CARTESIAN_POINT ( 'NONE',  ( -204.9459734468148895, 1.025126265847089435, 39.06828755692797728 ) ) ;
#31322 = ORIENTED_EDGE ( 'NONE', *, *, #41650, .F. ) ;
#31323 = CARTESIAN_POINT ( 'NONE',  ( 0.8813691545818379547, 1.919529038513666297, 9.884520277910691988 ) ) ;
#31324 = CARTESIAN_POINT ( 'NONE',  ( -64.99999999999971578, 17.00000000000000000, -84.99999999999998579 ) ) ;
#31325 = DIRECTION ( 'NONE',  ( -0.000000000000000000, -0.000000000000000000, 1.000000000000000000 ) ) ;
#31326 = ORIENTED_EDGE ( 'NONE', *, *, #50337, .F. ) ;
#31327 = DIRECTION ( 'NONE',  ( 4.758098676964956461E-16, 0.000000000000000000, 1.000000000000000000 ) ) ;
#31328 = ADVANCED_FACE ( 'NONE', ( #13275 ), #20476, .F. ) ;
#31329 = DIRECTION ( 'NONE',  ( 1.000000000000000000, 0.000000000000000000, 0.000000000000000000 ) ) ;
#31330 = ORIENTED_EDGE ( 'NONE', *, *, #26469, .F. ) ;
#31331 = CARTESIAN_POINT ( 'NONE',  ( 6.174150299305392053, -50.00000000000000711, 8.807470649214879543 ) ) ;
#31332 = LINE ( 'NONE', #27973, #2393 ) ;
#31333 =( GEOMETRIC_REPRESENTATION_CONTEXT ( 3 ) GLOBAL_UNCERTAINTY_ASSIGNED_CONTEXT ( ( #5073 ) ) GLOBAL_UNIT_ASSIGNED_CONTEXT ( ( #4266, #16316, #42994 ) ) REPRESENTATION_CONTEXT ( 'NONE', 'WORKASPACE' ) );
#31334 = ORIENTED_EDGE ( 'NONE', *, *, #4189, .F. ) ;
#31335 = CARTESIAN_POINT ( 'NONE',  ( 210.0000000000000568, 0.000000000000000000, -39.18171244307202983 ) ) ;
#31336 = AXIS2_PLACEMENT_3D ( 'NONE', #33866, #7161, #3041 ) ;
#31337 = LINE ( 'NONE', #46927, #43138 ) ;
#31338 = ORIENTED_EDGE ( 'NONE', *, *, #28164, .F. ) ;
#31339 = LINE ( 'NONE', #47682, #44758 ) ;
#31340 = DIRECTION ( 'NONE',  ( 0.000000000000000000, -2.265761274745217480E-16, 1.000000000000000000 ) ) ;
#31341 = CARTESIAN_POINT ( 'NONE',  ( 155.0540265531850537, -1.025126265847089435, -117.4317124430720156 ) ) ;
#31342 = CARTESIAN_POINT ( 'NONE',  ( -4.945973446814903696, 2.143131898507912917E-16, 39.06828755692792754 ) ) ;
#31343 = EDGE_CURVE ( 'NONE', #17183, #17041, #36153, .T. ) ;
#31344 = ADVANCED_FACE ( 'NONE', ( #40749 ), #15841, .T. ) ;
#31345 = VECTOR ( 'NONE', #24386, 1000.000000000000000 ) ;
#31346 = ORIENTED_EDGE ( 'NONE', *, *, #12723, .T. ) ;
#31347 = CARTESIAN_POINT ( 'NONE',  ( 46.76852358249013975, -17.86468378716709537, -9.367992836599954742 ) ) ;
#31348 = CARTESIAN_POINT ( 'NONE',  ( 14.76429217231961566, 8.192625680377691566, 9.178419661560148768 ) ) ;
#31349 = CARTESIAN_POINT ( 'NONE',  ( -13.59579750444763668, 10.60877755095910935, 8.727788335465566760 ) ) ;
#31350 = ORIENTED_EDGE ( 'NONE', *, *, #15466, .F. ) ;
#31351 = VERTEX_POINT ( 'NONE', #24354 ) ;
#31352 = EDGE_CURVE ( 'NONE', #19994, #21654, #28448, .T. ) ;
#31353 = EDGE_CURVE ( 'NONE', #8610, #24878, #12783, .T. ) ;
#31354 = CARTESIAN_POINT ( 'NONE',  ( -225.0000000000000568, -175.0000000000000000, 0.000000000000000000 ) ) ;
#31355 = DIRECTION ( 'NONE',  ( 0.000000000000000000, 0.000000000000000000, -1.000000000000000000 ) ) ;
#31356 = DIRECTION ( 'NONE',  ( 0.000000000000000000, 0.000000000000000000, -1.000000000000000000 ) ) ;
#31357 = DIRECTION ( 'NONE',  ( -0.000000000000000000, -0.000000000000000000, -1.000000000000000000 ) ) ;
#31358 = CARTESIAN_POINT ( 'NONE',  ( 181.0000000000000000, -93.49999999999997158, -115.0000000000001563 ) ) ;
#31359 = ORIENTED_EDGE ( 'NONE', *, *, #28142, .T. ) ;
#31360 = ADVANCED_FACE ( 'NONE', ( #14542 ), #41746, .T. ) ;
#31361 = VECTOR ( 'NONE', #9718, 1000.000000000000000 ) ;
#31362 = CARTESIAN_POINT ( 'NONE',  ( 0.000000000000000000, -184.7999999999999545, -359.8000000000002387 ) ) ;
#31363 = CARTESIAN_POINT ( 'NONE',  ( -166.6959734468149463, 0.000000000000000000, -165.0000000000000000 ) ) ;
#31364 =( NAMED_UNIT ( * ) PLANE_ANGLE_UNIT ( ) SI_UNIT ( $, .RADIAN. ) );
#31365 = ORIENTED_EDGE ( 'NONE', *, *, #9099, .T. ) ;
#31366 = DIRECTION ( 'NONE',  ( -0.000000000000000000, -0.000000000000000000, -1.000000000000000000 ) ) ;
#31367 = ORIENTED_EDGE ( 'NONE', *, *, #12510, .T. ) ;
#31368 = DIRECTION ( 'NONE',  ( 0.000000000000000000, 0.000000000000000000, 1.000000000000000000 ) ) ;
#31369 = SHAPE_REPRESENTATION ( 'aluminum', ( #45486 ), #12706 ) ;
#31370 = CARTESIAN_POINT ( 'NONE',  ( 339.9999999999998863, 174.9999999999996305, -356.0000000000003411 ) ) ;
#31371 = EDGE_LOOP ( 'NONE', ( #23740, #21364, #40021, #14997 ) ) ;
#31372 = DIRECTION ( 'NONE',  ( 0.000000000000000000, -1.000000000000000000, 0.000000000000000000 ) ) ;
#31373 = AXIS2_PLACEMENT_3D ( 'NONE', #3939, #15740, #17006 ) ;
#31374 = CARTESIAN_POINT ( 'NONE',  ( -1.228394325311288560, 1.341866297401936636, 9.903764339332077782 ) ) ;
#31375 = SURFACE_STYLE_USAGE ( .BOTH. , #2937 ) ;
#31376 = CYLINDRICAL_SURFACE ( 'NONE', #14031, 1.750000000000015543 ) ;
#31377 = EDGE_LOOP ( 'NONE', ( #15061, #21278, #35258, #21338 ) ) ;
#31378 = AXIS2_PLACEMENT_3D ( 'NONE', #3835, #46896, #20494 ) ;
#31379 = CARTESIAN_POINT ( 'NONE',  ( -166.6959734468149463, -1.750000000000010658, -79.18171244307201562 ) ) ;
#31380 = VECTOR ( 'NONE', #35969, 1000.000000000000000 ) ;
#31381 = CARTESIAN_POINT ( 'NONE',  ( 339.9999999999998863, -182.9999999999999716, 355.9999999999997726 ) ) ;
#31382 = ORIENTED_EDGE ( 'NONE', *, *, #41987, .F. ) ;
#31383 = CARTESIAN_POINT ( 'NONE',  ( -207.7210997126620384, 1.750000000000009548, -38.15658617722494483 ) ) ;
#31384 = CARTESIAN_POINT ( 'NONE',  ( 2.943113318327519767, 2.672530871845234302, 3.247139928068174530 ) ) ;
#31385 = CARTESIAN_POINT ( 'NONE',  ( 153.3040265531850537, -1.750000000000010658, -79.18171244307201562 ) ) ;
#31386 = FACE_BOUND ( 'NONE', #22590, .T. ) ;
#31387 = ORIENTED_EDGE ( 'NONE', *, *, #36278, .T. ) ;
#31388 = ORIENTED_EDGE ( 'NONE', *, *, #18036, .F. ) ;
#31389 = DIRECTION ( 'NONE',  ( 1.000000000000000000, 0.000000000000000000, 0.000000000000000000 ) ) ;
#31390 = ADVANCED_FACE ( 'NONE', ( #9941, #49401 ), #14800, .T. ) ;
#31391 = EDGE_LOOP ( 'NONE', ( #28973, #43900, #44152, #18250 ) ) ;
#31392 = CARTESIAN_POINT ( 'NONE',  ( 36.32827987961125871, -9.445964435368829015, 3.209567239418972928 ) ) ;
#31393 = CARTESIAN_POINT ( 'NONE',  ( -207.7210997126620384, -1.750000000000010214, -120.2068387089191219 ) ) ;
#31394 = VECTOR ( 'NONE', #47579, 1000.000000000000000 ) ;
#31395 = DIRECTION ( 'NONE',  ( -1.000000000000000000, -0.000000000000000000, -0.000000000000000000 ) ) ;
#31396 = ORIENTED_EDGE ( 'NONE', *, *, #19813, .F. ) ;
#31397 = DIRECTION ( 'NONE',  ( 0.000000000000000000, 0.000000000000000000, -1.000000000000000000 ) ) ;
#31398 = ORIENTED_EDGE ( 'NONE', *, *, #13313, .T. ) ;
#31399 = DIRECTION ( 'NONE',  ( 0.000000000000000000, -1.000000000000000000, 0.000000000000000000 ) ) ;
#31400 = PLANE ( 'NONE',  #23474 ) ;
#31401 = CARTESIAN_POINT ( 'NONE',  ( -14.99999999999782041, 17.00000000000000000, 115.0000000000000142 ) ) ;
#31402 = ORIENTED_EDGE ( 'NONE', *, *, #40882, .F. ) ;
#31403 = ORIENTED_EDGE ( 'NONE', *, *, #11626, .F. ) ;
#31404 = VECTOR ( 'NONE', #36168, 1000.000000000000000 ) ;
#31405 = ORIENTED_EDGE ( 'NONE', *, *, #4837, .F. ) ;
#31406 = CARTESIAN_POINT ( 'NONE',  ( 5.551115123125782702E-14, -180.9999999999999716, 359.9999999999997726 ) ) ;
#31407 = CARTESIAN_POINT ( 'NONE',  ( 192.2789002873380184, -1.750000000000009548, 161.8434138227750907 ) ) ;
#31408 = VECTOR ( 'NONE', #8444, 1000.000000000000000 ) ;
#31409 = CARTESIAN_POINT ( 'NONE',  ( 33.30402655318503946, 0.000000000000000000, 165.0000000000000000 ) ) ;
#31410 = ORIENTED_EDGE ( 'NONE', *, *, #43768, .F. ) ;
#31411 = CARTESIAN_POINT ( 'NONE',  ( 193.3040265531851105, 0.000000000000000000, -165.0000000000000000 ) ) ;
#31412 = ORIENTED_EDGE ( 'NONE', *, *, #11084, .F. ) ;
#31413 = LINE ( 'NONE', #28814, #5346 ) ;
#31414 = EDGE_LOOP ( 'NONE', ( #46209, #9167, #34224, #15482, #39379, #17314, #21205, #34670 ) ) ;
#31415 = CARTESIAN_POINT ( 'NONE',  ( 360.0000000000000000, 181.0000000000000284, -356.0000000000001705 ) ) ;
#31416 = CARTESIAN_POINT ( 'NONE',  ( 22.69295089195473736, 45.31600496604706052, 7.455576670931136185 ) ) ;
#31417 = LINE ( 'NONE', #23958, #25050 ) ;
#31418 = CIRCLE ( 'NONE', #22380, 4.000000000000003553 ) ;
#31419 = CARTESIAN_POINT ( 'NONE',  ( 356.0000000000000000, -167.0000000000001137, 341.9999999999999432 ) ) ;
#31420 = CARTESIAN_POINT ( 'NONE',  ( -27.25836557470613286, 25.76317754842369112, 8.100132398494515940 ) ) ;
#31421 = ORIENTED_EDGE ( 'NONE', *, *, #39084, .F. ) ;
#31422 = VERTEX_POINT ( 'NONE', #34308 ) ;
#31423 = EDGE_CURVE ( 'NONE', #16247, #41332, #25599, .T. ) ;
#31424 = CARTESIAN_POINT ( 'NONE',  ( 181.0000000000000284, -174.9999999999999716, -113.0000000000001563 ) ) ;
#31425 = B_SPLINE_SURFACE_WITH_KNOTS ( 'NONE', 3, 3, ( 
 ( #34642, #3062, #11284, #45639 ),
 ( #14877, #30526, #15125, #18460 ),
 ( #34148, #42566, #49721, #7180 ),
 ( #30275, #45884, #10762, #38742 ) ),
 .UNSPECIFIED., .F., .F., .F.,
 ( 4, 4 ),
 ( 4, 4 ),
 ( 0.000000000000000000, 1.000000000000000000 ),
 ( 0.000000000000000000, 1.000000000000000000 ),
 .UNSPECIFIED. ) ;
#31426 = CARTESIAN_POINT ( 'NONE',  ( -164.9999999999987779, 17.00000000000000000, 5.000000000000004441 ) ) ;
#31427 = CARTESIAN_POINT ( 'NONE',  ( -0.2778388845795317086, 1.251314014313103851, 9.976582533991678048 ) ) ;
#31428 =( BOUNDED_CURVE ( )  B_SPLINE_CURVE ( 3, ( #29608, #5306, #705, #27914 ),
 .UNSPECIFIED., .F., .F. ) 
 B_SPLINE_CURVE_WITH_KNOTS ( ( 4, 4 ),
 ( 1.570796326794896558, 3.141592653589793116 ),
 .UNSPECIFIED. ) 
 CURVE ( )  GEOMETRIC_REPRESENTATION_ITEM ( )  RATIONAL_B_SPLINE_CURVE ( ( 1.000000000000000000, 0.8047378541243649375, 0.8047378541243649375, 1.000000000000000000 ) ) 
 REPRESENTATION_ITEM ( '' )  );
#31429 = DIRECTION ( 'NONE',  ( -8.673617379884028076E-17, 1.000000000000000000, -0.000000000000000000 ) ) ;
#31430 = CARTESIAN_POINT ( 'NONE',  ( -0.3862712429686895876, 1.188820645368940720, 10.00000000000000000 ) ) ;
#31431 = ORIENTED_EDGE ( 'NONE', *, *, #48136, .F. ) ;
#31432 = DIRECTION ( 'NONE',  ( -1.000000000000000000, -0.000000000000000000, -0.000000000000000000 ) ) ;
#31433 =( BOUNDED_CURVE ( )  B_SPLINE_CURVE ( 3, ( #24671, #8263, #1327, #12859 ),
 .UNSPECIFIED., .F., .F. ) 
 B_SPLINE_CURVE_WITH_KNOTS ( ( 4, 4 ),
 ( 4.712388980384689674, 6.283185307179586232 ),
 .UNSPECIFIED. ) 
 CURVE ( )  GEOMETRIC_REPRESENTATION_ITEM ( )  RATIONAL_B_SPLINE_CURVE ( ( 1.000000000000000000, 0.8047378541243649375, 0.8047378541243649375, 1.000000000000000000 ) ) 
 REPRESENTATION_ITEM ( '' )  );
#31434 = VERTEX_POINT ( 'NONE', #5844 ) ;
#31435 = CARTESIAN_POINT ( 'NONE',  ( -543.5050241616419271, 54.43801056904003133, -176.2397770772458898 ) ) ;
#31436 = VECTOR ( 'NONE', #7461, 1000.000000000000000 ) ;
#31437 = DIRECTION ( 'NONE',  ( -1.586032892321652236E-16, -1.000000000000000000, -6.853681917100419162E-49 ) ) ;
#31438 = CARTESIAN_POINT ( 'NONE',  ( 3.975459390375365665, 0.2195152216756870167, 1.992221491942114397E-15 ) ) ;
#31439 = VECTOR ( 'NONE', #6407, 1000.000000000000000 ) ;
#31440 =( BOUNDED_CURVE ( )  B_SPLINE_CURVE ( 3, ( #35782, #361, #36021, #31671 ),
 .UNSPECIFIED., .F., .F. ) 
 B_SPLINE_CURVE_WITH_KNOTS ( ( 4, 4 ),
 ( 3.141592653589793116, 4.712388980384689674 ),
 .UNSPECIFIED. ) 
 CURVE ( )  GEOMETRIC_REPRESENTATION_ITEM ( )  RATIONAL_B_SPLINE_CURVE ( ( 1.000000000000000000, 0.8047378541243649375, 0.8047378541243649375, 1.000000000000000000 ) ) 
 REPRESENTATION_ITEM ( '' )  );
#31441 = ORIENTED_EDGE ( 'NONE', *, *, #39696, .T. ) ;
#31442 = ORIENTED_EDGE ( 'NONE', *, *, #4192, .F. ) ;
#31443 = FACE_OUTER_BOUND ( 'NONE', #25531, .T. ) ;
#31444 = CYLINDRICAL_SURFACE ( 'NONE', #17297, 1.750000000000015543 ) ;
#31445 = VERTEX_POINT ( 'NONE', #38177 ) ;
#31446 = EDGE_LOOP ( 'NONE', ( #38203, #12932, #42216, #33633, #30963 ) ) ;
#31447 = CARTESIAN_POINT ( 'NONE',  ( 210.0000000000000568, 0.000000000000000000, 42.56828755692799149 ) ) ;
#31448 = FACE_OUTER_BOUND ( 'NONE', #48192, .T. ) ;
#31449 = CARTESIAN_POINT ( 'NONE',  ( 181.0000000000000000, -5.999999999999950262, 339.9999999999998295 ) ) ;
#31450 = CARTESIAN_POINT ( 'NONE',  ( 71.55402655318505367, 0.000000000000000000, 165.0000000000000000 ) ) ;
#31451 = ORIENTED_EDGE ( 'NONE', *, *, #48672, .F. ) ;
#31452 = EDGE_LOOP ( 'NONE', ( #36195, #36000, #5518, #42908, #14969, #49632 ) ) ;
#31453 = ORIENTED_EDGE ( 'NONE', *, *, #39328, .F. ) ;
#31454 = CARTESIAN_POINT ( 'NONE',  ( -17.23491422248386584, 0.5912720620001978844, 8.727788335465566760 ) ) ;
#31455 = EDGE_LOOP ( 'NONE', ( #19872, #49894, #41712, #25481 ) ) ;
#31456 = AXIS2_PLACEMENT_3D ( 'NONE', #22674, #35262, #14982 ) ;
#31457 = CARTESIAN_POINT ( 'NONE',  ( -1.250000000000000222, 0.000000000000000000, 10.00000000000000000 ) ) ;
#31458 = FACE_OUTER_BOUND ( 'NONE', #30300, .T. ) ;
#31459 = FACE_OUTER_BOUND ( 'NONE', #23804, .T. ) ;
#31460 = ORIENTED_EDGE ( 'NONE', *, *, #45266, .F. ) ;
#31461 = ORIENTED_EDGE ( 'NONE', *, *, #37839, .T. ) ;
#31462 = LINE ( 'NONE', #27099, #33 ) ;
#31463 = CARTESIAN_POINT ( 'NONE',  ( 232.4999999999999716, -169.9999999999999716, 444.9999999999998295 ) ) ;
#31464 = FACE_OUTER_BOUND ( 'NONE', #5736, .T. ) ;
#31465 = ORIENTED_EDGE ( 'NONE', *, *, #19941, .F. ) ;
#31466 = ORIENTED_EDGE ( 'NONE', *, *, #5545, .F. ) ;
#31467 = B_SPLINE_CURVE_WITH_KNOTS ( 'NONE', 3,
 ( #9454, #8959, #40516, #25118 ),
 .UNSPECIFIED., .F., .F.,
 ( 4, 4 ),
 ( 0.001937412222931636377, 0.003978261222106059536 ),
 .UNSPECIFIED. ) ;
#31468 = DIRECTION ( 'NONE',  ( 0.000000000000000000, 0.000000000000000000, -1.000000000000000000 ) ) ;
#31469 = CARTESIAN_POINT ( 'NONE',  ( -239.0000000000000853, -153.6999999999999602, 250.3600000000000136 ) ) ;
#31470 = VERTEX_POINT ( 'NONE', #29954 ) ;
#31471 = CARTESIAN_POINT ( 'NONE',  ( -85.67084718096784002, -1.750000000000009548, 121.8434138227750623 ) ) ;
#31472 = DIRECTION ( 'NONE',  ( 0.000000000000000000, -0.000000000000000000, -1.000000000000000000 ) ) ;
#31473 = DIRECTION ( 'NONE',  ( 0.000000000000000000, 0.000000000000000000, -1.000000000000000000 ) ) ;
#31474 = EDGE_CURVE ( 'NONE', #14709, #16946, #17186, .T. ) ;
#31475 = AXIS2_PLACEMENT_3D ( 'NONE', #46664, #11563, #7717 ) ;
#31476 = VECTOR ( 'NONE', #47100, 1000.000000000000000 ) ;
#31477 = LINE ( 'NONE', #35848, #6059 ) ;
#31478 = VERTEX_POINT ( 'NONE', #40993 ) ;
#31479 = ADVANCED_FACE ( 'NONE', ( #37421 ), #17880, .F. ) ;
#31480 = AXIS2_PLACEMENT_3D ( 'NONE', #15628, #19980, #31299 ) ;
#31481 = CARTESIAN_POINT ( 'NONE',  ( -8.176860274785726190, 5.756644512789648616, 9.282506307616472441 ) ) ;
#31482 = CARTESIAN_POINT ( 'NONE',  ( 210.0000000000000568, 0.000000000000000000, -117.4317124430720298 ) ) ;
#31483 = DIRECTION ( 'NONE',  ( -0.4055129968046615185, -0.4055129968046615185, -0.8192181753629524943 ) ) ;
#31484 = CIRCLE ( 'NONE', #38038, 0.5000000000000004441 ) ;
#31485 = EDGE_CURVE ( 'NONE', #44630, #44983, #47757, .T. ) ;
#31486 = PLANE ( 'NONE',  #27164 ) ;
#31487 = ADVANCED_FACE ( 'NONE', ( #6347 ), #21483, .F. ) ;
#31488 = EDGE_LOOP ( 'NONE', ( #5223, #35722, #31072, #21029, #31158, #27870 ) ) ;
#31489 = CARTESIAN_POINT ( 'NONE',  ( 358.0000000000000000, 175.0000000000000284, -106.0000000000001990 ) ) ;
#31490 = EDGE_CURVE ( 'NONE', #23447, #38145, #19118, .T. ) ;
#31491 = DIRECTION ( 'NONE',  ( -1.612977847700450206E-50, 0.000000000000000000, -1.000000000000000000 ) ) ;
#31492 = CARTESIAN_POINT ( 'NONE',  ( 8.813458710706171928, 4.724716452304571490, 0.000000000000000000 ) ) ;
#31493 = ORIENTED_EDGE ( 'NONE', *, *, #2002, .T. ) ;
#31494 = DIRECTION ( 'NONE',  ( 0.000000000000000000, -1.000000000000000000, -4.687818848539279227E-49 ) ) ;
#31495 = CIRCLE ( 'NONE', #14252, 2.000000000000001776 ) ;
#31496 = CARTESIAN_POINT ( 'NONE',  ( 71.55402655318505367, -1.025126265847089213, -0.9317124430720324924 ) ) ;
#31497 = EDGE_LOOP ( 'NONE', ( #47182, #16613, #35641, #18132 ) ) ;
#31498 = DIRECTION ( 'NONE',  ( 1.000000000000000000, 0.000000000000000000, 0.000000000000000000 ) ) ;
#31499 = DIRECTION ( 'NONE',  ( 1.000000000000000000, 0.000000000000000000, 0.000000000000000000 ) ) ;
#31500 = CARTESIAN_POINT ( 'NONE',  ( -88.44597344681494633, 1.025126265847089213, 42.56828755692799149 ) ) ;
#31501 = VERTEX_POINT ( 'NONE', #26358 ) ;
#31502 = DIRECTION ( 'NONE',  ( 1.000000000000000000, 0.000000000000000000, 2.958228394578794708E-31 ) ) ;
#31503 = ADVANCED_FACE ( 'NONE', ( #2740 ), #30457, .T. ) ;
#31505 = ORIENTED_EDGE ( 'NONE', *, *, #8771, .T. ) ;
#31504 = EDGE_CURVE ( 'NONE', #4426, #42650, #31280, .T. ) ;
#31506 = VERTEX_POINT ( 'NONE', #18635 ) ;
#31507 = CARTESIAN_POINT ( 'NONE',  ( 349.9999999999999432, -180.9999999999999716, 355.9999999999997726 ) ) ;
#31508 = EDGE_CURVE ( 'NONE', #3587, #37149, #29442, .T. ) ;
#31509 = EDGE_CURVE ( 'NONE', #586, #43206, #13778, .T. ) ;
#31510 = B_SPLINE_CURVE_WITH_KNOTS ( 'NONE', 3,
 ( #27219, #46161, #31070, #6695 ),
 .UNSPECIFIED., .F., .F.,
 ( 4, 4 ),
 ( 0.000000000000000000, 0.2562577668812813236 ),
 .UNSPECIFIED. ) ;
#31511 = VERTEX_POINT ( 'NONE', #21995 ) ;
#31512 = LINE ( 'NONE', #47099, #31998 ) ;
#31513 = CARTESIAN_POINT ( 'NONE',  ( -128.4459734468149179, 0.000000000000000000, 162.5682875569279702 ) ) ;
#31514 = AXIS2_PLACEMENT_3D ( 'NONE', #21650, #3146, #45473 ) ;
#31515 = EDGE_CURVE ( 'NONE', #18948, #40759, #26056, .T. ) ;
#31516 = VECTOR ( 'NONE', #35679, 1000.000000000000000 ) ;
#31517 = EDGE_CURVE ( 'NONE', #19548, #8682, #39837, .T. ) ;
#31518 = CARTESIAN_POINT ( 'NONE',  ( 0.000000000000000000, -50.00000000000000000, 900.0000000000000000 ) ) ;
#31519 = ORIENTED_EDGE ( 'NONE', *, *, #40314, .F. ) ;
#31520 = AXIS2_PLACEMENT_3D ( 'NONE', #24709, #40355, #40844 ) ;
#31521 = CARTESIAN_POINT ( 'NONE',  ( -6.880036658038867436, 222.4999999999999716, -228.6347188485896140 ) ) ;
#31522 = CARTESIAN_POINT ( 'NONE',  ( 9.999999999999998224, 8.486842105263161073, -25.00000000000000000 ) ) ;
#31523 = CARTESIAN_POINT ( 'NONE',  ( 344.0000000000000000, 165.0000000000000000, -90.00000000000018474 ) ) ;
#31524 = ORIENTED_EDGE ( 'NONE', *, *, #11922, .T. ) ;
#31525 = B_SPLINE_CURVE_WITH_KNOTS ( 'NONE', 3,
 ( #1543, #40539, #783, #20526 ),
 .UNSPECIFIED., .F., .F.,
 ( 4, 4 ),
 ( 0.0006669682284780829038, 0.0007799402130931998951 ),
 .UNSPECIFIED. ) ;
#31526 = FACE_OUTER_BOUND ( 'NONE', #13941, .T. ) ;
#31527 = CARTESIAN_POINT ( 'NONE',  ( 74.32915281903215998, 1.750000000000010214, 121.8434138227750623 ) ) ;
#31528 = ORIENTED_EDGE ( 'NONE', *, *, #23641, .T. ) ;
#31529 = VERTEX_POINT ( 'NONE', #11220 ) ;
#31530 = ORIENTED_EDGE ( 'NONE', *, *, #7471, .T. ) ;
#31531 = CARTESIAN_POINT ( 'NONE',  ( 30.22736451279166658, 39.84193304692632154, -2.408242355805840784 ) ) ;
#31532 = DIRECTION ( 'NONE',  ( 0.000000000000000000, -0.8962124318248270161, 0.4436251537532894806 ) ) ;
#31533 = ORIENTED_EDGE ( 'NONE', *, *, #43874, .F. ) ;
#31534 = EDGE_CURVE ( 'NONE', #23498, #12400, #430, .T. ) ;
#31535 = CARTESIAN_POINT ( 'NONE',  ( -1.011271242968683426, -0.7347315653655928092, 3.333333333333333481 ) ) ;
#31536 = FACE_OUTER_BOUND ( 'NONE', #15465, .T. ) ;
#31537 = CARTESIAN_POINT ( 'NONE',  ( 169.0000000000000284, 165.0000000000000000, 355.9999999999998863 ) ) ;
#31538 = VECTOR ( 'NONE', #37550, 1000.000000000000000 ) ;
#31539 = EDGE_CURVE ( 'NONE', #20559, #16655, #10295, .T. ) ;
#31540 = CARTESIAN_POINT ( 'NONE',  ( -7.576114424932982594, 50.00000000000000711, 7.906207997025717304 ) ) ;
#31541 = CARTESIAN_POINT ( 'NONE',  ( -1.080340181645087272, 0.5751155560365547315, 9.966990753365125855 ) ) ;
#31542 = EDGE_CURVE ( 'NONE', #19831, #26993, #16077, .T. ) ;
#31543 = CARTESIAN_POINT ( 'NONE',  ( -0.1189258207540733747, -1.297644153576902326, 9.961922210043269388 ) ) ;
#31544 = DIRECTION ( 'NONE',  ( -1.000000000000000000, -0.000000000000000000, -0.000000000000000000 ) ) ;
#31545 = AXIS2_PLACEMENT_3D ( 'NONE', #45695, #10573, #10828 ) ;
#31546 = DIRECTION ( 'NONE',  ( 0.1191452206184307611, 0.000000000000000000, -0.9928768384869220975 ) ) ;
#31547 = LINE ( 'NONE', #3551, #25826 ) ;
#31548 = CARTESIAN_POINT ( 'NONE',  ( 34.32915281903212446, 1.750000000000010214, 119.7931612910808781 ) ) ;
#31549 = CARTESIAN_POINT ( 'NONE',  ( -2.943113374786527014, -2.672530809841224375, 3.247138655587367584 ) ) ;
#31550 = EDGE_CURVE ( 'NONE', #15399, #4762, #15326, .T. ) ;
#31551 = CARTESIAN_POINT ( 'NONE',  ( -14.99999999999906919, 17.00000000000000000, 0.000000000000000000 ) ) ;
#31552 = CARTESIAN_POINT ( 'NONE',  ( 344.0000000000000568, 167.0000000000000000, 349.9999999999998863 ) ) ;
#31553 = VECTOR ( 'NONE', #215, 1000.000000000000000 ) ;
#31554 = FACE_OUTER_BOUND ( 'NONE', #5568, .T. ) ;
#31555 = DIRECTION ( 'NONE',  ( -0.000000000000000000, -0.000000000000000000, 1.000000000000000000 ) ) ;
#31556 = EDGE_LOOP ( 'NONE', ( #49425, #27547, #31075, #13454 ) ) ;
#31557 = DIRECTION ( 'NONE',  ( 0.000000000000000000, 0.000000000000000000, 1.000000000000000000 ) ) ;
#31558 = DIRECTION ( 'NONE',  ( 1.000000000000000000, 0.000000000000000000, 2.958228394578794270E-31 ) ) ;
#31559 = CARTESIAN_POINT ( 'NONE',  ( 210.0000000000000568, 0.000000000000000000, 42.56828755692799149 ) ) ;
#31560 = VECTOR ( 'NONE', #45112, 1000.000000000000000 ) ;
#31561 = CARTESIAN_POINT ( 'NONE',  ( 0.000000000000000000, 17.00000000000000000, 0.000000000000000000 ) ) ;
#31562 = EDGE_CURVE ( 'NONE', #42175, #17726, #15817, .T. ) ;
#31563 = ORIENTED_EDGE ( 'NONE', *, *, #6431, .T. ) ;
#31564 = SURFACE_STYLE_FILL_AREA ( #15896 ) ;
#31565 = EDGE_LOOP ( 'NONE', ( #18443, #13796, #48916, #42240 ) ) ;
#31566 = DIRECTION ( 'NONE',  ( 0.000000000000000000, 0.000000000000000000, 1.000000000000000000 ) ) ;
#31567 = ADVANCED_FACE ( 'NONE', ( #30979 ), #35596, .F. ) ;
#31568 = EDGE_LOOP ( 'NONE', ( #22747, #44928, #12184, #25856 ) ) ;
#31569 = CARTESIAN_POINT ( 'NONE',  ( 154.3291528190321458, -1.750000000000009548, -160.2068387089191219 ) ) ;
#31570 = CARTESIAN_POINT ( 'NONE',  ( -44.94597344681493922, 2.143131898507880377E-16, 165.0000000000000000 ) ) ;
#31571 = ORIENTED_EDGE ( 'NONE', *, *, #43768, .T. ) ;
#31572 = CARTESIAN_POINT ( 'NONE',  ( 210.0000000000000568, 2.143131898507880377E-16, 159.0682875569279702 ) ) ;
#31573 = EDGE_LOOP ( 'NONE', ( #19268, #365, #48606, #19515 ) ) ;
#31574 = EDGE_CURVE ( 'NONE', #28100, #26320, #22711, .T. ) ;
#31575 = AXIS2_PLACEMENT_3D ( 'NONE', #33077, #33328, #25619 ) ;
#31576 = ADVANCED_FACE ( 'NONE', ( #8135 ), #19666, .T. ) ;
#31577 = ORIENTED_EDGE ( 'NONE', *, *, #20245, .T. ) ;
#31578 = LINE ( 'NONE', #12065, #26998 ) ;
#31579 = CYLINDRICAL_SURFACE ( 'NONE', #15049, 1.750000000000015543 ) ;
#31580 = AXIS2_PLACEMENT_3D ( 'NONE', #16699, #21557, #48465 ) ;
#31581 = VERTEX_POINT ( 'NONE', #39188 ) ;
#31582 = CARTESIAN_POINT ( 'NONE',  ( 360.0000000000001137, 181.0000000000000284, 355.9999999999998295 ) ) ;
#31583 = CARTESIAN_POINT ( 'NONE',  ( -126.6959734468149321, -1.749999999999997335, 120.8182875569279702 ) ) ;
#31584 = DIRECTION ( 'NONE',  ( 0.000000000000000000, 0.000000000000000000, -1.000000000000000000 ) ) ;
#31585 = VERTEX_POINT ( 'NONE', #23251 ) ;
#31586 = EDGE_CURVE ( 'NONE', #21707, #33352, #50583, .T. ) ;
#31587 = CARTESIAN_POINT ( 'NONE',  ( 181.0000000000000000, -252.4999999999999432, -349.9999999999999432 ) ) ;
#31588 = EDGE_CURVE ( 'NONE', #16652, #35927, #15567, .T. ) ;
#31589 = CYLINDRICAL_SURFACE ( 'NONE', #39549, 4.000000000000003553 ) ;
#31590 = EDGE_LOOP ( 'NONE', ( #1970, #18468, #12767, #4843 ) ) ;
#31591 = FACE_OUTER_BOUND ( 'NONE', #35704, .T. ) ;
#31592 = AXIS2_PLACEMENT_3D ( 'NONE', #16108, #20209, #31773 ) ;
#31593 = FACE_OUTER_BOUND ( 'NONE', #46812, .T. ) ;
#31594 = VECTOR ( 'NONE', #28433, 1000.000000000000000 ) ;
#31595 = ORIENTED_EDGE ( 'NONE', *, *, #12489, .F. ) ;
#31596 = FACE_OUTER_BOUND ( 'NONE', #11711, .T. ) ;
#31597 =( BOUNDED_CURVE ( )  B_SPLINE_CURVE ( 3, ( #44728, #5498, #21148, #10103 ),
 .UNSPECIFIED., .F., .F. ) 
 B_SPLINE_CURVE_WITH_KNOTS ( ( 4, 4 ),
 ( 0.000000000000000000, 1.570796326794896558 ),
 .UNSPECIFIED. ) 
 CURVE ( )  GEOMETRIC_REPRESENTATION_ITEM ( )  RATIONAL_B_SPLINE_CURVE ( ( 1.000000000000000000, 0.8047378541243649375, 0.8047378541243649375, 1.000000000000000000 ) ) 
 REPRESENTATION_ITEM ( '' )  );
#31598 = AXIS2_PLACEMENT_3D ( 'NONE', #43136, #27243, #26734 ) ;
#31599 = DIRECTION ( 'NONE',  ( -1.000000000000000000, -0.000000000000000000, -0.000000000000000000 ) ) ;
#31600 = VERTEX_POINT ( 'NONE', #46821 ) ;
#31601 = CIRCLE ( 'NONE', #38148, 5.000000000000000000 ) ;
#31602 = CARTESIAN_POINT ( 'NONE',  ( 24.87968592351591823, 28.06706927586064637, -8.600750091277037157 ) ) ;
#31603 = LINE ( 'NONE', #46932, #9383 ) ;
#31604 = CARTESIAN_POINT ( 'NONE',  ( -8.445973446814976526, 0.000000000000000000, -120.9317124430720725 ) ) ;
#31605 = CARTESIAN_POINT ( 'NONE',  ( -85.67084718096784002, -1.750000000000009326, 1.843413822775066269 ) ) ;
#31606 = EDGE_CURVE ( 'NONE', #25022, #2713, #27368, .T. ) ;
#31607 = VERTEX_POINT ( 'NONE', #7110 ) ;
#31608 = CARTESIAN_POINT ( 'NONE',  ( -1.512516825103204177, 0.5229758018505511474, 9.919954280166521698 ) ) ;
#31609 = CARTESIAN_POINT ( 'NONE',  ( 28.96803024440893992, 18.11533787072037072, 7.455576670931136185 ) ) ;
#31610 = DIRECTION ( 'NONE',  ( -1.000000000000000000, 0.000000000000000000, 0.000000000000000000 ) ) ;
#31611 = EDGE_LOOP ( 'NONE', ( #31878, #14438, #3720, #36394 ) ) ;
#31612 = EDGE_LOOP ( 'NONE', ( #48156, #23592, #4766, #2963 ) ) ;
#31613 = APPLICATION_PROTOCOL_DEFINITION ( 'draft international standard', 'automotive_design', 1998, #7939 ) ;
#31614 = DIRECTION ( 'NONE',  ( 0.000000000000000000, 0.000000000000000000, 1.000000000000000000 ) ) ;
#31615 = PLANE ( 'NONE',  #15193 ) ;
#31616 = AXIS2_PLACEMENT_3D ( 'NONE', #40144, #43223, #19619 ) ;
#31617 = CARTESIAN_POINT ( 'NONE',  ( -13.59579750444763668, 10.60877755095910935, 8.727788335465566760 ) ) ;
#31618 = CARTESIAN_POINT ( 'NONE',  ( 1.104477492316107146, 0.6506302558160963478, 9.957892297621020461 ) ) ;
#31619 = EDGE_LOOP ( 'NONE', ( #36755, #27621, #15697, #45457 ) ) ;
#31620 = LINE ( 'NONE', #47208, #42735 ) ;
#31621 = AXIS2_PLACEMENT_3D ( 'NONE', #27991, #11592, #38554 ) ;
#31622 = CARTESIAN_POINT ( 'NONE',  ( -166.6959734468149463, 1.750000000000010658, -79.18171244307201562 ) ) ;
#31623 = CARTESIAN_POINT ( 'NONE',  ( 181.0000000000000000, 175.0000000000000284, -360.0000000000001705 ) ) ;
#31624 = DIRECTION ( 'NONE',  ( 0.000000000000000000, 0.000000000000000000, 1.000000000000000000 ) ) ;
#31625 = ORIENTED_EDGE ( 'NONE', *, *, #36900, .T. ) ;
#31626 = CARTESIAN_POINT ( 'NONE',  ( 344.0000000000000568, 167.0000000000000000, 349.9999999999998863 ) ) ;
#31627 = ORIENTED_EDGE ( 'NONE', *, *, #9042, .F. ) ;
#31628 = DIRECTION ( 'NONE',  ( -0.000000000000000000, -0.000000000000000000, 1.000000000000000000 ) ) ;
#31629 = VECTOR ( 'NONE', #12894, 1000.000000000000000 ) ;
#31630 = ORIENTED_EDGE ( 'NONE', *, *, #32434, .F. ) ;
#31631 = FACE_OUTER_BOUND ( 'NONE', #5176, .T. ) ;
#31632 = CARTESIAN_POINT ( 'NONE',  ( 12.78770032058947237, 31.68259716188277864, 7.455576670931136185 ) ) ;
#31633 = CARTESIAN_POINT ( 'NONE',  ( -84.94597344681493212, 1.025126265847089435, 39.06828755692797728 ) ) ;
#31634 = CARTESIAN_POINT ( 'NONE',  ( -9.999999999999992895, -48.43825625180578953, 5.363892796379245986 ) ) ;
#31635 = VECTOR ( 'NONE', #24030, 1000.000000000000000 ) ;
#31636 = VERTEX_POINT ( 'NONE', #47073 ) ;
#31637 = AXIS2_PLACEMENT_3D ( 'NONE', #47350, #39207, #19936 ) ;
#31638 = EDGE_CURVE ( 'NONE', #16880, #42585, #47331, .T. ) ;
#31639 = CARTESIAN_POINT ( 'NONE',  ( -175.0000000000000000, 15.00000000000000000, 122.5000000000000142 ) ) ;
#31640 = EDGE_CURVE ( 'NONE', #41927, #6309, #36188, .T. ) ;
#31641 = CARTESIAN_POINT ( 'NONE',  ( 151.5540265531850537, 0.000000000000000000, -77.43171244307204404 ) ) ;
#31642 = VERTEX_POINT ( 'NONE', #34566 ) ;
#31643 = CARTESIAN_POINT ( 'NONE',  ( -208.4459734468149463, 0.000000000000000000, -37.43171244307205825 ) ) ;
#31644 = CARTESIAN_POINT ( 'NONE',  ( 356.0000000000000000, 165.0000000000000000, -110.0000000000002132 ) ) ;
#31645 = CARTESIAN_POINT ( 'NONE',  ( -204.9459734468148895, -1.025126265847089213, -0.9317124430720324924 ) ) ;
#31646 = VERTEX_POINT ( 'NONE', #19913 ) ;
#31647 = ADVANCED_FACE ( 'NONE', ( #50148 ), #28387, .F. ) ;
#31648 = B_SPLINE_CURVE_WITH_KNOTS ( 'NONE', 3,
 ( #14615, #34149, #49969, #33883 ),
 .UNSPECIFIED., .F., .F.,
 ( 4, 4 ),
 ( 0.000000000000000000, 0.001246897409371940492 ),
 .UNSPECIFIED. ) ;
#31649 = ORIENTED_EDGE ( 'NONE', *, *, #6691, .F. ) ;
#31650 = CARTESIAN_POINT ( 'NONE',  ( 130.0000000000012221, 17.00000000000000000, 5.000000000000004441 ) ) ;
#31651 = ADVANCED_FACE ( 'NONE', ( #1444 ), #8873, .T. ) ;
#31652 = EDGE_CURVE ( 'NONE', #8676, #10849, #30985, .T. ) ;
#31653 = VECTOR ( 'NONE', #42219, 1000.000000000000000 ) ;
#31654 = ORIENTED_EDGE ( 'NONE', *, *, #20040, .T. ) ;
#31655 = CARTESIAN_POINT ( 'NONE',  ( -33.89193117067290473, 21.24469349090191983, 910.0000000000000000 ) ) ;
#31656 = FACE_OUTER_BOUND ( 'NONE', #32329, .T. ) ;
#31657 = VECTOR ( 'NONE', #44482, 1000.000000000000000 ) ;
#31658 = ORIENTED_EDGE ( 'NONE', *, *, #44072, .F. ) ;
#31659 = CARTESIAN_POINT ( 'NONE',  ( 168.9999999999999716, -166.9999999999999432, -340.0000000000001137 ) ) ;
#31660 = VERTEX_POINT ( 'NONE', #24292 ) ;
#31661 = EDGE_CURVE ( 'NONE', #29268, #48485, #24395, .T. ) ;
#31662 = ORIENTED_EDGE ( 'NONE', *, *, #49886, .F. ) ;
#31663 = CARTESIAN_POINT ( 'NONE',  ( -7.726417830024645994, 6.396462539501611033, 9.390253821402618328 ) ) ;
#31665 = VECTOR ( 'NONE', #43930, 1000.000000000000000 ) ;
#31664 = PLANE ( 'NONE',  #20628 ) ;
#31666 = ORIENTED_EDGE ( 'NONE', *, *, #10300, .F. ) ;
#31667 = ORIENTED_EDGE ( 'NONE', *, *, #45385, .T. ) ;
#31668 = COLOUR_RGB ( '',0.7921568627450980005, 0.8196078431372548767, 0.9333333333333333481 ) ;
#31669 = VERTEX_POINT ( 'NONE', #20932 ) ;
#31670 = CARTESIAN_POINT ( 'NONE',  ( 343.9999999999999432, -183.0000000000001421, -358.0000000000003411 ) ) ;
#31671 = CARTESIAN_POINT ( 'NONE',  ( -86.69597344681494633, -1.750000000000009992, 160.8182875569279702 ) ) ;
#31672 = CARTESIAN_POINT ( 'NONE',  ( -166.6959734468149463, 1.750000000000010658, -119.1817124430720440 ) ) ;
#31673 = ORIENTED_EDGE ( 'NONE', *, *, #29761, .T. ) ;
#31674 = PLANE ( 'NONE',  #40381 ) ;
#31675 = ORIENTED_EDGE ( 'NONE', *, *, #27450, .T. ) ;
#31676 = AXIS2_PLACEMENT_3D ( 'NONE', #4114, #11820, #27213 ) ;
#31677 = DIRECTION ( 'NONE',  ( 1.586032892321651989E-16, 1.194346094642793337E-32, 1.000000000000000000 ) ) ;
#31678 = VERTEX_POINT ( 'NONE', #1195 ) ;
#31679 = PLANE ( 'NONE',  #41695 ) ;
#31680 = CARTESIAN_POINT ( 'NONE',  ( 35.05402655318504657, 1.025126265847088991, 162.5682875569279133 ) ) ;
#31681 = CARTESIAN_POINT ( 'NONE',  ( -8.176860274785726190, 5.756644512789648616, 9.282506307616472441 ) ) ;
#31682 = CARTESIAN_POINT ( 'NONE',  ( 0.7246461030033715112, -1.181777192779797314, 9.960033073700731876 ) ) ;
#31683 = LINE ( 'NONE', #24728, #25613 ) ;
#31684 = ORIENTED_EDGE ( 'NONE', *, *, #32789, .F. ) ;
#31685 = ORIENTED_EDGE ( 'NONE', *, *, #28456, .F. ) ;
#31686 = PLANE ( 'NONE',  #12179 ) ;
#31687 = CARTESIAN_POINT ( 'NONE',  ( 30.00000000000092726, 16.00000000000000000, -24.99999999999999289 ) ) ;
#31688 = EDGE_CURVE ( 'NONE', #10051, #26564, #21176, .T. ) ;
#31689 = DIRECTION ( 'NONE',  ( 0.000000000000000000, -1.000000000000000000, -0.000000000000000000 ) ) ;
#31690 = VECTOR ( 'NONE', #41344, 1000.000000000000000 ) ;
#31691 = VECTOR ( 'NONE', #43618, 1000.000000000000000 ) ;
#31692 = CARTESIAN_POINT ( 'NONE',  ( -45.42829307628559832, -21.98948915213271960, 8.356839323120299312 ) ) ;
#31693 = B_SPLINE_CURVE_WITH_KNOTS ( 'NONE', 3,
 ( #1705, #44775, #20692, #1461 ),
 .UNSPECIFIED., .F., .F.,
 ( 4, 4 ),
 ( 0.000000000000000000, 0.2562577668812812681 ),
 .UNSPECIFIED. ) ;
#31694 = ORIENTED_EDGE ( 'NONE', *, *, #2118, .F. ) ;
#31695 = CARTESIAN_POINT ( 'NONE',  ( -165.6708471809677974, 1.750000000000009548, -0.2068387089191121020 ) ) ;
#31696 = DIRECTION ( 'NONE',  ( -0.000000000000000000, -0.000000000000000000, 1.000000000000000000 ) ) ;
#31697 = EDGE_LOOP ( 'NONE', ( #23204, #45902, #19634, #34049 ) ) ;
#31698 = AXIS2_PLACEMENT_3D ( 'NONE', #12568, #42853, #16185 ) ;
#31699 = CARTESIAN_POINT ( 'NONE',  ( 8.277096487746778308, -50.00000000000000711, 7.455576670931136185 ) ) ;
#31700 = VECTOR ( 'NONE', #26911, 1000.000000000000000 ) ;
#31701 = AXIS2_PLACEMENT_3D ( 'NONE', #8865, #5520, #48827 ) ;
#31702 = CARTESIAN_POINT ( 'NONE',  ( -128.4459734468149179, 0.000000000000000000, 119.0682875569279986 ) ) ;
#31703 = PLANE ( 'NONE',  #50361 ) ;
#31704 = VERTEX_POINT ( 'NONE', #33003 ) ;
#31705 = B_SPLINE_CURVE_WITH_KNOTS ( 'NONE', 3,
 ( #12700, #2592, #36073, #45678 ),
 .UNSPECIFIED., .F., .F.,
 ( 4, 4 ),
 ( 0.003717756258871352318, 0.009855839347410961029 ),
 .UNSPECIFIED. ) ;
#31706 = ORIENTED_EDGE ( 'NONE', *, *, #24934, .F. ) ;
#31707 = CARTESIAN_POINT ( 'NONE',  ( 1.096405084303662569, 0.6872075889365651946, 9.947020504990323531 ) ) ;
#31708 = VECTOR ( 'NONE', #47102, 1000.000000000000000 ) ;
#31709 = CARTESIAN_POINT ( 'NONE',  ( 155.0540265531850537, 1.025126265847089657, 79.06828755692797017 ) ) ;
#31710 = ORIENTED_EDGE ( 'NONE', *, *, #20871, .F. ) ;
#31711 = VERTEX_POINT ( 'NONE', #24032 ) ;
#31712 = DIRECTION ( 'NONE',  ( -0.7233555441435719491, 0.6904757466825007794, -0.000000000000000000 ) ) ;
#31713 = CARTESIAN_POINT ( 'NONE',  ( 168.9999999999999716, -252.4999999999999432, -339.9999999999998863 ) ) ;
#31714 = CARTESIAN_POINT ( 'NONE',  ( -64.99999999999909051, 17.00000000000000000, -24.99999999999999289 ) ) ;
#31715 = LINE ( 'NONE', #4491, #12799 ) ;
#31716 = CARTESIAN_POINT ( 'NONE',  ( 210.0000000000000568, 0.000000000000000000, 0.8182875569279768335 ) ) ;
#31717 = ORIENTED_EDGE ( 'NONE', *, *, #27062, .F. ) ;
#31718 = VERTEX_POINT ( 'NONE', #40694 ) ;
#31719 = EDGE_CURVE ( 'NONE', #42713, #9801, #32736, .T. ) ;
#31720 = ORIENTED_EDGE ( 'NONE', *, *, #32170, .T. ) ;
#31721 = DIRECTION ( 'NONE',  ( 0.000000000000000000, 0.000000000000000000, 1.000000000000000000 ) ) ;
#31722 = ORIENTED_EDGE ( 'NONE', *, *, #41446, .F. ) ;
#31723 = B_SPLINE_CURVE_WITH_KNOTS ( 'NONE', 3,
 ( #5166, #9027, #20816, #43910 ),
 .UNSPECIFIED., .F., .F.,
 ( 4, 4 ),
 ( 2.577543251182695844E-16, 0.009782300387714808892 ),
 .UNSPECIFIED. ) ;
#31724 = AXIS2_PLACEMENT_3D ( 'NONE', #3529, #45611, #50183 ) ;
#31725 = DIRECTION ( 'NONE',  ( 1.000000000000000000, 0.000000000000000000, 0.000000000000000000 ) ) ;
#31726 = ORIENTED_EDGE ( 'NONE', *, *, #22820, .F. ) ;
#31727 = EDGE_LOOP ( 'NONE', ( #32774, #3340, #3469, #34754, #42117, #4251 ) ) ;
#31728 = CARTESIAN_POINT ( 'NONE',  ( -8.445973446814976526, 0.000000000000000000, 165.0000000000000000 ) ) ;
#31729 = CARTESIAN_POINT ( 'NONE',  ( 0.6595498452743703277, -16.59563386392009576, 3.266473740018926541 ) ) ;
#31730 = CARTESIAN_POINT ( 'NONE',  ( 210.0000000000000568, 0.000000000000000000, 82.56828755692799859 ) ) ;
#31731 = ORIENTED_EDGE ( 'NONE', *, *, #46857, .T. ) ;
#31732 = ORIENTED_EDGE ( 'NONE', *, *, #28399, .F. ) ;
#31733 = DIRECTION ( 'NONE',  ( 0.2599384441937613310, 0.8000082703740953871, 0.5407575913134970991 ) ) ;
#31734 = CARTESIAN_POINT ( 'NONE',  ( 21.23829395927641883, -2.816136035261161297, 229.0000000000000000 ) ) ;
#31735 = ORIENTED_EDGE ( 'NONE', *, *, #3526, .F. ) ;
#31736 =( BOUNDED_CURVE ( )  B_SPLINE_CURVE ( 3, ( #24043, #43011, #19422, #42748 ),
 .UNSPECIFIED., .F., .F. ) 
 B_SPLINE_CURVE_WITH_KNOTS ( ( 4, 4 ),
 ( 0.000000000000000000, 1.570796326794896558 ),
 .UNSPECIFIED. ) 
 CURVE ( )  GEOMETRIC_REPRESENTATION_ITEM ( )  RATIONAL_B_SPLINE_CURVE ( ( 1.000000000000000000, 0.8047378541243649375, 0.8047378541243649375, 1.000000000000000000 ) ) 
 REPRESENTATION_ITEM ( '' )  );
#31737 = CARTESIAN_POINT ( 'NONE',  ( -84.94597344681493212, -1.025126265847089435, 122.5682875569280128 ) ) ;
#31738 = CARTESIAN_POINT ( 'NONE',  ( -2.418900724918336298, -41.61933801977895087, -9.387872844313825738 ) ) ;
#31739 = CARTESIAN_POINT ( 'NONE',  ( 153.3040265531850537, 0.000000000000000000, 165.0000000000000000 ) ) ;
#31740 = EDGE_LOOP ( 'NONE', ( #16643, #20378, #44058, #43971 ) ) ;
#31741 = PLANE ( 'NONE',  #29163 ) ;
#31742 =( BOUNDED_CURVE ( )  B_SPLINE_CURVE ( 3, ( #4990, #40662, #43732, #48048 ),
 .UNSPECIFIED., .F., .F. ) 
 B_SPLINE_CURVE_WITH_KNOTS ( ( 4, 4 ),
 ( 3.141592653589793116, 4.712388980384689674 ),
 .UNSPECIFIED. ) 
 CURVE ( )  GEOMETRIC_REPRESENTATION_ITEM ( )  RATIONAL_B_SPLINE_CURVE ( ( 1.000000000000000000, 0.8047378541243649375, 0.8047378541243649375, 1.000000000000000000 ) ) 
 REPRESENTATION_ITEM ( '' )  );
#31743 = CYLINDRICAL_SURFACE ( 'NONE', #316, 0.5000000000000007772 ) ;
#31744 = DIRECTION ( 'NONE',  ( -1.000000000000000000, 0.000000000000000000, 0.000000000000000000 ) ) ;
#31745 = AXIS2_PLACEMENT_3D ( 'NONE', #12140, #46477, #8548 ) ;
#31746 = EDGE_CURVE ( 'NONE', #18422, #4997, #16282, .T. ) ;
#31747 = LINE ( 'NONE', #185, #946 ) ;
#31748 = DIRECTION ( 'NONE',  ( -1.156482317317870492E-16, 1.000000000000000000, 0.000000000000000000 ) ) ;
#31750 = CARTESIAN_POINT ( 'NONE',  ( -1.104213410210672430, -0.6509177773818179968, 9.976582533991678048 ) ) ;
#31749 =( BOUNDED_CURVE ( )  B_SPLINE_CURVE ( 3, ( #19130, #34820, #27353, #14787 ),
 .UNSPECIFIED., .F., .F. ) 
 B_SPLINE_CURVE_WITH_KNOTS ( ( 4, 4 ),
 ( 0.000000000000000000, 1.570796326794896558 ),
 .UNSPECIFIED. ) 
 CURVE ( )  GEOMETRIC_REPRESENTATION_ITEM ( )  RATIONAL_B_SPLINE_CURVE ( ( 1.000000000000000000, 0.8047378541243649375, 0.8047378541243649375, 1.000000000000000000 ) ) 
 REPRESENTATION_ITEM ( '' )  );
#31751 = CARTESIAN_POINT ( 'NONE',  ( 30.00000000000123279, 16.00000000000000000, 5.000000000000004441 ) ) ;
#31752 = ORIENTED_EDGE ( 'NONE', *, *, #6440, .F. ) ;
#31753 = CARTESIAN_POINT ( 'NONE',  ( 75.05402655318509630, 2.143131898507880377E-16, 165.0000000000000000 ) ) ;
#31754 = AXIS2_PLACEMENT_3D ( 'NONE', #2347, #17989, #1855 ) ;
#31755 = PLANE ( 'NONE',  #867 ) ;
#31756 = ORIENTED_EDGE ( 'NONE', *, *, #4619, .T. ) ;
#31757 = DIRECTION ( 'NONE',  ( -0.000000000000000000, -0.000000000000000000, 1.000000000000000000 ) ) ;
#31758 = DIRECTION ( 'NONE',  ( -1.000000000000000000, 0.000000000000000000, -0.000000000000000000 ) ) ;
#31759 = CARTESIAN_POINT ( 'NONE',  ( 350.0000000000000000, 169.0000000000000000, -340.0000000000001705 ) ) ;
#31760 = ORIENTED_EDGE ( 'NONE', *, *, #24303, .T. ) ;
#31761 = LINE ( 'NONE', #47346, #30669 ) ;
#31762 = ORIENTED_EDGE ( 'NONE', *, *, #25498, .F. ) ;
#31763 = ORIENTED_EDGE ( 'NONE', *, *, #46859, .F. ) ;
#31764 = CARTESIAN_POINT ( 'NONE',  ( -6.695973446814940111, 1.750000000000023315, -159.1817124430720298 ) ) ;
#31765 = CARTESIAN_POINT ( 'NONE',  ( 210.0000000000000568, 2.143131898507880377E-16, -0.9317124430720331585 ) ) ;
#31766 = ORIENTED_EDGE ( 'NONE', *, *, #21891, .F. ) ;
#31767 = CARTESIAN_POINT ( 'NONE',  ( 350.0000000000001137, 185.0000000000000284, 343.9999999999997726 ) ) ;
#31768 = CARTESIAN_POINT ( 'NONE',  ( 344.0000000000000000, 165.0000000000001990, -340.0000000000002842 ) ) ;
#31769 = ORIENTED_EDGE ( 'NONE', *, *, #27024, .F. ) ;
#31770 = ADVANCED_FACE ( 'NONE', ( #36353 ), #5018, .F. ) ;
#31771 = CARTESIAN_POINT ( 'NONE',  ( -194.9999999999999432, 164.9999999999999716, 132.0000000000001137 ) ) ;
#31772 = ORIENTED_EDGE ( 'NONE', *, *, #36875, .T. ) ;
#31773 = DIRECTION ( 'NONE',  ( 0.000000000000000000, 0.000000000000000000, 1.000000000000000000 ) ) ;
#31774 = DIRECTION ( 'NONE',  ( -1.000000000000000000, -0.000000000000000000, -0.000000000000000000 ) ) ;
#31775 = CARTESIAN_POINT ( 'NONE',  ( 210.0000000000000568, 2.143131898507881856E-16, 119.0682875569279560 ) ) ;
#31776 = EDGE_LOOP ( 'NONE', ( #39963, #38269 ) ) ;
#31777 = CARTESIAN_POINT ( 'NONE',  ( 193.3040265531851105, 0.000000000000000000, 165.0000000000000000 ) ) ;
#31778 = CARTESIAN_POINT ( 'NONE',  ( 359.9999999999998295, -183.3431457505077731, 358.3431457505076310 ) ) ;
#31779 = VERTEX_POINT ( 'NONE', #17080 ) ;
#31780 = ORIENTED_EDGE ( 'NONE', *, *, #27518, .T. ) ;
#31781 = EDGE_LOOP ( 'NONE', ( #45360, #11741, #12981, #38719 ) ) ;
#31782 = PLANE ( 'NONE',  #36114 ) ;
#31783 = EDGE_CURVE ( 'NONE', #37447, #4392, #20168, .T. ) ;
#31784 = EDGE_CURVE ( 'NONE', #16304, #32679, #27976, .T. ) ;
#31785 = DIRECTION ( 'NONE',  ( -1.000000000000000000, 0.000000000000000000, 0.000000000000000000 ) ) ;
#31786 = ORIENTED_EDGE ( 'NONE', *, *, #12073, .F. ) ;
#31787 = CARTESIAN_POINT ( 'NONE',  ( -13.59579750444763668, 10.60877755095910935, 8.727788335465566760 ) ) ;
#31788 = DIRECTION ( 'NONE',  ( -0.000000000000000000, -1.000000000000000000, 2.537652627714643577E-15 ) ) ;
#31789 = EDGE_CURVE ( 'NONE', #16425, #10758, #16634, .T. ) ;
#31790 = FACE_OUTER_BOUND ( 'NONE', #15218, .T. ) ;
#31791 = LINE ( 'NONE', #16626, #27642 ) ;
#31792 = CARTESIAN_POINT ( 'NONE',  ( -85.67084718096784002, 1.750000000000009326, 161.8434138227750907 ) ) ;
#31793 = VECTOR ( 'NONE', #36287, 1000.000000000000000 ) ;
#31794 = CARTESIAN_POINT ( 'NONE',  ( -164.9999999999990905, 17.00000000000000000, 0.000000000000000000 ) ) ;
#31795 = LINE ( 'NONE', #47378, #2792 ) ;
#31796 = CARTESIAN_POINT ( 'NONE',  ( 191.5540265531851105, 0.000000000000000000, -37.43171244307205825 ) ) ;
#31797 = CARTESIAN_POINT ( 'NONE',  ( 35.34822294759176486, 12.62826869953554976, -3.721387749823083180 ) ) ;
#31798 = ADVANCED_FACE ( 'NONE', ( #24792 ), #15420, .T. ) ;
#31799 = CYLINDRICAL_SURFACE ( 'NONE', #9684, 1.750000000000008438 ) ;
#31800 = EDGE_CURVE ( 'NONE', #40868, #40145, #6027, .T. ) ;
#31801 = CARTESIAN_POINT ( 'NONE',  ( 0.000000000000000000, 0.000000000000000000, 0.000000000000000000 ) ) ;
#31802 = ADVANCED_FACE ( 'NONE', ( #49588, #41177 ), #22197, .F. ) ;
#31803 = EDGE_CURVE ( 'NONE', #50130, #48877, #13730, .T. ) ;
#31804 = CARTESIAN_POINT ( 'NONE',  ( -206.6959734468149463, 1.750000000000010214, -39.18171244307202983 ) ) ;
#31805 = CARTESIAN_POINT ( 'NONE',  ( -14.49999999999999822, 12.98684210526315930, 19.37312575500900280 ) ) ;
#31806 = ORIENTED_EDGE ( 'NONE', *, *, #9855, .F. ) ;
#31807 = LINE ( 'NONE', #43580, #26974 ) ;
#31808 = AXIS2_PLACEMENT_3D ( 'NONE', #47009, #16012, #39617 ) ;
#31809 = EDGE_CURVE ( 'NONE', #31434, #27847, #38108, .T. ) ;
#31810 = LINE ( 'NONE', #47388, #17117 ) ;
#31811 = CARTESIAN_POINT ( 'NONE',  ( 151.5540265531850537, -1.025126265847089213, 162.5682875569279133 ) ) ;
#31812 = VERTEX_POINT ( 'NONE', #18320 ) ;
#31813 = CARTESIAN_POINT ( 'NONE',  ( 30.00000000000029132, 17.00000000000000000, -84.99999999999998579 ) ) ;
#31814 = ORIENTED_EDGE ( 'NONE', *, *, #40244, .T. ) ;
#31815 = FACE_OUTER_BOUND ( 'NONE', #48402, .T. ) ;
#31816 = EDGE_LOOP ( 'NONE', ( #6944, #34295, #3119, #39048 ) ) ;
#31817 = LINE ( 'NONE', #46901, #33642 ) ;
#31818 = CARTESIAN_POINT ( 'NONE',  ( 0.7139173712341854161, -1.401061409226349141, 9.927288994922818688 ) ) ;
#31819 = CARTESIAN_POINT ( 'NONE',  ( 164.9999999999999716, -174.9999999999999716, -344.0000000000001137 ) ) ;
#31820 = ORIENTED_EDGE ( 'NONE', *, *, #19694, .T. ) ;
#31821 = CARTESIAN_POINT ( 'NONE',  ( -208.4459734468148611, 1.025126265847089213, 159.0682875569279418 ) ) ;
#31822 = EDGE_CURVE ( 'NONE', #49726, #20342, #37369, .T. ) ;
#31824 = ORIENTED_EDGE ( 'NONE', *, *, #48842, .T. ) ;
#31823 = B_SPLINE_CURVE_WITH_KNOTS ( 'NONE', 3,
 ( #24731, #20111, #884, #39890 ),
 .UNSPECIFIED., .F., .F.,
 ( 4, 4 ),
 ( 5.445986106959422297E-16, 0.009782300387714812362 ),
 .UNSPECIFIED. ) ;
#31825 = EDGE_CURVE ( 'NONE', #22094, #16336, #17583, .T. ) ;
#31826 = AXIS2_PLACEMENT_3D ( 'NONE', #42252, #3762, #4018 ) ;
#31827 = EDGE_CURVE ( 'NONE', #8241, #23844, #41751, .T. ) ;
#31828 = ORIENTED_EDGE ( 'NONE', *, *, #47784, .F. ) ;
#31829 = CYLINDRICAL_SURFACE ( 'NONE', #22091, 1.749999999999987566 ) ;
#31830 = DIRECTION ( 'NONE',  ( 0.000000000000000000, 0.000000000000000000, 1.000000000000000000 ) ) ;
#31831 = ORIENTED_EDGE ( 'NONE', *, *, #9797, .F. ) ;
#31832 = PLANE ( 'NONE',  #24606 ) ;
#31833 = CARTESIAN_POINT ( 'NONE',  ( 113.3040265531850537, 1.749999999999997335, -79.18171244307201562 ) ) ;
#31834 = EDGE_CURVE ( 'NONE', #19505, #26902, #29330, .T. ) ;
#31835 = CARTESIAN_POINT ( 'NONE',  ( 210.0000000000000568, 0.000000000000000000, 0.8182875569279768335 ) ) ;
#31836 = CARTESIAN_POINT ( 'NONE',  ( -8.019230367734902387, 14.74354227315965282, -9.233365092205394475 ) ) ;
#31837 = ADVANCED_FACE ( 'NONE', ( #2193 ), #34004, .T. ) ;
#31838 = DIRECTION ( 'NONE',  ( 0.000000000000000000, -1.000000000000000000, 0.000000000000000000 ) ) ;
#31839 = ORIENTED_EDGE ( 'NONE', *, *, #33450, .T. ) ;
#31840 = CARTESIAN_POINT ( 'NONE',  ( 153.3040265531850537, -1.750000000000010214, -39.18171244307202983 ) ) ;
#31841 = CARTESIAN_POINT ( 'NONE',  ( 155.0540265531850537, 2.143131898507880377E-16, 39.06828755692798438 ) ) ;
#31842 = ORIENTED_EDGE ( 'NONE', *, *, #37613, .T. ) ;
#31843 = CARTESIAN_POINT ( 'NONE',  ( -87.72109971266203843, 1.750000000000009548, -0.2068387089191121020 ) ) ;
#31844 = LINE ( 'NONE', #43359, #40696 ) ;
#31845 = B_SPLINE_SURFACE_WITH_KNOTS ( 'NONE', 3, 3, ( 
 ( #7301, #26810, #50612, #31430 ),
 ( #31692, #22947, #27582, #50095 ),
 ( #27055, #8081, #39389, #35537 ),
 ( #46262, #4225, #30930, #7060 ) ),
 .UNSPECIFIED., .F., .F., .F.,
 ( 4, 4 ),
 ( 4, 4 ),
 ( 0.000000000000000000, 1.000000000000000000 ),
 ( 0.000000000000000000, 1.000000000000000000 ),
 .UNSPECIFIED. ) ;
#31846 = ORIENTED_EDGE ( 'NONE', *, *, #2071, .T. ) ;
#31847 = FACE_OUTER_BOUND ( 'NONE', #41519, .T. ) ;
#31848 = DIRECTION ( 'NONE',  ( -1.000000000000000000, 0.000000000000000000, 0.000000000000000000 ) ) ;
#31849 = CARTESIAN_POINT ( 'NONE',  ( -44.94597344681493922, -1.025126265847089657, -80.93171244307201562 ) ) ;
#31850 = CARTESIAN_POINT ( 'NONE',  ( 0.4400426740873927822, -2.015233077865103972, 9.886433018048071730 ) ) ;
#31851 = EDGE_LOOP ( 'NONE', ( #2717, #22793, #43861, #19990 ) ) ;
#31852 = EDGE_CURVE ( 'NONE', #7869, #5114, #4797, .T. ) ;
#31853 = LINE ( 'NONE', #1305, #48216 ) ;
#31854 = CARTESIAN_POINT ( 'NONE',  ( 29.61572577327002520, 16.11461842845735859, 8.807470649214879543 ) ) ;
#31855 = CARTESIAN_POINT ( 'NONE',  ( 14.29087950072012170, 9.652079258044652832, 8.727788335465566760 ) ) ;
#31856 = VERTEX_POINT ( 'NONE', #49090 ) ;
#31857 = EDGE_CURVE ( 'NONE', #4748, #15011, #47362, .T. ) ;
#31858 = ORIENTED_EDGE ( 'NONE', *, *, #50432, .T. ) ;
#31859 = LINE ( 'NONE', #47453, #11405 ) ;
#31860 = CARTESIAN_POINT ( 'NONE',  ( -126.6959734468149321, -1.749999999999997113, -39.18171244307202983 ) ) ;
#31861 = EDGE_CURVE ( 'NONE', #7906, #18739, #40848, .T. ) ;
#31862 = ADVANCED_FACE ( 'NONE', ( #33754 ), #10396, .T. ) ;
#31863 = AXIS2_PLACEMENT_3D ( 'NONE', #2615, #21622, #10077 ) ;
#31864 = CARTESIAN_POINT ( 'NONE',  ( -1.011271242968683426, -0.7347315653655928092, -10.00000000000000000 ) ) ;
#31865 = LINE ( 'NONE', #8767, #31380 ) ;
#31866 = VERTEX_POINT ( 'NONE', #37609 ) ;
#31867 = EDGE_CURVE ( 'NONE', #17646, #47659, #22420, .T. ) ;
#31868 = CARTESIAN_POINT ( 'NONE',  ( 168.9999999999999716, -7.999999999999952038, -340.0000000000001137 ) ) ;
#31869 = EDGE_CURVE ( 'NONE', #41575, #2449, #21422, .T. ) ;
#31870 = PLANE ( 'NONE',  #42518 ) ;
#31871 = CARTESIAN_POINT ( 'NONE',  ( 34.91952936320839740, -13.67027684621004546, -9.422646554964178023 ) ) ;
#31872 = CLOSED_SHELL ( 'NONE', ( #13829, #35360, #10809, #2990, #18281, #15983, #20971, #43386, #46780, #40301, #48121, #22702, #38447, #49897, #27295, #31260, #8895, #10185 ) ) ;
#31873 = FACE_OUTER_BOUND ( 'NONE', #49001, .T. ) ;
#31874 = VERTEX_POINT ( 'NONE', #7296 ) ;
#31875 = CARTESIAN_POINT ( 'NONE',  ( 193.3040265531851105, 0.000000000000000000, 165.0000000000000000 ) ) ;
#31876 = ORIENTED_EDGE ( 'NONE', *, *, #38117, .F. ) ;
#31877 = DIRECTION ( 'NONE',  ( 1.132880637372608740E-16, 4.718402560806925739E-50, 1.000000000000000000 ) ) ;
#31878 = ORIENTED_EDGE ( 'NONE', *, *, #35781, .T. ) ;
#31879 = FACE_OUTER_BOUND ( 'NONE', #36043, .T. ) ;
#31880 = CARTESIAN_POINT ( 'NONE',  ( 28.52604530808654815, 41.07801380285680892, -3.760136334089591248 ) ) ;
#31881 = DIRECTION ( 'NONE',  ( 0.000000000000000000, 6.123233995736766036E-17, -1.000000000000000000 ) ) ;
#31882 = LINE ( 'NONE', #41514, #9940 ) ;
#31883 = EDGE_LOOP ( 'NONE', ( #49513, #37091, #27729, #46122 ) ) ;
#31884 = CARTESIAN_POINT ( 'NONE',  ( 0.6883547519190692521, -1.010122381805036440, 9.969517326150320713 ) ) ;
#31885 = ADVANCED_FACE ( 'NONE', ( #42688 ), #7561, .F. ) ;
#31886 = LINE ( 'NONE', #4420, #9024 ) ;
#31887 = VERTEX_POINT ( 'NONE', #34510 ) ;
#31888 = DIRECTION ( 'NONE',  ( -1.000000000000000000, 0.000000000000000000, 4.625929269271584521E-16 ) ) ;
#31889 = CARTESIAN_POINT ( 'NONE',  ( -125.6708471809678542, 1.749999999999996669, 159.7931612910809065 ) ) ;
#31890 = CARTESIAN_POINT ( 'NONE',  ( 5.551115123125782702E-14, -184.9999999999999716, 355.9999999999997726 ) ) ;
#31891 =( BOUNDED_CURVE ( )  B_SPLINE_CURVE ( 3, ( #33647, #40335, #37018, #29532 ),
 .UNSPECIFIED., .F., .F. ) 
 B_SPLINE_CURVE_WITH_KNOTS ( ( 4, 4 ),
 ( 3.141592653589793116, 4.712388980384689674 ),
 .UNSPECIFIED. ) 
 CURVE ( )  GEOMETRIC_REPRESENTATION_ITEM ( )  RATIONAL_B_SPLINE_CURVE ( ( 1.000000000000000000, 0.8047378541243649375, 0.8047378541243649375, 1.000000000000000000 ) ) 
 REPRESENTATION_ITEM ( '' )  );
#31892 = EDGE_LOOP ( 'NONE', ( #40211, #48758, #6235, #9056, #43806, #49863 ) ) ;
#31893 = PRODUCT_RELATED_PRODUCT_CATEGORY ( 'part', '', ( #37631 ) ) ;
#31894 = EDGE_LOOP ( 'NONE', ( #8019, #42586, #42268, #37800, #41207, #45098, #39684, #363 ) ) ;
#31895 = CARTESIAN_POINT ( 'NONE',  ( -119.9999999999978400, 17.00000000000000000, 95.00000000000000000 ) ) ;
#31896 = AXIS2_PLACEMENT_3D ( 'NONE', #4270, #39680, #39935 ) ;
#31897 = ORIENTED_EDGE ( 'NONE', *, *, #31142, .F. ) ;
#31898 = DIRECTION ( 'NONE',  ( 0.000000000000000000, 0.000000000000000000, 1.000000000000000000 ) ) ;
#31899 = DIRECTION ( 'NONE',  ( 0.000000000000000000, 0.9749645535258953943, 0.2223603367690637489 ) ) ;
#31900 = CARTESIAN_POINT ( 'NONE',  ( -1.468446590252919348, -0.3226319952343834063, 9.953784399990620813 ) ) ;
#31901 = EDGE_LOOP ( 'NONE', ( #19753, #6822, #30040, #34706 ) ) ;
#31903 = VECTOR ( 'NONE', #27494, 1000.000000000000000 ) ;
#31902 = DIRECTION ( 'NONE',  ( 1.000000000000000000, 0.000000000000000000, 0.000000000000000000 ) ) ;
#31904 = AXIS2_PLACEMENT_3D ( 'NONE', #16424, #39537, #30 ) ;
#31905 = ORIENTED_EDGE ( 'NONE', *, *, #23317, .T. ) ;
#31906 = ADVANCED_FACE ( 'NONE', ( #3955 ), #18829, .F. ) ;
#31907 = CIRCLE ( 'NONE', #23690, 4.000000000000003553 ) ;
#31908 = CARTESIAN_POINT ( 'NONE',  ( 210.0000000000000568, 0.000000000000000000, 2.568287556927987048 ) ) ;
#31909 = CIRCLE ( 'NONE', #46606, 0.5000000000000004441 ) ;
#31910 = LINE ( 'NONE', #44181, #45967 ) ;
#31911 = ORIENTED_EDGE ( 'NONE', *, *, #41692, .T. ) ;
#31912 = ORIENTED_EDGE ( 'NONE', *, *, #2457, .F. ) ;
#31913 = ORIENTED_EDGE ( 'NONE', *, *, #47710, .T. ) ;
#31914 = LINE ( 'NONE', #7543, #12385 ) ;
#31915 = FILL_AREA_STYLE ('',( #28553 ) ) ;
#31916 = CARTESIAN_POINT ( 'NONE',  ( -6.909265173666245374, 36.86491375218297861, 8.100132398494514163 ) ) ;
#31917 = PRODUCT_DEFINITION_CONTEXT ( 'detailed design', #37166, 'design' ) ;
#31918 = ORIENTED_EDGE ( 'NONE', *, *, #11749, .F. ) ;
#31919 = CARTESIAN_POINT ( 'NONE',  ( -8.445973446814962315, -1.025126265847096985, -0.9317124430720461481 ) ) ;
#31920 = ORIENTED_EDGE ( 'NONE', *, *, #24660, .F. ) ;
#31921 = PLANE ( 'NONE',  #6156 ) ;
#31922 = VERTEX_POINT ( 'NONE', #11400 ) ;
#31923 = CARTESIAN_POINT ( 'NONE',  ( 0.000000000000000000, 0.000000000000000000, 0.000000000000000000 ) ) ;
#31924 = LINE ( 'NONE', #39618, #32593 ) ;
#31925 = DIRECTION ( 'NONE',  ( 1.000000000000000000, 0.000000000000000000, 0.000000000000000000 ) ) ;
#31926 = EDGE_CURVE ( 'NONE', #14555, #47244, #50351, .T. ) ;
#31927 = ADVANCED_FACE ( 'NONE', ( #39132 ), #11919, .F. ) ;
#31928 = LINE ( 'NONE', #12406, #41415 ) ;
#31929 = CARTESIAN_POINT ( 'NONE',  ( 356.0000000000006253, 167.0000000000000000, 341.9999999999998295 ) ) ;
#31930 = FACE_OUTER_BOUND ( 'NONE', #42363, .T. ) ;
#31931 = ORIENTED_EDGE ( 'NONE', *, *, #39555, .T. ) ;
#31932 = EDGE_LOOP ( 'NONE', ( #29474, #44487, #42758, #42512 ) ) ;
#31933 = CARTESIAN_POINT ( 'NONE',  ( 42.51732812238058301, -47.49695244670218131, 5.000000000000000000 ) ) ;
#31934 = EDGE_CURVE ( 'NONE', #3038, #32533, #23199, .T. ) ;
#31935 = PLANE ( 'NONE',  #26088 ) ;
#31936 = FACE_OUTER_BOUND ( 'NONE', #48913, .T. ) ;
#31937 = EDGE_CURVE ( 'NONE', #12984, #17110, #7822, .T. ) ;
#31938 = EDGE_CURVE ( 'NONE', #22255, #22371, #41080, .T. ) ;
#31939 = VECTOR ( 'NONE', #48280, 1000.000000000000000 ) ;
#31940 = CARTESIAN_POINT ( 'NONE',  ( -4.945973446814903696, 2.143131898507912917E-16, 165.0000000000000000 ) ) ;
#31941 = VECTOR ( 'NONE', #35639, 1000.000000000000000 ) ;
#31942 = EDGE_LOOP ( 'NONE', ( #25140, #6956 ) ) ;
#31943 = LINE ( 'NONE', #27058, #23755 ) ;
#31944 = EDGE_CURVE ( 'NONE', #24104, #19505, #9989, .T. ) ;
#31945 = LINE ( 'NONE', #1143, #28812 ) ;
#31946 = VERTEX_POINT ( 'NONE', #50089 ) ;
#31947 = VECTOR ( 'NONE', #389, 1000.000000000000000 ) ;
#31948 = CYLINDRICAL_SURFACE ( 'NONE', #7421, 2.000000000000001776 ) ;
#31949 = CARTESIAN_POINT ( 'NONE',  ( 155.0540265531850537, -1.025126265847089435, 122.5682875569280128 ) ) ;
#31950 = CARTESIAN_POINT ( 'NONE',  ( 9.999999999999994671, -1.084202172485504187E-16, 9.303249460322209785 ) ) ;
#31951 = VERTEX_POINT ( 'NONE', #42943 ) ;
#31952 = VERTEX_POINT ( 'NONE', #7052 ) ;
#31953 = CARTESIAN_POINT ( 'NONE',  ( 154.1026953830863420, 103.0380105690400683, 23.74256005001722158 ) ) ;
#31954 = CARTESIAN_POINT ( 'NONE',  ( 23.26005729352310425, 44.90397804740356236, 7.906207997025717304 ) ) ;
#31955 = ORIENTED_EDGE ( 'NONE', *, *, #34223, .F. ) ;
#31956 = ORIENTED_EDGE ( 'NONE', *, *, #50609, .T. ) ;
#31957 = DIRECTION ( 'NONE',  ( -1.000000000000000000, 0.000000000000000000, 0.000000000000000000 ) ) ;
#31958 = CARTESIAN_POINT ( 'NONE',  ( -49.75871208702130133, -40.58472229863598102, -5.000000000000000000 ) ) ;
#31959 = CARTESIAN_POINT ( 'NONE',  ( -5.000000000000000000, 184.8000000000000114, -359.8000000000002387 ) ) ;
#31960 = CYLINDRICAL_SURFACE ( 'NONE', #49312, 4.000000000000003553 ) ;
#31961 = ORIENTED_EDGE ( 'NONE', *, *, #12367, .T. ) ;
#31962 = ORIENTED_EDGE ( 'NONE', *, *, #17243, .F. ) ;
#31963 = ORIENTED_EDGE ( 'NONE', *, *, #45914, .T. ) ;
#31964 = EDGE_CURVE ( 'NONE', #19831, #38131, #15002, .T. ) ;
#31965 = DIRECTION ( 'NONE',  ( -0.000000000000000000, -0.000000000000000000, -1.000000000000000000 ) ) ;
#31966 = VECTOR ( 'NONE', #29970, 1000.000000000000000 ) ;
#31967 = ORIENTED_EDGE ( 'NONE', *, *, #11541, .F. ) ;
#31968 = VECTOR ( 'NONE', #22697, 1000.000000000000000 ) ;
#31969 = CARTESIAN_POINT ( 'NONE',  ( 71.55402655318505367, 0.000000000000000000, -120.9317124430720725 ) ) ;
#31970 = ORIENTED_EDGE ( 'NONE', *, *, #49125, .T. ) ;
#31971 =( BOUNDED_CURVE ( )  B_SPLINE_CURVE ( 3, ( #21128, #25231, #9830, #17029 ),
 .UNSPECIFIED., .F., .F. ) 
 B_SPLINE_CURVE_WITH_KNOTS ( ( 4, 4 ),
 ( 3.141592653589793116, 4.712388980384689674 ),
 .UNSPECIFIED. ) 
 CURVE ( )  GEOMETRIC_REPRESENTATION_ITEM ( )  RATIONAL_B_SPLINE_CURVE ( ( 1.000000000000000000, 0.8047378541243649375, 0.8047378541243649375, 1.000000000000000000 ) ) 
 REPRESENTATION_ITEM ( '' )  );
#31972 = ORIENTED_EDGE ( 'NONE', *, *, #26656, .F. ) ;
#31973 = CARTESIAN_POINT ( 'NONE',  ( -6.695973446814940111, -1.750000000000023315, -159.1817124430720298 ) ) ;
#31974 = CIRCLE ( 'NONE', #23762, 10.00000000000000000 ) ;
#31975 = CARTESIAN_POINT ( 'NONE',  ( -0.5000000000000000000, -0.5000000000000000000, 1000.000000000000000 ) ) ;
#31976 = ORIENTED_EDGE ( 'NONE', *, *, #9089, .F. ) ;
#31977 = ORIENTED_EDGE ( 'NONE', *, *, #2946, .T. ) ;
#31978 = DIRECTION ( 'NONE',  ( 1.000000000000000000, 0.000000000000000000, 0.000000000000000000 ) ) ;
#31979 = CARTESIAN_POINT ( 'NONE',  ( 35.05402655318504657, 2.143131898507880377E-16, -157.4317124430720014 ) ) ;
#31980 = ORIENTED_EDGE ( 'NONE', *, *, #2614, .F. ) ;
#31981 = AXIS2_PLACEMENT_3D ( 'NONE', #19303, #31118, #19551 ) ;
#31982 = LINE ( 'NONE', #43755, #30576 ) ;
#31983 = CARTESIAN_POINT ( 'NONE',  ( -208.4459734468149463, 0.000000000000000000, 122.5682875569279702 ) ) ;
#31984 = CARTESIAN_POINT ( 'NONE',  ( 210.0000000000000568, 0.000000000000000000, 162.5682875569279702 ) ) ;
#31985 = ADVANCED_FACE ( 'NONE', ( #35038 ), #49830, .F. ) ;
#31986 = EDGE_CURVE ( 'NONE', #24656, #29740, #11156, .T. ) ;
#31987 = CARTESIAN_POINT ( 'NONE',  ( 36.08557433729230723, -35.58569447144768105, 7.455576670931136185 ) ) ;
#31988 = ORIENTED_EDGE ( 'NONE', *, *, #514, .T. ) ;
#31989 = CARTESIAN_POINT ( 'NONE',  ( 85.00000000000184741, 17.00000000000000000, 65.00000000000000000 ) ) ;
#31990 = CARTESIAN_POINT ( 'NONE',  ( -126.6959734468149321, -1.749999999999996891, 160.8182875569279702 ) ) ;
#31991 = CARTESIAN_POINT ( 'NONE',  ( -10.28825587112213746, 13.03847615613166333, 3.266473740018926541 ) ) ;
#31992 = ADVANCED_FACE ( 'NONE', ( #46008 ), #19086, .T. ) ;
#31993 = CARTESIAN_POINT ( 'NONE',  ( 33.30402655318503946, 1.750000000000009992, 0.8182875569279768335 ) ) ;
#31994 = EDGE_CURVE ( 'NONE', #1434, #20980, #15246, .T. ) ;
#31995 = EDGE_CURVE ( 'NONE', #31059, #49554, #15264, .T. ) ;
#31996 = CARTESIAN_POINT ( 'NONE',  ( 31.55402655318503236, 1.025126265847089657, 119.0682875569279560 ) ) ;
#31997 = CARTESIAN_POINT ( 'NONE',  ( -1.468713901642213493, -0.3220470327672489419, 9.927319414211227766 ) ) ;
#31998 = VECTOR ( 'NONE', #16102, 1000.000000000000000 ) ;
#31999 = CARTESIAN_POINT ( 'NONE',  ( 4.204997580903516941, -7.388441598285492518, 229.0000000000000000 ) ) ;
#32000 = AXIS2_PLACEMENT_3D ( 'NONE', #49790, #42643, #23150 ) ;
#32001 = ORIENTED_EDGE ( 'NONE', *, *, #43679, .T. ) ;
#32002 = VECTOR ( 'NONE', #37503, 1000.000000000000000 ) ;
#32003 = CARTESIAN_POINT ( 'NONE',  ( -207.2473046169136808, 159.2880105690400399, 23.74256005001722158 ) ) ;
#32004 = VERTEX_POINT ( 'NONE', #4465 ) ;
#32005 = CARTESIAN_POINT ( 'NONE',  ( -7.721099712662037540, -1.750000000000023537, -120.2068387089191219 ) ) ;
#32006 = LINE ( 'NONE', #29158, #34703 ) ;
#32007 = AXIS2_PLACEMENT_3D ( 'NONE', #32033, #47624, #28178 ) ;
#32008 = DIRECTION ( 'NONE',  ( -1.000000000000000000, -0.000000000000000000, -0.000000000000000000 ) ) ;
#32009 = AXIS2_PLACEMENT_3D ( 'NONE', #29496, #37227, #17927 ) ;
#32010 = ORIENTED_EDGE ( 'NONE', *, *, #17428, .T. ) ;
#32011 = CARTESIAN_POINT ( 'NONE',  ( 194.3291528190321742, 1.750000000000010214, -118.1565861772249519 ) ) ;
#32012 = ORIENTED_EDGE ( 'NONE', *, *, #17830, .F. ) ;
#32013 = ORIENTED_EDGE ( 'NONE', *, *, #24672, .T. ) ;
#32014 = CARTESIAN_POINT ( 'NONE',  ( -8.445973446814962315, 1.025126265847096763, -157.4317124430720014 ) ) ;
#32015 = DIRECTION ( 'NONE',  ( -0.000000000000000000, -0.000000000000000000, -1.000000000000000000 ) ) ;
#32016 = ORIENTED_EDGE ( 'NONE', *, *, #27218, .F. ) ;
#32017 = DIRECTION ( 'NONE',  ( 0.000000000000000000, 0.000000000000000000, 1.000000000000000000 ) ) ;
#32018 = DIRECTION ( 'NONE',  ( -1.000000000000000000, 0.000000000000000000, 0.000000000000000000 ) ) ;
#32019 = VERTEX_POINT ( 'NONE', #43956 ) ;
#32020 = FACE_OUTER_BOUND ( 'NONE', #14110, .T. ) ;
#32021 = ORIENTED_EDGE ( 'NONE', *, *, #5123, .T. ) ;
#32022 = EDGE_CURVE ( 'NONE', #29885, #8231, #44685, .T. ) ;
#32023 = DIRECTION ( 'NONE',  ( 0.000000000000000000, 0.000000000000000000, 1.000000000000000000 ) ) ;
#32024 = CARTESIAN_POINT ( 'NONE',  ( 344.0000000000000000, -165.0000000000001137, -94.00000000000019895 ) ) ;
#32025 = DIRECTION ( 'NONE',  ( -1.000000000000000000, -0.000000000000000000, -0.000000000000000000 ) ) ;
#32026 =( BOUNDED_CURVE ( )  B_SPLINE_CURVE ( 3, ( #32511, #25051, #40189, #33009 ),
 .UNSPECIFIED., .F., .F. ) 
 B_SPLINE_CURVE_WITH_KNOTS ( ( 4, 4 ),
 ( 0.000000000000000000, 1.570796326794896558 ),
 .UNSPECIFIED. ) 
 CURVE ( )  GEOMETRIC_REPRESENTATION_ITEM ( )  RATIONAL_B_SPLINE_CURVE ( ( 1.000000000000000000, 0.8047378541243649375, 0.8047378541243649375, 1.000000000000000000 ) ) 
 REPRESENTATION_ITEM ( '' )  );
#32027 = ORIENTED_EDGE ( 'NONE', *, *, #41067, .F. ) ;
#32028 = FACE_OUTER_BOUND ( 'NONE', #42561, .T. ) ;
#32029 = DIRECTION ( 'NONE',  ( 0.000000000000000000, 0.000000000000000000, -1.000000000000000000 ) ) ;
#32030 = ORIENTED_EDGE ( 'NONE', *, *, #37769, .F. ) ;
#32031 = ORIENTED_EDGE ( 'NONE', *, *, #41987, .T. ) ;
#32032 = ORIENTED_EDGE ( 'NONE', *, *, #49021, .F. ) ;
#32033 = CARTESIAN_POINT ( 'NONE',  ( 168.9999999999999716, -272.5000000000000000, -110.9999999999999005 ) ) ;
#32034 =( BOUNDED_CURVE ( )  B_SPLINE_CURVE ( 3, ( #30536, #26690, #45139, #21565 ),
 .UNSPECIFIED., .F., .F. ) 
 B_SPLINE_CURVE_WITH_KNOTS ( ( 4, 4 ),
 ( 0.000000000000000000, 1.570796326794896558 ),
 .UNSPECIFIED. ) 
 CURVE ( )  GEOMETRIC_REPRESENTATION_ITEM ( )  RATIONAL_B_SPLINE_CURVE ( ( 1.000000000000000000, 0.8047378541243649375, 0.8047378541243649375, 1.000000000000000000 ) ) 
 REPRESENTATION_ITEM ( '' )  );
#32035 = DIRECTION ( 'NONE',  ( -0.000000000000000000, 1.000000000000000000, 0.000000000000000000 ) ) ;
#32036 = ORIENTED_EDGE ( 'NONE', *, *, #23253, .F. ) ;
#32037 = VECTOR ( 'NONE', #9904, 1000.000000000000000 ) ;
#32038 = CYLINDRICAL_SURFACE ( 'NONE', #47868, 1.750000000000008438 ) ;
#32039 = DIRECTION ( 'NONE',  ( -0.000000000000000000, -0.000000000000000000, -1.000000000000000000 ) ) ;
#32040 = DIRECTION ( 'NONE',  ( 0.000000000000000000, -1.000000000000000000, 0.000000000000000000 ) ) ;
#32041 = VECTOR ( 'NONE', #12675, 1000.000000000000000 ) ;
#32042 = CARTESIAN_POINT ( 'NONE',  ( -125.6708471809678542, 1.749999999999996891, 81.84341382277506227 ) ) ;
#32043 = DIRECTION ( 'NONE',  ( -1.000000000000000000, -0.000000000000000000, -0.000000000000000000 ) ) ;
#32044 = DIRECTION ( 'NONE',  ( 1.000000000000000000, 0.000000000000000000, 0.000000000000000000 ) ) ;
#32045 = CARTESIAN_POINT ( 'NONE',  ( 166.9999999999999716, -184.9999999999999716, -356.0000000000014211 ) ) ;
#32046 = CARTESIAN_POINT ( 'NONE',  ( 85.00000000000213163, 17.00000000000000000, 95.00000000000000000 ) ) ;
#32047 = CARTESIAN_POINT ( 'NONE',  ( -64.99999999999909051, 17.00000000000000000, -24.99999999999999289 ) ) ;
#32048 = VECTOR ( 'NONE', #26615, 1000.000000000000000 ) ;
#32049 = CARTESIAN_POINT ( 'NONE',  ( 15.00099850811936264, 7.462898891544210933, 9.403735324607438884 ) ) ;
#32050 = FACE_OUTER_BOUND ( 'NONE', #22046, .T. ) ;
#32051 = LINE ( 'NONE', #997, #35593 ) ;
#32052 = CYLINDRICAL_SURFACE ( 'NONE', #18268, 4.000000000000003553 ) ;
#32053 = ORIENTED_EDGE ( 'NONE', *, *, #38424, .F. ) ;
#32054 = EDGE_CURVE ( 'NONE', #37949, #34748, #32946, .T. ) ;
#32055 = DIRECTION ( 'NONE',  ( -0.9510565162951566398, 0.3090169943749383474, 0.000000000000000000 ) ) ;
#32056 = DIRECTION ( 'NONE',  ( 1.000000000000000000, 0.000000000000000000, 0.000000000000000000 ) ) ;
#32057 = DIRECTION ( 'NONE',  ( 1.156482317317870492E-16, -1.000000000000000000, -0.000000000000000000 ) ) ;
#32058 = CARTESIAN_POINT ( 'NONE',  ( -33.86622497129646092, 3.037805405905158462, 7.906207997025717304 ) ) ;
#32059 = ORIENTED_EDGE ( 'NONE', *, *, #35406, .T. ) ;
#32060 = CARTESIAN_POINT ( 'NONE',  ( -42.99990394833793061, 47.95759300784327905, 5.000000000000000000 ) ) ;
#32061 = VERTEX_POINT ( 'NONE', #36036 ) ;
#32062 = CARTESIAN_POINT ( 'NONE',  ( -33.14391172085786508, -37.72293746533094350, -8.016098858316205167 ) ) ;
#32063 = CARTESIAN_POINT ( 'NONE',  ( 0.6215990105956902267, -1.608617984725389860, 9.928159647716132241 ) ) ;
#32064 = DIRECTION ( 'NONE',  ( 1.000000000000000000, 0.000000000000000000, 0.000000000000000000 ) ) ;
#32065 = ORIENTED_EDGE ( 'NONE', *, *, #24379, .F. ) ;
#32066 = CARTESIAN_POINT ( 'NONE',  ( 73.30402655318508209, 0.000000000000000000, 165.0000000000000000 ) ) ;
#32067 = ORIENTED_EDGE ( 'NONE', *, *, #3297, .T. ) ;
#32068 = ORIENTED_EDGE ( 'NONE', *, *, #23288, .T. ) ;
#32069 = VECTOR ( 'NONE', #42148, 1000.000000000000000 ) ;
#32070 = EDGE_LOOP ( 'NONE', ( #45576, #32853, #18274, #12357, #1330, #33905 ) ) ;
#32071 = CARTESIAN_POINT ( 'NONE',  ( -14.99999999999812594, 17.00000000000000000, 90.00000000000000000 ) ) ;
#32072 = CARTESIAN_POINT ( 'NONE',  ( -204.9459734468148895, 1.025126265847089879, 122.5682875569280128 ) ) ;
#32073 = EDGE_LOOP ( 'NONE', ( #47583, #16653, #22939, #13112 ) ) ;
#32074 = FACE_BOUND ( 'NONE', #9762, .T. ) ;
#32075 = CARTESIAN_POINT ( 'NONE',  ( -1.270883027774187379, -0.2878889193224725696, 9.961922210043276493 ) ) ;
#32076 = VECTOR ( 'NONE', #26359, 1000.000000000000000 ) ;
#32077 = LINE ( 'NONE', #27966, #346 ) ;
#32078 = VECTOR ( 'NONE', #579, 1000.000000000000000 ) ;
#32079 = CARTESIAN_POINT ( 'NONE',  ( -168.4459734468149747, -1.025126265847089213, 159.0682875569279418 ) ) ;
#32080 = VERTEX_POINT ( 'NONE', #378 ) ;
#32081 = CARTESIAN_POINT ( 'NONE',  ( 356.0000000000000000, -169.0000000000001137, -349.9999999999999432 ) ) ;
#32082 = ORIENTED_EDGE ( 'NONE', *, *, #25309, .F. ) ;
#32083 = CARTESIAN_POINT ( 'NONE',  ( 181.0000000000000568, 175.0000000000000284, 355.9999999999998863 ) ) ;
#32084 = LINE ( 'NONE', #3863, #39260 ) ;
#32085 = ORIENTED_EDGE ( 'NONE', *, *, #33841, .T. ) ;
#32086 = FACE_OUTER_BOUND ( 'NONE', #36018, .T. ) ;
#32087 = FACE_OUTER_BOUND ( 'NONE', #22088, .T. ) ;
#32088 = ORIENTED_EDGE ( 'NONE', *, *, #11171, .T. ) ;
#32089 = DIRECTION ( 'NONE',  ( -1.000000000000000000, -0.000000000000000000, -0.000000000000000000 ) ) ;
#32090 = FACE_OUTER_BOUND ( 'NONE', #26786, .T. ) ;
#32091 = DIRECTION ( 'NONE',  ( 1.000000000000000000, 0.000000000000000000, 0.000000000000000000 ) ) ;
#32092 = DIRECTION ( 'NONE',  ( -1.110223024625156171E-16, 0.7071067811865474617, -0.7071067811865474617 ) ) ;
#32093 = ORIENTED_EDGE ( 'NONE', *, *, #43417, .F. ) ;
#32094 = DIRECTION ( 'NONE',  ( -1.000000000000000000, -0.000000000000000000, -0.000000000000000000 ) ) ;
#32095 = DIRECTION ( 'NONE',  ( 0.000000000000000000, 2.265761274745217480E-16, -1.000000000000000000 ) ) ;
#32096 = CIRCLE ( 'NONE', #1766, 2.000000000000001776 ) ;
#32097 = LINE ( 'NONE', #16195, #37128 ) ;
#32098 = VERTEX_POINT ( 'NONE', #12657 ) ;
#32099 = ORIENTED_EDGE ( 'NONE', *, *, #12346, .T. ) ;
#32100 = PRODUCT_CONTEXT ( 'NONE', #23656, 'mechanical' ) ;
#32101 = DIRECTION ( 'NONE',  ( 1.000000000000000000, -3.172065745548403743E-16, 1.587271980518778491E-16 ) ) ;
#32102 = LINE ( 'NONE', #48456, #19279 ) ;
#32103 = EDGE_CURVE ( 'NONE', #49222, #36524, #31823, .T. ) ;
#32104 = AXIS2_PLACEMENT_3D ( 'NONE', #23195, #43955, #24227 ) ;
#32105 = DIRECTION ( 'NONE',  ( -4.758098676964957447E-16, -1.000000000000000000, 7.143884938411937192E-48 ) ) ;
#32106 = DIRECTION ( 'NONE',  ( 1.000000000000000000, 0.000000000000000000, 0.000000000000000000 ) ) ;
#32107 = ORIENTED_EDGE ( 'NONE', *, *, #47123, .F. ) ;
#32108 = DIRECTION ( 'NONE',  ( -1.000000000000000000, 0.000000000000000000, 0.000000000000000000 ) ) ;
#32109 = EDGE_CURVE ( 'NONE', #46256, #16880, #7262, .T. ) ;
#32111 = VECTOR ( 'NONE', #46076, 1000.000000000000000 ) ;
#32110 = CARTESIAN_POINT ( 'NONE',  ( 340.0000000000000568, 177.9999999999999432, -3.000000000000003109 ) ) ;
#32112 = FACE_OUTER_BOUND ( 'NONE', #31241, .T. ) ;
#32113 = EDGE_CURVE ( 'NONE', #45606, #11106, #12168, .T. ) ;
#32114 = CARTESIAN_POINT ( 'NONE',  ( 155.0540265531850537, -1.025126265847089657, -80.93171244307201562 ) ) ;
#32115 = ADVANCED_FACE ( 'NONE', ( #8326 ), #31935, .F. ) ;
#32116 = ORIENTED_EDGE ( 'NONE', *, *, #36979, .F. ) ;
#32117 = CYLINDRICAL_SURFACE ( 'NONE', #13328, 37.50000000000000000 ) ;
#32118 = ORIENTED_EDGE ( 'NONE', *, *, #36048, .T. ) ;
#32119 = CARTESIAN_POINT ( 'NONE',  ( 27.73884755486784570, -25.23502201956245017, 7.697694107796188234 ) ) ;
#32120 = EDGE_LOOP ( 'NONE', ( #24516, #39514, #37961, #37220, #33160, #43374 ) ) ;
#32121 = DIRECTION ( 'NONE',  ( 0.000000000000000000, -1.000000000000000000, 0.000000000000000000 ) ) ;
#32122 = DIRECTION ( 'NONE',  ( 0.000000000000000000, 0.000000000000000000, -1.000000000000000000 ) ) ;
#32123 = PLANE ( 'NONE',  #17339 ) ;
#32124 = VERTEX_POINT ( 'NONE', #35801 ) ;
#32125 = DIRECTION ( 'NONE',  ( 1.000000000000000000, 0.000000000000000000, 0.000000000000000000 ) ) ;
#32126 = CARTESIAN_POINT ( 'NONE',  ( -164.9999999999997442, 16.00000000000000000, -60.00000000000000000 ) ) ;
#32127 = ORIENTED_EDGE ( 'NONE', *, *, #34840, .T. ) ;
#32128 = CARTESIAN_POINT ( 'NONE',  ( 181.0000000000000000, -272.4999999999999432, -359.9999999999999432 ) ) ;
#32129 = DIRECTION ( 'NONE',  ( -1.000000000000000000, 4.105366553918459587E-48, 1.586032880504786307E-16 ) ) ;
#32130 = CARTESIAN_POINT ( 'NONE',  ( 1.553222296440332606, -1.431397764604065204, 9.884520316594379352 ) ) ;
#32131 = DIRECTION ( 'NONE',  ( 1.000000000000000000, 0.000000000000000000, 0.000000000000000000 ) ) ;
#32132 = AXIS2_PLACEMENT_3D ( 'NONE', #31537, #35143, #727 ) ;
#32133 = ORIENTED_EDGE ( 'NONE', *, *, #5778, .T. ) ;
#32135 = ORIENTED_EDGE ( 'NONE', *, *, #19643, .F. ) ;
#32134 = ADVANCED_FACE ( 'NONE', ( #4962 ), #27820, .F. ) ;
#32136 = DIRECTION ( 'NONE',  ( 8.673617379884028076E-17, -1.000000000000000000, -0.000000000000000000 ) ) ;
#32137 = ADVANCED_FACE ( 'NONE', ( #628 ), #12909, .F. ) ;
#32138 = CIRCLE ( 'NONE', #1127, 4.000000000000003553 ) ;
#32139 = ADVANCED_FACE ( 'NONE', ( #43459 ), #31686, .F. ) ;
#32140 = ADVANCED_FACE ( 'NONE', ( #36551 ), #17020, .T. ) ;
#32141 = ORIENTED_EDGE ( 'NONE', *, *, #42134, .F. ) ;
#32142 = VECTOR ( 'NONE', #43979, 1000.000000000000000 ) ;
#32143 = FACE_OUTER_BOUND ( 'NONE', #13200, .T. ) ;
#32144 = CARTESIAN_POINT ( 'NONE',  ( -4.999999999999997335, 204.9999999999999716, -234.7500000000000000 ) ) ;
#32145 = LINE ( 'NONE', #47739, #23173 ) ;
#32146 = ORIENTED_EDGE ( 'NONE', *, *, #41556, .T. ) ;
#32147 = LINE ( 'NONE', #40103, #22099 ) ;
#32148 = EDGE_CURVE ( 'NONE', #13512, #38070, #46665, .T. ) ;
#32149 = EDGE_CURVE ( 'NONE', #29100, #14588, #36296, .T. ) ;
#32150 = DIRECTION ( 'NONE',  ( 0.000000000000000000, 0.000000000000000000, 1.000000000000000000 ) ) ;
#32151 = CARTESIAN_POINT ( 'NONE',  ( -4.672045878990125800, 50.00000000000000711, 1.847720168420772691 ) ) ;
#32152 = EDGE_LOOP ( 'NONE', ( #33334, #20696, #3403, #16312, #49646, #28236 ) ) ;
#32153 = ORIENTED_EDGE ( 'NONE', *, *, #1092, .F. ) ;
#32154 = ORIENTED_EDGE ( 'NONE', *, *, #11449, .F. ) ;
#32155 = CARTESIAN_POINT ( 'NONE',  ( 169.0000000000000000, -174.9999999999999716, -115.0000000000001563 ) ) ;
#32156 = CARTESIAN_POINT ( 'NONE',  ( 0.000000000000000000, 175.0000000000000284, 353.7500000000001705 ) ) ;
#32157 = DIRECTION ( 'NONE',  ( 0.1191452206184309831, 0.000000000000000000, -0.9928768384869219865 ) ) ;
#32158 = AXIS2_PLACEMENT_3D ( 'NONE', #20647, #8604, #28853 ) ;
#32159 = ORIENTED_EDGE ( 'NONE', *, *, #5675, .T. ) ;
#32160 = CARTESIAN_POINT ( 'NONE',  ( 115.0540265531850395, 1.025126265847081219, 162.5682875569279133 ) ) ;
#32161 = ORIENTED_EDGE ( 'NONE', *, *, #37188, .F. ) ;
#32162 = EDGE_CURVE ( 'NONE', #49488, #609, #15435, .T. ) ;
#32163 = CARTESIAN_POINT ( 'NONE',  ( 342.0000000000000000, 165.0000000000000000, -94.00000000000019895 ) ) ;
#32164 = ORIENTED_EDGE ( 'NONE', *, *, #47432, .T. ) ;
#32165 =( LENGTH_UNIT ( ) NAMED_UNIT ( * ) SI_UNIT ( .MILLI., .METRE. ) );
#32166 =( BOUNDED_CURVE ( )  B_SPLINE_CURVE ( 3, ( #12031, #488, #27931, #28188 ),
 .UNSPECIFIED., .F., .F. ) 
 B_SPLINE_CURVE_WITH_KNOTS ( ( 4, 4 ),
 ( 4.712388980384689674, 6.283185307179586232 ),
 .UNSPECIFIED. ) 
 CURVE ( )  GEOMETRIC_REPRESENTATION_ITEM ( )  RATIONAL_B_SPLINE_CURVE ( ( 1.000000000000000000, 0.8047378541243649375, 0.8047378541243649375, 1.000000000000000000 ) ) 
 REPRESENTATION_ITEM ( '' )  );
#32167 = DIRECTION ( 'NONE',  ( 0.5038710255240862468, 0.000000000000000000, 0.8637789008984334549 ) ) ;
#32168 = CARTESIAN_POINT ( 'NONE',  ( 85.00000000000152056, 16.00000000000000000, 35.00000000000000000 ) ) ;
#32169 = CARTESIAN_POINT ( 'NONE',  ( 152.2789002873379900, -1.750000000000009548, 39.79316129108089228 ) ) ;
#32170 = EDGE_CURVE ( 'NONE', #25384, #40502, #29619, .T. ) ;
#32171 = ADVANCED_FACE ( 'NONE', ( #16023 ), #49277, .F. ) ;
#32172 = CARTESIAN_POINT ( 'NONE',  ( 29.99999999999998579, 17.00000000000000000, -114.9999999999999858 ) ) ;
#32173 = LINE ( 'NONE', #9071, #15142 ) ;
#32174 = VECTOR ( 'NONE', #40174, 1000.000000000000000 ) ;
#32175 = CARTESIAN_POINT ( 'NONE',  ( 8.277096487746778308, -50.00000000000000711, 7.455576670931136185 ) ) ;
#32176 = VERTEX_POINT ( 'NONE', #9814 ) ;
#32177 = CYLINDRICAL_SURFACE ( 'NONE', #9969, 1.750000000000001554 ) ;
#32178 = VECTOR ( 'NONE', #7935, 999.9999999999998863 ) ;
#32179 = DIRECTION ( 'NONE',  ( 1.333906992743555050E-23, -1.000000000000000000, 0.000000000000000000 ) ) ;
#32180 = FACE_OUTER_BOUND ( 'NONE', #8505, .T. ) ;
#32181 = AXIS2_PLACEMENT_3D ( 'NONE', #19796, #47465, #44144 ) ;
#32182 = VECTOR ( 'NONE', #9320, 1000.000000000000000 ) ;
#32183 = CARTESIAN_POINT ( 'NONE',  ( 356.0000000000000000, 165.0000000000001705, -340.0000000000002842 ) ) ;
#32184 = VERTEX_POINT ( 'NONE', #29331 ) ;
#32185 = EDGE_CURVE ( 'NONE', #5052, #29935, #45445, .T. ) ;
#32186 = DIRECTION ( 'NONE',  ( -0.000000000000000000, -0.000000000000000000, -1.000000000000000000 ) ) ;
#32187 =( BOUNDED_CURVE ( )  B_SPLINE_CURVE ( 3, ( #32495, #32998, #17578, #1439 ),
 .UNSPECIFIED., .F., .F. ) 
 B_SPLINE_CURVE_WITH_KNOTS ( ( 4, 4 ),
 ( 4.712388980384689674, 6.283185307179586232 ),
 .UNSPECIFIED. ) 
 CURVE ( )  GEOMETRIC_REPRESENTATION_ITEM ( )  RATIONAL_B_SPLINE_CURVE ( ( 1.000000000000000000, 0.8047378541243649375, 0.8047378541243649375, 1.000000000000000000 ) ) 
 REPRESENTATION_ITEM ( '' )  );
#32188 = LINE ( 'NONE', #36304, #48425 ) ;
#32189 = VERTEX_POINT ( 'NONE', #14161 ) ;
#32190 = DIRECTION ( 'NONE',  ( 1.860490536778032451E-50, 0.000000000000000000, -1.000000000000000000 ) ) ;
#32191 = CARTESIAN_POINT ( 'NONE',  ( 3.940019464150765760, 50.00000000000000711, -8.466730184410787174 ) ) ;
#32192 = EDGE_CURVE ( 'NONE', #23358, #40073, #30093, .T. ) ;
#32193 = CARTESIAN_POINT ( 'NONE',  ( 356.0000000000006253, 167.0000000000000000, -342.0000000000001137 ) ) ;
#32194 = LINE ( 'NONE', #8839, #41403 ) ;
#32195 = AXIS2_PLACEMENT_3D ( 'NONE', #25191, #9290, #2339 ) ;
#32196 = ORIENTED_EDGE ( 'NONE', *, *, #29635, .F. ) ;
#32197 = VERTEX_POINT ( 'NONE', #41629 ) ;
#32198 = FACE_OUTER_BOUND ( 'NONE', #37396, .T. ) ;
#32199 = CARTESIAN_POINT ( 'NONE',  ( 15.45175104485250728, -6.222373774239001065, -2.870787844569587133 ) ) ;
#32200 = EDGE_CURVE ( 'NONE', #24673, #35472, #45694, .T. ) ;
#32201 = EDGE_CURVE ( 'NONE', #30616, #10238, #21988, .T. ) ;
#32202 = ORIENTED_EDGE ( 'NONE', *, *, #46931, .T. ) ;
#32203 = ORIENTED_EDGE ( 'NONE', *, *, #19358, .T. ) ;
#32204 = CARTESIAN_POINT ( 'NONE',  ( 181.0000000000000284, -168.9999999999999432, -115.0000000000001847 ) ) ;
#32205 = CYLINDRICAL_SURFACE ( 'NONE', #11872, 1.750000000000015543 ) ;
#32206 = LINE ( 'NONE', #43981, #27539 ) ;
#32207 = DIRECTION ( 'NONE',  ( -1.000000000000000000, -0.000000000000000000, -0.000000000000000000 ) ) ;
#32208 = APPLICATION_CONTEXT ( 'automotive_design' ) ;
#32209 = VERTEX_POINT ( 'NONE', #6475 ) ;
#32210 = ORIENTED_EDGE ( 'NONE', *, *, #39039, .T. ) ;
#32211 = AXIS2_PLACEMENT_3D ( 'NONE', #41803, #38731, #15378 ) ;
#32212 = ORIENTED_EDGE ( 'NONE', *, *, #10456, .F. ) ;
#32213 = EDGE_CURVE ( 'NONE', #49071, #8841, #25738, .T. ) ;
#32214=STYLED_ITEM('',(#50747),#39303);
#32215 = EDGE_CURVE ( 'NONE', #43597, #35332, #1463, .T. ) ;
#32216 = CARTESIAN_POINT ( 'NONE',  ( -208.1473046169136580, 159.2880105690400399, 472.6625600500173050 ) ) ;
#32217 = AXIS2_PLACEMENT_3D ( 'NONE', #43075, #21181, #5530 ) ;
#32218 = CARTESIAN_POINT ( 'NONE',  ( -204.9459734468148895, 1.025126265847089435, 162.5682875569279133 ) ) ;
#32219 = VERTEX_POINT ( 'NONE', #26237 ) ;
#32220 = ORIENTED_EDGE ( 'NONE', *, *, #6429, .F. ) ;
#32221 = CARTESIAN_POINT ( 'NONE',  ( -7.721099712662037540, -1.750000000000022871, -160.2068387089191219 ) ) ;
#32222 = CARTESIAN_POINT ( 'NONE',  ( 2.569099690548740877, -50.00000000000000711, 3.199614146704519602 ) ) ;
#32223 = EDGE_CURVE ( 'NONE', #22898, #18727, #9711, .T. ) ;
#32224 = DIRECTION ( 'NONE',  ( -1.000000000000000000, -0.000000000000000000, -0.000000000000000000 ) ) ;
#32225 = ORIENTED_EDGE ( 'NONE', *, *, #8457, .F. ) ;
#32226 = VERTEX_POINT ( 'NONE', #5715 ) ;
#32227 = CARTESIAN_POINT ( 'NONE',  ( 1.377551617740986334, -0.6025367262284159198, 9.936141075690080982 ) ) ;
#32228 = DIRECTION ( 'NONE',  ( 0.000000000000000000, 0.000000000000000000, 1.000000000000000000 ) ) ;
#32229 = ORIENTED_EDGE ( 'NONE', *, *, #46847, .F. ) ;
#32230 = CARTESIAN_POINT ( 'NONE',  ( -14.49999999999999822, 12.87566193687862715, 19.86060803177194600 ) ) ;
#32231 = DIRECTION ( 'NONE',  ( -0.000000000000000000, -1.000000000000000000, -0.000000000000000000 ) ) ;
#32232 = CARTESIAN_POINT ( 'NONE',  ( -2.210477865340801706, -37.43479381012853224, -9.422646554964178023 ) ) ;
#32233 = ADVANCED_FACE ( 'NONE', ( #5467, #33446 ), #2133, .F. ) ;
#32234 = CARTESIAN_POINT ( 'NONE',  ( 181.0000000000000568, -164.9999999999999432, 341.9999999999998863 ) ) ;
#32235 = ORIENTED_EDGE ( 'NONE', *, *, #33450, .F. ) ;
#32236 = CARTESIAN_POINT ( 'NONE',  ( -15.62858259096117841, 5.755205073598721910, -9.683996418299976483 ) ) ;
#32237 = CARTESIAN_POINT ( 'NONE',  ( 46.76852358249013975, -17.86468378716709537, -9.367992836599954742 ) ) ;
#32238 = B_SPLINE_CURVE_WITH_KNOTS ( 'NONE', 3,
 ( #27096, #4503, #34815, #27862 ),
 .UNSPECIFIED., .F., .F.,
 ( 4, 4 ),
 ( 0.000000000000000000, 0.0002610106747149790337 ),
 .UNSPECIFIED. ) ;
#32239 = DIRECTION ( 'NONE',  ( 0.000000000000000000, 0.000000000000000000, 1.000000000000000000 ) ) ;
#32240 = CARTESIAN_POINT ( 'NONE',  ( -14.49999999999999822, -46.01315789473684248, -6.315789473684215949 ) ) ;
#32241 = CIRCLE ( 'NONE', #21563, 0.5000000000000004441 ) ;
#32242 = CARTESIAN_POINT ( 'NONE',  ( -46.69597344681494633, -1.750000000000010658, -79.18171244307201562 ) ) ;
#32243 = VECTOR ( 'NONE', #27634, 1000.000000000000000 ) ;
#32244 = CARTESIAN_POINT ( 'NONE',  ( -1.531049279420139131, -0.4659387722959919542, 9.919954280166518146 ) ) ;
#32245 = CARTESIAN_POINT ( 'NONE',  ( 151.5540265531850537, 0.000000000000000000, 39.06828755692798438 ) ) ;
#32246 =( GEOMETRIC_REPRESENTATION_CONTEXT ( 3 ) GLOBAL_UNCERTAINTY_ASSIGNED_CONTEXT ( ( #11619 ) ) GLOBAL_UNIT_ASSIGNED_CONTEXT ( ( #8724, #35925, #20752 ) ) REPRESENTATION_CONTEXT ( 'NONE', 'WORKASPACE' ) );
#32247 = ORIENTED_EDGE ( 'NONE', *, *, #11521, .T. ) ;
#32248 = CARTESIAN_POINT ( 'NONE',  ( 22.90865447854256232, 29.73489050103220777, -2.490396854064190979 ) ) ;
#32249 = VECTOR ( 'NONE', #11280, 1000.000000000000000 ) ;
#32250 = FACE_OUTER_BOUND ( 'NONE', #34030, .T. ) ;
#32251 = ORIENTED_EDGE ( 'NONE', *, *, #2005, .F. ) ;
#32252 = CARTESIAN_POINT ( 'NONE',  ( -128.4459734468149179, 0.000000000000000000, 2.568287556927950632 ) ) ;
#32253 = FACE_OUTER_BOUND ( 'NONE', #23590, .T. ) ;
#32254 = CARTESIAN_POINT ( 'NONE',  ( 210.0000000000000568, 0.000000000000000000, 120.8182875569279702 ) ) ;
#32255 = ORIENTED_EDGE ( 'NONE', *, *, #39947, .T. ) ;
#32256 = CARTESIAN_POINT ( 'NONE',  ( -165.6708471809677974, -1.750000000000009548, -40.20683870891912193 ) ) ;
#32257 = B_SPLINE_SURFACE_WITH_KNOTS ( 'NONE', 3, 3, ( 
 ( #24627, #5105, #32587, #40526 ),
 ( #5364, #1530, #23221, #15293 ),
 ( #35313, #38390, #14770, #22469 ),
 ( #23496, #46785, #149, #11430 ) ),
 .UNSPECIFIED., .F., .F., .F.,
 ( 4, 4 ),
 ( 4, 4 ),
 ( 0.000000000000000000, 1.000000000000000000 ),
 ( 0.000000000000000000, 1.000000000000000000 ),
 .UNSPECIFIED. ) ;
#32258 = ORIENTED_EDGE ( 'NONE', *, *, #9110, .T. ) ;
#32259 = VERTEX_POINT ( 'NONE', #36799 ) ;
#32260 = CARTESIAN_POINT ( 'NONE',  ( -0.3978397141392489011, 0.1292659590674825332, 9.992713367193012175 ) ) ;
#32261 = CARTESIAN_POINT ( 'NONE',  ( -46.69597344681494633, 0.000000000000000000, 165.0000000000000000 ) ) ;
#32262 = ADVANCED_FACE ( 'NONE', ( #13906 ), #21366, .T. ) ;
#32263 = VECTOR ( 'NONE', #19895, 1000.000000000000000 ) ;
#32264 = EDGE_CURVE ( 'NONE', #19656, #6992, #29574, .T. ) ;
#32265 = EDGE_LOOP ( 'NONE', ( #15764, #49187, #179, #19709, #14924, #39851 ) ) ;
#32266 = DIRECTION ( 'NONE',  ( -1.000000000000000000, -0.000000000000000000, -0.000000000000000000 ) ) ;
#32267 = LINE ( 'NONE', #40467, #33126 ) ;
#32268 =( BOUNDED_CURVE ( )  B_SPLINE_CURVE ( 3, ( #37438, #41255, #10216, #25618 ),
 .UNSPECIFIED., .F., .F. ) 
 B_SPLINE_CURVE_WITH_KNOTS ( ( 4, 4 ),
 ( 1.570796326794896558, 3.141592653589793116 ),
 .UNSPECIFIED. ) 
 CURVE ( )  GEOMETRIC_REPRESENTATION_ITEM ( )  RATIONAL_B_SPLINE_CURVE ( ( 1.000000000000000000, 0.8047378541243649375, 0.8047378541243649375, 1.000000000000000000 ) ) 
 REPRESENTATION_ITEM ( '' )  );
#32269 = ORIENTED_EDGE ( 'NONE', *, *, #745, .F. ) ;
#32270 = ADVANCED_FACE ( 'NONE', ( #6237 ), #48525, .F. ) ;
#32271 = B_SPLINE_CURVE_WITH_KNOTS ( 'NONE', 3,
 ( #35735, #15955, #38808, #35973, #4153, #4662 ),
 .UNSPECIFIED., .F., .F.,
 ( 4, 2, 4 ),
 ( 4.635316164197443437E-17, 0.009882509389272372408, 0.01976501877854469624 ),
 .UNSPECIFIED. ) ;
#32272 = CARTESIAN_POINT ( 'NONE',  ( 210.0000000000000568, 0.000000000000000000, 80.81828755692798438 ) ) ;
#32273 = ORIENTED_EDGE ( 'NONE', *, *, #50525, .F. ) ;
#32275 = ADVANCED_FACE ( 'NONE', ( #13673 ), #13412, .T. ) ;
#32274 = CARTESIAN_POINT ( 'NONE',  ( 71.55402655318505367, 1.025126265847089435, 122.5682875569280128 ) ) ;
#32276 = DIRECTION ( 'NONE',  ( -0.4740998230350175202, -0.3386427307392980701, -0.8127425537743157014 ) ) ;
#32277 = EDGE_CURVE ( 'NONE', #26320, #19053, #50099, .T. ) ;
#32278 = LINE ( 'NONE', #12760, #43934 ) ;
#32279 = ORIENTED_EDGE ( 'NONE', *, *, #6126, .T. ) ;
#32280 = PLANE ( 'NONE',  #23506 ) ;
#32281 = DIRECTION ( 'NONE',  ( 0.000000000000000000, 0.000000000000000000, 1.000000000000000000 ) ) ;
#32282 = AXIS2_PLACEMENT_3D ( 'NONE', #12362, #4173, #46975 ) ;
#32283 = VERTEX_POINT ( 'NONE', #37555 ) ;
#32284 = EDGE_LOOP ( 'NONE', ( #50121, #2225, #2859, #4171, #14446, #29304 ) ) ;
#32285 = ORIENTED_EDGE ( 'NONE', *, *, #4630, .F. ) ;
#32286 = DIRECTION ( 'NONE',  ( -0.000000000000000000, -1.000000000000000000, -0.000000000000000000 ) ) ;
#32287 = ADVANCED_FACE ( 'NONE', ( #38560 ), #36371, .T. ) ;
#32288 = VECTOR ( 'NONE', #11016, 1000.000000000000000 ) ;
#32289 = EDGE_CURVE ( 'NONE', #43380, #20901, #57, .T. ) ;
#32290 = CARTESIAN_POINT ( 'NONE',  ( 210.0000000000000568, 2.143131898507881116E-16, -40.93171244307203693 ) ) ;
#32291 = VERTEX_POINT ( 'NONE', #34972 ) ;
#32292 = VECTOR ( 'NONE', #40263, 1000.000000000000000 ) ;
#32293 = DIRECTION ( 'NONE',  ( -0.000000000000000000, -0.000000000000000000, -1.000000000000000000 ) ) ;
#32294 = AXIS2_PLACEMENT_3D ( 'NONE', #33875, #26158, #2799 ) ;
#32295 = CARTESIAN_POINT ( 'NONE',  ( -4.999999999999950262, -197.4999999999999432, -228.6347188485896140 ) ) ;
#32296 = CARTESIAN_POINT ( 'NONE',  ( 432.7825420346616170, -102.8976013127941656, -7.208237214241163926 ) ) ;
#32297 = DIRECTION ( 'NONE',  ( 0.000000000000000000, 0.000000000000000000, 1.000000000000000000 ) ) ;
#32298 = CARTESIAN_POINT ( 'NONE',  ( 36.46533180484010472, 8.777022568848463990, -9.011255500499647297 ) ) ;
#32299 = PLANE ( 'NONE',  #13540 ) ;
#32300 = CARTESIAN_POINT ( 'NONE',  ( 35.05402655318504657, 1.025126265847089657, 119.0682875569279560 ) ) ;
#32301 = CARTESIAN_POINT ( 'NONE',  ( 214.9999999999999432, 173.0000000000000000, 231.9999999999999716 ) ) ;
#32302 = DIRECTION ( 'NONE',  ( -1.000000000000000000, 0.000000000000000000, 0.000000000000000000 ) ) ;
#32303 = UNCERTAINTY_MEASURE_WITH_UNIT (LENGTH_MEASURE( 1.000000000000000082E-05 ), #49817, 'distance_accuracy_value', 'NONE');
#32304 = AXIS2_PLACEMENT_3D ( 'NONE', #5523, #39936, #13473 ) ;
#32305 = CARTESIAN_POINT ( 'NONE',  ( -114.9999999999987779, 16.00000000000000000, 5.000000000000004441 ) ) ;
#32306 = ORIENTED_EDGE ( 'NONE', *, *, #3020, .F. ) ;
#32307 = CARTESIAN_POINT ( 'NONE',  ( 73.30402655318508209, 1.750000000000010214, -39.18171244307202983 ) ) ;
#32308 = EDGE_CURVE ( 'NONE', #48932, #11192, #7755, .T. ) ;
#32309 = CARTESIAN_POINT ( 'NONE',  ( 224.9999999999999432, -175.0000000000000000, 0.000000000000000000 ) ) ;
#32310 = PLANE ( 'NONE',  #50363 ) ;
#32311 = LINE ( 'NONE', #40507, #1710 ) ;
#32312 = ADVANCED_FACE ( 'NONE', ( #46698 ), #34711, .T. ) ;
#32313 = ORIENTED_EDGE ( 'NONE', *, *, #43679, .F. ) ;
#32314 = DIRECTION ( 'NONE',  ( 0.000000000000000000, 0.000000000000000000, 1.000000000000000000 ) ) ;
#32315 = VECTOR ( 'NONE', #8222, 1000.000000000000000 ) ;
#32316 = DIRECTION ( 'NONE',  ( 0.000000000000000000, 0.000000000000000000, -1.000000000000000000 ) ) ;
#32317 = ORIENTED_EDGE ( 'NONE', *, *, #13519, .F. ) ;
#32318 = DIRECTION ( 'NONE',  ( -0.000000000000000000, -1.000000000000000000, -0.000000000000000000 ) ) ;
#32319 = CARTESIAN_POINT ( 'NONE',  ( 73.30402655318508209, -1.750000000000010658, -119.1817124430720440 ) ) ;
#32320 = CARTESIAN_POINT ( 'NONE',  ( -5.647304616913629616, -41.71198943095993172, 741.9425600500172777 ) ) ;
#32321 = ORIENTED_EDGE ( 'NONE', *, *, #32740, .T. ) ;
#32322 = DIRECTION ( 'NONE',  ( -0.000000000000000000, -0.000000000000000000, 1.000000000000000000 ) ) ;
#32323 = ORIENTED_EDGE ( 'NONE', *, *, #29958, .T. ) ;
#32324 = VERTEX_POINT ( 'NONE', #34203 ) ;
#32325 = AXIS2_PLACEMENT_3D ( 'NONE', #29244, #16948, #32602 ) ;
#32326 =( BOUNDED_CURVE ( )  B_SPLINE_CURVE ( 3, ( #2038, #9724, #33598, #40785 ),
 .UNSPECIFIED., .F., .F. ) 
 B_SPLINE_CURVE_WITH_KNOTS ( ( 4, 4 ),
 ( 3.141592653589793560, 4.712388980384689674 ),
 .UNSPECIFIED. ) 
 CURVE ( )  GEOMETRIC_REPRESENTATION_ITEM ( )  RATIONAL_B_SPLINE_CURVE ( ( 1.000000000000000000, 0.8047378541243650485, 0.8047378541243650485, 1.000000000000000000 ) ) 
 REPRESENTATION_ITEM ( '' )  );
#32327 = EDGE_LOOP ( 'NONE', ( #8662, #6502, #29411, #6759 ) ) ;
#32328 = DIRECTION ( 'NONE',  ( 0.000000000000000000, -1.000000000000000000, 0.000000000000000000 ) ) ;
#32329 = EDGE_LOOP ( 'NONE', ( #32146, #22715, #5828, #43626, #9345, #14370 ) ) ;
#32330 = DIRECTION ( 'NONE',  ( -0.000000000000000000, 1.000000000000000000, -0.000000000000000000 ) ) ;
#32331 = CARTESIAN_POINT ( 'NONE',  ( 73.30402655318508209, 0.000000000000000000, 165.0000000000000000 ) ) ;
#32332 = CARTESIAN_POINT ( 'NONE',  ( -0.9600884595229873808, 0.8493647100668667571, 9.957892297621016908 ) ) ;
#32333 =( BOUNDED_CURVE ( )  B_SPLINE_CURVE ( 3, ( #7326, #7849, #38642, #147 ),
 .UNSPECIFIED., .F., .F. ) 
 B_SPLINE_CURVE_WITH_KNOTS ( ( 4, 4 ),
 ( 1.570796326794896558, 3.141592653589793116 ),
 .UNSPECIFIED. ) 
 CURVE ( )  GEOMETRIC_REPRESENTATION_ITEM ( )  RATIONAL_B_SPLINE_CURVE ( ( 1.000000000000000000, 0.8047378541243649375, 0.8047378541243649375, 1.000000000000000000 ) ) 
 REPRESENTATION_ITEM ( '' )  );
#32334 = FACE_OUTER_BOUND ( 'NONE', #14237, .T. ) ;
#32335 = ORIENTED_EDGE ( 'NONE', *, *, #49627, .F. ) ;
#32336 = FACE_OUTER_BOUND ( 'NONE', #46907, .T. ) ;
#32337 = VECTOR ( 'NONE', #7048, 1000.000000000000000 ) ;
#32338 = ORIENTED_EDGE ( 'NONE', *, *, #46294, .F. ) ;
#32339 = CYLINDRICAL_SURFACE ( 'NONE', #22643, 1.750000000000010214 ) ;
#32340 = DIRECTION ( 'NONE',  ( -0.000000000000000000, 0.000000000000000000, 1.000000000000000000 ) ) ;
#32341 = AXIS2_PLACEMENT_3D ( 'NONE', #6028, #21681, #21423 ) ;
#32342 = ORIENTED_EDGE ( 'NONE', *, *, #36928, .T. ) ;
#32343 = DIRECTION ( 'NONE',  ( 1.000000000000000000, 0.000000000000000000, 0.000000000000000000 ) ) ;
#32344 = EDGE_CURVE ( 'NONE', #574, #36127, #41879, .T. ) ;
#32345 = CARTESIAN_POINT ( 'NONE',  ( -175.0000000000000000, 0.000000000000000000, 122.5000000000000142 ) ) ;
#32346 = VERTEX_POINT ( 'NONE', #11853 ) ;
#32347 = DIRECTION ( 'NONE',  ( 0.000000000000000000, 0.000000000000000000, -1.000000000000000000 ) ) ;
#32348 = CARTESIAN_POINT ( 'NONE',  ( -36.08557433729205144, 35.58569447144795816, 7.455576670931136185 ) ) ;
#32349 = CARTESIAN_POINT ( 'NONE',  ( 340.0000000000000568, 185.0000000000000284, 349.9999999999997726 ) ) ;
#32350 = ORIENTED_EDGE ( 'NONE', *, *, #15540, .T. ) ;
#32351 = FACE_OUTER_BOUND ( 'NONE', #15963, .T. ) ;
#32352 = DIRECTION ( 'NONE',  ( 1.000000000000000000, 0.000000000000000000, 0.000000000000000000 ) ) ;
#32353 = CARTESIAN_POINT ( 'NONE',  ( -0.3862712429686977478, 1.188820645368937390, 10.00000000000000000 ) ) ;
#32354 = VERTEX_POINT ( 'NONE', #50283 ) ;
#32355 = CIRCLE ( 'NONE', #41351, 2.000000000000001776 ) ;
#32356 = ORIENTED_EDGE ( 'NONE', *, *, #3795, .T. ) ;
#32357 = CONTEXT_DEPENDENT_SHAPE_REPRESENTATION ( #19755, #22883 ) ;
#32358 = DIRECTION ( 'NONE',  ( 1.587271980518778491E-16, -5.169878828456422968E-26, -1.000000000000000000 ) ) ;
#32359 = LINE ( 'NONE', #35964, #11125 ) ;
#32360 = CARTESIAN_POINT ( 'NONE',  ( -205.6708471809678827, 1.750000000000009548, -40.20683870891912193 ) ) ;
#32361 = CARTESIAN_POINT ( 'NONE',  ( 35.00000000000186162, 17.00000000000000000, 90.00000000000000000 ) ) ;
#32362 = ORIENTED_EDGE ( 'NONE', *, *, #9656, .F. ) ;
#32363 = CARTESIAN_POINT ( 'NONE',  ( 24.39427009665984869, 44.07992421011656603, 8.807470649214879543 ) ) ;
#32364 = CYLINDRICAL_SURFACE ( 'NONE', #7299, 1.750000000000036193 ) ;
#32365 = DIRECTION ( 'NONE',  ( -1.000000000000000000, -0.000000000000000000, -0.000000000000000000 ) ) ;
#32366 = CARTESIAN_POINT ( 'NONE',  ( 193.3040265531851105, 1.750000000000010214, -39.18171244307202983 ) ) ;
#32367 = EDGE_CURVE ( 'NONE', #46904, #33640, #6727, .T. ) ;
#32368 = ORIENTED_EDGE ( 'NONE', *, *, #11414, .T. ) ;
#32369 = VECTOR ( 'NONE', #34583, 1000.000000000000000 ) ;
#32370 = CYLINDRICAL_SURFACE ( 'NONE', #3466, 1.750000000000001554 ) ;
#32371 = ORIENTED_EDGE ( 'NONE', *, *, #8597, .T. ) ;
#32372 = LINE ( 'NONE', #4668, #24520 ) ;
#32373 = AXIS2_PLACEMENT_3D ( 'NONE', #47708, #24422, #12593 ) ;
#32374 = ORIENTED_EDGE ( 'NONE', *, *, #5891, .F. ) ;
#32375 = CARTESIAN_POINT ( 'NONE',  ( -165.0000000000000284, 16.00000000000000000, 115.0000000000000142 ) ) ;
#32376 = CARTESIAN_POINT ( 'NONE',  ( -204.9459734468149463, 2.143131898507880377E-16, -37.43171244307205825 ) ) ;
#32377 = LINE ( 'NONE', #17893, #49229 ) ;
#32378 = ORIENTED_EDGE ( 'NONE', *, *, #27123, .T. ) ;
#32379 = CARTESIAN_POINT ( 'NONE',  ( -6.695973446814940111, 1.750000000000023759, 40.81828755692798438 ) ) ;
#32380 = ORIENTED_EDGE ( 'NONE', *, *, #1054, .T. ) ;
#32381 = LINE ( 'NONE', #13859, #11556 ) ;
#32382 = CARTESIAN_POINT ( 'NONE',  ( 214.9999999999999432, -165.2931214222915628, 497.2965085865001811 ) ) ;
#32383 = CARTESIAN_POINT ( 'NONE',  ( -8.445973446814976526, 0.000000000000000000, 165.0000000000000000 ) ) ;
#32384 = DIRECTION ( 'NONE',  ( -1.000000000000000000, 0.000000000000000000, 0.000000000000000000 ) ) ;
#32385 = ORIENTED_EDGE ( 'NONE', *, *, #17975, .T. ) ;
#32386 =( GEOMETRIC_REPRESENTATION_CONTEXT ( 3 ) GLOBAL_UNCERTAINTY_ASSIGNED_CONTEXT ( ( #7519 ) ) GLOBAL_UNIT_ASSIGNED_CONTEXT ( ( #4712, #13158, #17010 ) ) REPRESENTATION_CONTEXT ( 'NONE', 'WORKASPACE' ) );
#32387 = ORIENTED_EDGE ( 'NONE', *, *, #6489, .T. ) ;
#32388 = DIRECTION ( 'NONE',  ( -1.000000000000000000, -0.000000000000000000, -0.000000000000000000 ) ) ;
#32389 = AXIS2_PLACEMENT_3D ( 'NONE', #33488, #45740, #33246 ) ;
#32390 = ORIENTED_EDGE ( 'NONE', *, *, #23522, .F. ) ;
#32391 = DIRECTION ( 'NONE',  ( 1.000000000000000000, 0.000000000000000000, 0.000000000000000000 ) ) ;
#32392 = DIRECTION ( 'NONE',  ( -0.000000000000000000, -1.000000000000000000, -0.000000000000000000 ) ) ;
#32393 = CYLINDRICAL_SURFACE ( 'NONE', #25596, 1.749999999999973799 ) ;
#32394 = VERTEX_POINT ( 'NONE', #10827 ) ;
#32395 = CYLINDRICAL_SURFACE ( 'NONE', #37683, 2.000000000000001776 ) ;
#32396 = EDGE_CURVE ( 'NONE', #31718, #8840, #27251, .T. ) ;
#32397 = CARTESIAN_POINT ( 'NONE',  ( 85.00000000000056843, 17.00000000000000000, -30.00000000000000000 ) ) ;
#32398 = EDGE_CURVE ( 'NONE', #40766, #25202, #15194, .T. ) ;
#32399 = CARTESIAN_POINT ( 'NONE',  ( -5.647304616913629616, -154.8119894309599260, 23.74256005001722158 ) ) ;
#32400 = CARTESIAN_POINT ( 'NONE',  ( -0.9358216137853901939, 0.9039474357307636376, 9.986087673579197244 ) ) ;
#32401 = PLANE ( 'NONE',  #35630 ) ;
#32402 = EDGE_CURVE ( 'NONE', #42338, #37393, #22375, .T. ) ;
#32403 = CARTESIAN_POINT ( 'NONE',  ( 2.538055338523177440, 50.00000000000000711, -9.367992836599954742 ) ) ;
#32404 = AXIS2_PLACEMENT_3D ( 'NONE', #48482, #13862, #40586 ) ;
#32405 = ORIENTED_EDGE ( 'NONE', *, *, #33096, .T. ) ;
#32406 = ORIENTED_EDGE ( 'NONE', *, *, #36825, .T. ) ;
#32407 = ORIENTED_EDGE ( 'NONE', *, *, #17612, .T. ) ;
#32408 = VECTOR ( 'NONE', #47899, 1000.000000000000000 ) ;
#32409 = LINE ( 'NONE', #12638, #40267 ) ;
#32410 = CARTESIAN_POINT ( 'NONE',  ( 113.3040265531850537, -1.749999999999997335, -119.1817124430720440 ) ) ;
#32411 = EDGE_CURVE ( 'NONE', #50487, #12217, #25088, .T. ) ;
#32412 = CARTESIAN_POINT ( 'NONE',  ( 169.0000000000000000, -174.9999999999999716, -99.00000000000014211 ) ) ;
#32413 = VECTOR ( 'NONE', #13161, 1000.000000000000000 ) ;
#32414 = ADVANCED_FACE ( 'NONE', ( #18522 ), #46448, .T. ) ;
#32415 = CYLINDRICAL_SURFACE ( 'NONE', #42804, 1.750000000000015543 ) ;
#32416 = EDGE_LOOP ( 'NONE', ( #3821, #32600, #26418, #44041 ) ) ;
#32417 = CARTESIAN_POINT ( 'NONE',  ( -166.6959734468149463, 1.750000000000010214, -39.18171244307202983 ) ) ;
#32418 = ORIENTED_EDGE ( 'NONE', *, *, #13987, .F. ) ;
#32419 = EDGE_CURVE ( 'NONE', #34763, #34025, #14678, .T. ) ;
#32420 = CARTESIAN_POINT ( 'NONE',  ( -6.174150299305392053, 33.14591993373988998, 8.807470649214879543 ) ) ;
#32421 = AXIS2_PLACEMENT_3D ( 'NONE', #8821, #16520, #20355 ) ;
#32422 = LINE ( 'NONE', #5708, #33440 ) ;
#32423 = CARTESIAN_POINT ( 'NONE',  ( -45.67084718096785423, 1.750000000000010214, -118.1565861772249519 ) ) ;
#32424 = DIRECTION ( 'NONE',  ( -1.156482317317870492E-16, 1.000000000000000000, 0.000000000000000000 ) ) ;
#32425 = CIRCLE ( 'NONE', #26664, 4.000000000000003553 ) ;
#32426 = DIRECTION ( 'NONE',  ( -1.000000000000000000, -0.000000000000000000, -0.000000000000000000 ) ) ;
#32427 = VECTOR ( 'NONE', #29680, 1000.000000000000000 ) ;
#32428 = LINE ( 'NONE', #8572, #46073 ) ;
#32429 = VERTEX_POINT ( 'NONE', #8256 ) ;
#32430 = DIRECTION ( 'NONE',  ( 0.000000000000000000, -1.000000000000000000, 0.000000000000000000 ) ) ;
#32431 = CARTESIAN_POINT ( 'NONE',  ( -15.00000000000001421, 17.00000000000000000, -114.9999999999999858 ) ) ;
#32432 = DIRECTION ( 'NONE',  ( -1.000000000000000000, 0.000000000000000000, 0.000000000000000000 ) ) ;
#32433 = EDGE_CURVE ( 'NONE', #24770, #37466, #38186, .T. ) ;
#32434 = EDGE_CURVE ( 'NONE', #6557, #17311, #20798, .T. ) ;
#32435 = AXIS2_PLACEMENT_3D ( 'NONE', #9128, #36095, #48582 ) ;
#32436 = ADVANCED_FACE ( 'NONE', ( #23648 ), #31870, .T. ) ;
#32437 = ADVANCED_FACE ( 'NONE', ( #1322 ), #43384, .T. ) ;
#32438 = CARTESIAN_POINT ( 'NONE',  ( -0.3862712429686729343, -1.188820645368946050, 10.00000000000000000 ) ) ;
#32439 = EDGE_LOOP ( 'NONE', ( #11322, #16356, #21541, #1731, #6124, #30105, #17230, #18866 ) ) ;
#32440 = LINE ( 'NONE', #31940, #31939 ) ;
#32441 = ORIENTED_EDGE ( 'NONE', *, *, #31515, .T. ) ;
#32442 = DIRECTION ( 'NONE',  ( 0.000000000000000000, 0.000000000000000000, 1.000000000000000000 ) ) ;
#32443 = EDGE_CURVE ( 'NONE', #37651, #49286, #12341, .T. ) ;
#32444 = DIRECTION ( 'NONE',  ( 1.132880637372608740E-16, 4.718402560806925739E-50, 1.000000000000000000 ) ) ;
#32445 = B_SPLINE_CURVE_WITH_KNOTS ( 'NONE', 3,
 ( #23606, #533, #47171, #24133 ),
 .UNSPECIFIED., .F., .F.,
 ( 4, 4 ),
 ( 0.000000000000000000, 0.0002520763768929601498 ),
 .UNSPECIFIED. ) ;
#32446 = ORIENTED_EDGE ( 'NONE', *, *, #28628, .T. ) ;
#32447 = VECTOR ( 'NONE', #17172, 1000.000000000000000 ) ;
#32448 = CARTESIAN_POINT ( 'NONE',  ( 1.066995270233474624, -50.00000000000000711, -3.760136334089591248 ) ) ;
#32449 = PLANE ( 'NONE',  #42552 ) ;
#32450 = VECTOR ( 'NONE', #37347, 1000.000000000000000 ) ;
#32451 = DIRECTION ( 'NONE',  ( 1.000000000000000000, 0.000000000000000000, -1.586032892321652482E-16 ) ) ;
#32452 = CARTESIAN_POINT ( 'NONE',  ( 9.999630309108590964, 0.09931773306215448127, 9.289350385289854017 ) ) ;
#32453 = AXIS2_PLACEMENT_3D ( 'NONE', #30661, #15265, #22693 ) ;
#32454 = ORIENTED_EDGE ( 'NONE', *, *, #21513, .T. ) ;
#32455 = ORIENTED_EDGE ( 'NONE', *, *, #16684, .T. ) ;
#32456 = EDGE_CURVE ( 'NONE', #48958, #25250, #43397, .T. ) ;
#32457 = DIRECTION ( 'NONE',  ( 0.000000000000000000, 1.000000000000000000, 7.004339610132985974E-48 ) ) ;
#32458 = CARTESIAN_POINT ( 'NONE',  ( -0.3862712429686729343, -1.188820645368946050, 3.333333333333333481 ) ) ;
#32459 = VECTOR ( 'NONE', #46096, 1000.000000000000000 ) ;
#32460 = ADVANCED_FACE ( 'NONE', ( #47209 ), #4402, .F. ) ;
#32461 = ORIENTED_EDGE ( 'NONE', *, *, #1747, .F. ) ;
#32462 = ADVANCED_FACE ( 'NONE', ( #8516 ), #4152, .F. ) ;
#32463 = EDGE_LOOP ( 'NONE', ( #34093, #39013, #18805, #43731 ) ) ;
#32464 = CARTESIAN_POINT ( 'NONE',  ( 0.000000000000000000, 185.0000000000000284, -356.0000000000002274 ) ) ;
#32465 = LINE ( 'NONE', #36320, #24989 ) ;
#32466 = DIRECTION ( 'NONE',  ( 3.172065745548403743E-16, 1.000000000000000000, 0.000000000000000000 ) ) ;
#32467 = CARTESIAN_POINT ( 'NONE',  ( -125.6708471809678542, 1.749999999999996669, -160.2068387089191219 ) ) ;
#32468 = VECTOR ( 'NONE', #39294, 1000.000000000000000 ) ;
#32469 = ORIENTED_EDGE ( 'NONE', *, *, #35342, .F. ) ;
#32470 = ORIENTED_EDGE ( 'NONE', *, *, #37870, .T. ) ;
#32471 = EDGE_CURVE ( 'NONE', #47169, #50656, #35469, .T. ) ;
#32472 = ORIENTED_EDGE ( 'NONE', *, *, #43094, .F. ) ;
#32473 = ADVANCED_FACE ( 'NONE', ( #24167 ), #32364, .T. ) ;
#32474 = AXIS2_PLACEMENT_3D ( 'NONE', #37134, #13240, #49108 ) ;
#32475 = LINE ( 'NONE', #40161, #43087 ) ;
#32476 =( BOUNDED_CURVE ( )  B_SPLINE_CURVE ( 3, ( #50044, #46208, #11105, #42895 ),
 .UNSPECIFIED., .F., .F. ) 
 B_SPLINE_CURVE_WITH_KNOTS ( ( 4, 4 ),
 ( 3.141592653589793116, 4.712388980384689674 ),
 .UNSPECIFIED. ) 
 CURVE ( )  GEOMETRIC_REPRESENTATION_ITEM ( )  RATIONAL_B_SPLINE_CURVE ( ( 1.000000000000000000, 0.8047378541243649375, 0.8047378541243649375, 1.000000000000000000 ) ) 
 REPRESENTATION_ITEM ( '' )  );
#32477 = CARTESIAN_POINT ( 'NONE',  ( -165.4943081650523027, 70.03596893647545585, -93.79675437945476801 ) ) ;
#32478 = ORIENTED_EDGE ( 'NONE', *, *, #33461, .F. ) ;
#32479 = ORIENTED_EDGE ( 'NONE', *, *, #36998, .T. ) ;
#32481 =( NAMED_UNIT ( * ) SI_UNIT ( $, .STERADIAN. ) SOLID_ANGLE_UNIT ( ) );
#32480 =( BOUNDED_CURVE ( )  B_SPLINE_CURVE ( 3, ( #13972, #41174, #6297, #17828 ),
 .UNSPECIFIED., .F., .F. ) 
 B_SPLINE_CURVE_WITH_KNOTS ( ( 4, 4 ),
 ( 0.000000000000000000, 1.570796326794896558 ),
 .UNSPECIFIED. ) 
 CURVE ( )  GEOMETRIC_REPRESENTATION_ITEM ( )  RATIONAL_B_SPLINE_CURVE ( ( 1.000000000000000000, 0.8047378541243649375, 0.8047378541243649375, 1.000000000000000000 ) ) 
 REPRESENTATION_ITEM ( '' )  );
#32482 = FACE_OUTER_BOUND ( 'NONE', #26218, .T. ) ;
#32483 = EDGE_LOOP ( 'NONE', ( #41419, #44857, #2262, #29087, #14985 ) ) ;
#32484 = VERTEX_POINT ( 'NONE', #816 ) ;
#32485 = EDGE_CURVE ( 'NONE', #13307, #25458, #16458, .T. ) ;
#32486 = CARTESIAN_POINT ( 'NONE',  ( 195.0540265531851105, 2.143131898507880377E-16, 42.56828755692798438 ) ) ;
#32487 = SURFACE_SIDE_STYLE ('',( #16823 ) ) ;
#32488 = ORIENTED_EDGE ( 'NONE', *, *, #43469, .F. ) ;
#32489 = AXIS2_PLACEMENT_3D ( 'NONE', #18289, #1659, #32973 ) ;
#32490 = DIRECTION ( 'NONE',  ( -0.000000000000000000, -0.000000000000000000, -1.000000000000000000 ) ) ;
#32491 = CARTESIAN_POINT ( 'NONE',  ( 85.00000000000090949, 16.00000000000000000, 0.000000000000000000 ) ) ;
#32492 = LINE ( 'NONE', #9628, #20403 ) ;
#32493 = VECTOR ( 'NONE', #2102, 1000.000000000000000 ) ;
#32494 = EDGE_CURVE ( 'NONE', #24669, #43275, #47707, .T. ) ;
#32495 = CARTESIAN_POINT ( 'NONE',  ( -46.69597344681494633, -1.750000000000010658, -119.1817124430720440 ) ) ;
#32496 = VECTOR ( 'NONE', #19254, 1000.000000000000000 ) ;
#32497 = ORIENTED_EDGE ( 'NONE', *, *, #25378, .T. ) ;
#32498 = PLANE ( 'NONE',  #47940 ) ;
#32499 = FACE_OUTER_BOUND ( 'NONE', #29171, .T. ) ;
#32500 =( BOUNDED_CURVE ( )  B_SPLINE_CURVE ( 3, ( #23289, #7406, #19181, #34601 ),
 .UNSPECIFIED., .F., .F. ) 
 B_SPLINE_CURVE_WITH_KNOTS ( ( 4, 4 ),
 ( 0.000000000000000000, 1.570796326794896558 ),
 .UNSPECIFIED. ) 
 CURVE ( )  GEOMETRIC_REPRESENTATION_ITEM ( )  RATIONAL_B_SPLINE_CURVE ( ( 1.000000000000000000, 0.8047378541243649375, 0.8047378541243649375, 1.000000000000000000 ) ) 
 REPRESENTATION_ITEM ( '' )  );
#32501 = DIRECTION ( 'NONE',  ( 0.000000000000000000, 0.000000000000000000, 1.000000000000000000 ) ) ;
#32502 = DIRECTION ( 'NONE',  ( 1.000000000000000000, 0.000000000000000000, 0.000000000000000000 ) ) ;
#32503 = AXIS2_PLACEMENT_3D ( 'NONE', #18497, #14135, #6701 ) ;
#32504 = EDGE_CURVE ( 'NONE', #49119, #10420, #8360, .T. ) ;
#32505 = EDGE_CURVE ( 'NONE', #49828, #24745, #13581, .T. ) ;
#32506 = AXIS2_PLACEMENT_3D ( 'NONE', #17636, #5068, #33049 ) ;
#32507 = EDGE_CURVE ( 'NONE', #14529, #19026, #36223, .T. ) ;
#32508 = CARTESIAN_POINT ( 'NONE',  ( 10.49999999999996447, 8.875661936878630698, 18.94832733001756253 ) ) ;
#32509 = EDGE_CURVE ( 'NONE', #14108, #33082, #29768, .T. ) ;
#32510 = CARTESIAN_POINT ( 'NONE',  ( 1.040834085586084257E-14, -6.912230148066169200, 5.000000000000000000 ) ) ;
#32511 = CARTESIAN_POINT ( 'NONE',  ( 155.0540265531850537, 2.143131898507880377E-16, -160.9317124430720014 ) ) ;
#32512 = VECTOR ( 'NONE', #12369, 1000.000000000000000 ) ;
#32513 = ADVANCED_FACE ( 'NONE', ( #33134 ), #37248, .T. ) ;
#32514 = ORIENTED_EDGE ( 'NONE', *, *, #32788, .T. ) ;
#32515 = CARTESIAN_POINT ( 'NONE',  ( 31.55402655318503236, 0.000000000000000000, 122.5682875569279702 ) ) ;
#32516 = CARTESIAN_POINT ( 'NONE',  ( -4.999999999999948486, -214.9999999999999716, -234.7500000000000000 ) ) ;
#32517 = ORIENTED_EDGE ( 'NONE', *, *, #3396, .T. ) ;
#32518 = CYLINDRICAL_SURFACE ( 'NONE', #20450, 1.750000000000001554 ) ;
#32519 = FACE_OUTER_BOUND ( 'NONE', #17494, .T. ) ;
#32520 = VERTEX_POINT ( 'NONE', #17947 ) ;
#32521 = CARTESIAN_POINT ( 'NONE',  ( 210.0000000000000568, 0.000000000000000000, -159.1817124430720298 ) ) ;
#32522 = VERTEX_POINT ( 'NONE', #29514 ) ;
#32523 = ORIENTED_EDGE ( 'NONE', *, *, #49942, .T. ) ;
#32524 = CARTESIAN_POINT ( 'NONE',  ( 1.035950918207909632, 50.00000000000000711, -2.408242355805840784 ) ) ;
#32525 = CARTESIAN_POINT ( 'NONE',  ( 210.0000000000000568, 0.000000000000000000, 40.81828755692798438 ) ) ;
#32526 = AXIS2_PLACEMENT_3D ( 'NONE', #48619, #40729, #12763 ) ;
#32527 = EDGE_LOOP ( 'NONE', ( #14660, #760, #11036, #467, #8264, #19585 ) ) ;
#32528 = EDGE_CURVE ( 'NONE', #30619, #27759, #35163, .T. ) ;
#32529 = CARTESIAN_POINT ( 'NONE',  ( 135.0000000000015632, 17.00000000000000000, 60.00000000000000000 ) ) ;
#32530 = ORIENTED_EDGE ( 'NONE', *, *, #41853, .T. ) ;
#32531 = EDGE_LOOP ( 'NONE', ( #23754, #44472, #9109, #13700, #24645, #32579 ) ) ;
#32532 = CARTESIAN_POINT ( 'NONE',  ( 344.0000000000000000, -166.9999999999999716, 341.9999999999998295 ) ) ;
#32533 = VERTEX_POINT ( 'NONE', #1818 ) ;
#32534 = CARTESIAN_POINT ( 'NONE',  ( -4.672045878990125800, 33.19353511768168374, 1.847720168420772691 ) ) ;
#32535 = CARTESIAN_POINT ( 'NONE',  ( -24.39427009666018265, -44.07992421011638129, 8.807470649214879543 ) ) ;
#32536 = CARTESIAN_POINT ( 'NONE',  ( 341.9999999999999432, 181.0000000000000568, -356.0000000000002274 ) ) ;
#32537 = ORIENTED_EDGE ( 'NONE', *, *, #40330, .T. ) ;
#32538 = LINE ( 'NONE', #24570, #30874 ) ;
#32539 = CARTESIAN_POINT ( 'NONE',  ( -1.011271242968693862, 0.7347315653655780432, 10.00000000000000000 ) ) ;
#32540 = ORIENTED_EDGE ( 'NONE', *, *, #35680, .F. ) ;
#32541 = VERTEX_POINT ( 'NONE', #22062 ) ;
#32542 = ORIENTED_EDGE ( 'NONE', *, *, #376, .F. ) ;
#32543 = CARTESIAN_POINT ( 'NONE',  ( -124.9459734468149463, 2.143131898507847836E-16, 119.0682875569279844 ) ) ;
#32544 = ADVANCED_FACE ( 'NONE', ( #17461 ), #10014, .T. ) ;
#32545 = LINE ( 'NONE', #32791, #41418 ) ;
#32546 = ORIENTED_EDGE ( 'NONE', *, *, #3976, .F. ) ;
#32547 = AXIS2_PLACEMENT_3D ( 'NONE', #44587, #28479, #40035 ) ;
#32548 = CARTESIAN_POINT ( 'NONE',  ( -1.011271242968683426, -0.7347315653655928092, -3.333333333333333481 ) ) ;
#32549 = CARTESIAN_POINT ( 'NONE',  ( 240.0000000000000000, -164.9999999999999716, 62.29650858650038003 ) ) ;
#32550 = CARTESIAN_POINT ( 'NONE',  ( 155.0540265531850537, 2.143131898507880377E-16, 82.56828755692798438 ) ) ;
#32551 = CARTESIAN_POINT ( 'NONE',  ( -87.72109971266203843, -1.750000000000010214, 79.79316129108087807 ) ) ;
#32552 = CARTESIAN_POINT ( 'NONE',  ( 195.0540265531851105, 2.143131898507880377E-16, 2.568287556927978166 ) ) ;
#32553 = PLANE ( 'NONE',  #3703 ) ;
#32554 = CARTESIAN_POINT ( 'NONE',  ( 210.0000000000000568, 0.000000000000000000, -159.1817124430720298 ) ) ;
#32555 = CARTESIAN_POINT ( 'NONE',  ( -126.6959734468149321, -1.749999999999997335, 120.8182875569279702 ) ) ;
#32556 = LINE ( 'NONE', #4591, #19962 ) ;
#32557 = EDGE_CURVE ( 'NONE', #31711, #49297, #19558, .T. ) ;
#32558 = EDGE_CURVE ( 'NONE', #31642, #15166, #37738, .T. ) ;
#32559 = AXIS2_PLACEMENT_3D ( 'NONE', #6148, #49706, #33363 ) ;
#32560 = CARTESIAN_POINT ( 'NONE',  ( -21.58778298521296080, 25.34222074689773407, 3.199614146704519602 ) ) ;
#32561 = ORIENTED_EDGE ( 'NONE', *, *, #3543, .T. ) ;
#32562 = DIRECTION ( 'NONE',  ( -0.000000000000000000, -0.000000000000000000, -1.000000000000000000 ) ) ;
#32563 = EDGE_CURVE ( 'NONE', #9657, #50336, #2068, .T. ) ;
#32564 = EDGE_CURVE ( 'NONE', #8390, #41541, #19869, .T. ) ;
#32565 = CARTESIAN_POINT ( 'NONE',  ( -37.90972275097262667, 14.83505920947805556, 901.8832493327278144 ) ) ;
#32566 = CARTESIAN_POINT ( 'NONE',  ( -4.999999999999997335, 214.9999999999999716, -230.2499999999999716 ) ) ;
#32567 = B_SPLINE_CURVE_WITH_KNOTS ( 'NONE', 3,
 ( #49799, #50054, #3140, #34998 ),
 .UNSPECIFIED., .F., .F.,
 ( 4, 4 ),
 ( 1.734723475976807094E-18, 0.002458791966311097647 ),
 .UNSPECIFIED. ) ;
#32568 = CARTESIAN_POINT ( 'NONE',  ( 73.30402655318508209, -1.750000000000010658, 80.81828755692798438 ) ) ;
#32569 = ADVANCED_FACE ( 'NONE', ( #13843 ), #13100, .T. ) ;
#32570 = ADVANCED_FACE ( 'NONE', ( #41566 ), #36743, .T. ) ;
#32571 = ORIENTED_EDGE ( 'NONE', *, *, #40874, .T. ) ;
#32572 = PLANE ( 'NONE',  #34415 ) ;
#32573 =( BOUNDED_CURVE ( )  B_SPLINE_CURVE ( 3, ( #15965, #8782, #24430, #25173 ),
 .UNSPECIFIED., .F., .F. ) 
 B_SPLINE_CURVE_WITH_KNOTS ( ( 4, 4 ),
 ( 3.141592653589793116, 4.712388980384689674 ),
 .UNSPECIFIED. ) 
 CURVE ( )  GEOMETRIC_REPRESENTATION_ITEM ( )  RATIONAL_B_SPLINE_CURVE ( ( 1.000000000000000000, 0.8047378541243649375, 0.8047378541243649375, 1.000000000000000000 ) ) 
 REPRESENTATION_ITEM ( '' )  );
#32574 = VERTEX_POINT ( 'NONE', #28762 ) ;
#32575 = CARTESIAN_POINT ( 'NONE',  ( 3.808200756227633654, 0.8261963378076531139, 9.741991644047248045 ) ) ;
#32576 = CARTESIAN_POINT ( 'NONE',  ( 75.05402655318509630, 2.143131898507880377E-16, -120.9317124430720725 ) ) ;
#32577 = CARTESIAN_POINT ( 'NONE',  ( -128.4459734468149179, 0.000000000000000000, 159.0682875569279986 ) ) ;
#32578 = ADVANCED_FACE ( 'NONE', ( #33381 ), #19085, .T. ) ;
#32579 = ORIENTED_EDGE ( 'NONE', *, *, #4909, .T. ) ;
#32580 = ORIENTED_EDGE ( 'NONE', *, *, #30006, .F. ) ;
#32581 = ORIENTED_EDGE ( 'NONE', *, *, #30278, .F. ) ;
#32582 = ORIENTED_EDGE ( 'NONE', *, *, #17340, .T. ) ;
#32583 = CARTESIAN_POINT ( 'NONE',  ( -168.4459734468149463, 0.000000000000000000, 39.06828755692798438 ) ) ;
#32584 = CARTESIAN_POINT ( 'NONE',  ( -24.39427009666018265, -44.07992421011638129, 8.807470649214879543 ) ) ;
#32585 = ORIENTED_EDGE ( 'NONE', *, *, #48382, .T. ) ;
#32586 = DIRECTION ( 'NONE',  ( -1.000000000000000000, 0.000000000000000000, 0.000000000000000000 ) ) ;
#32587 = CARTESIAN_POINT ( 'NONE',  ( -2.462075149652696027, 16.57295996686994499, 9.403735324607438884 ) ) ;
#32588 = CARTESIAN_POINT ( 'NONE',  ( -33.89193117067293315, -33.89193117067293315, 910.0000000000000000 ) ) ;
#32589 = CARTESIAN_POINT ( 'NONE',  ( -9.260964247899876156, 13.84230907185616744, -9.683996418299976483 ) ) ;
#32590 = ORIENTED_EDGE ( 'NONE', *, *, #48842, .F. ) ;
#32591 = PLANE ( 'NONE',  #1044 ) ;
#32592 = EDGE_LOOP ( 'NONE', ( #2219, #41088, #11049, #46942 ) ) ;
#32593 = VECTOR ( 'NONE', #44193, 1000.000000000000000 ) ;
#32594 = LINE ( 'NONE', #48178, #39893 ) ;
#32595 = CARTESIAN_POINT ( 'NONE',  ( 169.0000000000000000, -174.9999999999999716, -113.0000000000001563 ) ) ;
#32596 = ORIENTED_EDGE ( 'NONE', *, *, #48462, .F. ) ;
#32597 = ORIENTED_EDGE ( 'NONE', *, *, #15933, .T. ) ;
#32598 = CARTESIAN_POINT ( 'NONE',  ( 360.0000000000000000, -169.0000000000001137, -349.9999999999999432 ) ) ;
#32599 = CARTESIAN_POINT ( 'NONE',  ( 166.9999999999999716, -5.999999999999950262, 339.9999999999998295 ) ) ;
#32600 = ORIENTED_EDGE ( 'NONE', *, *, #23346, .F. ) ;
#32601 = EDGE_CURVE ( 'NONE', #29839, #34606, #9503, .T. ) ;
#32602 = DIRECTION ( 'NONE',  ( 0.000000000000000000, -0.000000000000000000, -1.000000000000000000 ) ) ;
#32603 = CARTESIAN_POINT ( 'NONE',  ( 240.0000000000000000, -164.9999999999999716, 474.9999999999998863 ) ) ;
#32604 = CARTESIAN_POINT ( 'NONE',  ( 28.52604530808654815, 41.07801380285680892, -3.760136334089591248 ) ) ;
#32605 = ORIENTED_EDGE ( 'NONE', *, *, #26806, .F. ) ;
#32606 = CARTESIAN_POINT ( 'NONE',  ( 9.174209336589868258, 3.979181203266223488, 9.646707543097347681 ) ) ;
#32607 = CARTESIAN_POINT ( 'NONE',  ( -14.99999999999876366, 17.00000000000000000, 5.000000000000004441 ) ) ;
#32608 = DIRECTION ( 'NONE',  ( -1.000000000000000000, -0.000000000000000000, -0.000000000000000000 ) ) ;
#32609 = VERTEX_POINT ( 'NONE', #23070 ) ;
#32610 = ORIENTED_EDGE ( 'NONE', *, *, #32954, .F. ) ;
#32611 = DIRECTION ( 'NONE',  ( 0.000000000000000000, -1.000000000000000000, 2.969158215481698263E-48 ) ) ;
#32612 = EDGE_CURVE ( 'NONE', #41298, #12448, #41617, .T. ) ;
#32613 = CARTESIAN_POINT ( 'NONE',  ( -543.5050241616419271, -61.66198943095990614, -176.2397770772458898 ) ) ;
#32614 = CARTESIAN_POINT ( 'NONE',  ( -165.6708471809677974, 1.750000000000010214, -120.2068387089191219 ) ) ;
#32615 = ORIENTED_EDGE ( 'NONE', *, *, #18001, .F. ) ;
#32616 = CARTESIAN_POINT ( 'NONE',  ( 359.9999999999999432, -181.0000000000001421, -349.9999999999998863 ) ) ;
#32617 = CARTESIAN_POINT ( 'NONE',  ( -48.44597344681496054, -1.025126265847089657, 42.56828755692799149 ) ) ;
#32618 = DIRECTION ( 'NONE',  ( -1.000000000000000000, -0.000000000000000000, -0.000000000000000000 ) ) ;
#32619 = EDGE_CURVE ( 'NONE', #6739, #17123, #46374, .T. ) ;
#32620 = EDGE_CURVE ( 'NONE', #50433, #14892, #9746, .T. ) ;
#32621 =( BOUNDED_CURVE ( )  B_SPLINE_CURVE ( 3, ( #37531, #10056, #32218, #41356 ),
 .UNSPECIFIED., .F., .F. ) 
 B_SPLINE_CURVE_WITH_KNOTS ( ( 4, 4 ),
 ( 1.570796326794896558, 3.141592653589793116 ),
 .UNSPECIFIED. ) 
 CURVE ( )  GEOMETRIC_REPRESENTATION_ITEM ( )  RATIONAL_B_SPLINE_CURVE ( ( 1.000000000000000000, 0.8047378541243649375, 0.8047378541243649375, 1.000000000000000000 ) ) 
 REPRESENTATION_ITEM ( '' )  );
#32622 = ORIENTED_EDGE ( 'NONE', *, *, #22389, .F. ) ;
#32623 = LINE ( 'NONE', #6418, #10878 ) ;
#32625 = VERTEX_POINT ( 'NONE', #22566 ) ;
#32624 = VECTOR ( 'NONE', #31233, 1000.000000000000000 ) ;
#32626 = DIRECTION ( 'NONE',  ( 1.586032892321652236E-16, 1.000000000000000000, 2.288264760618012091E-48 ) ) ;
#32627 = VERTEX_POINT ( 'NONE', #7689 ) ;
#32628 = EDGE_CURVE ( 'NONE', #20753, #15030, #42253, .T. ) ;
#32629 = FACE_OUTER_BOUND ( 'NONE', #36215, .T. ) ;
#32630 = CYLINDRICAL_SURFACE ( 'NONE', #39686, 1.750000000000015543 ) ;
#32631 =( BOUNDED_CURVE ( )  B_SPLINE_CURVE ( 3, ( #47414, #20262, #15, #39020 ),
 .UNSPECIFIED., .F., .F. ) 
 B_SPLINE_CURVE_WITH_KNOTS ( ( 4, 4 ),
 ( 4.712388980384689674, 6.283185307179586232 ),
 .UNSPECIFIED. ) 
 CURVE ( )  GEOMETRIC_REPRESENTATION_ITEM ( )  RATIONAL_B_SPLINE_CURVE ( ( 1.000000000000000000, 0.8047378541243649375, 0.8047378541243649375, 1.000000000000000000 ) ) 
 REPRESENTATION_ITEM ( '' )  );
#32632 = CARTESIAN_POINT ( 'NONE',  ( 135.0000000000021600, 17.00000000000000000, 95.00000000000000000 ) ) ;
#32633 = ORIENTED_EDGE ( 'NONE', *, *, #27123, .F. ) ;
#32634 = CARTESIAN_POINT ( 'NONE',  ( -8.445973446814976526, 0.000000000000000000, 39.06828755692792754 ) ) ;
#32635 = ORIENTED_EDGE ( 'NONE', *, *, #20651, .F. ) ;
#32636 = CYLINDRICAL_SURFACE ( 'NONE', #40234, 1.880036658038868103 ) ;
#32637 = CYLINDRICAL_SURFACE ( 'NONE', #24076, 1.750000000000010214 ) ;
#32638 = CARTESIAN_POINT ( 'NONE',  ( 1.540526284687965264, -1.371707213411490267, 9.886433018048071730 ) ) ;
#32639 = CARTESIAN_POINT ( 'NONE',  ( 342.0000000000000568, 181.0000000000000284, 355.9999999999998863 ) ) ;
#32640 = CARTESIAN_POINT ( 'NONE',  ( 15.44803555374680393, 6.237487519713364570, -3.546734833711462365 ) ) ;
#32641 = ORIENTED_EDGE ( 'NONE', *, *, #42891, .T. ) ;
#32642 = ORIENTED_EDGE ( 'NONE', *, *, #31867, .F. ) ;
#32643 = DIRECTION ( 'NONE',  ( -1.000000000000000000, -0.000000000000000000, -0.000000000000000000 ) ) ;
#32644 = ORIENTED_EDGE ( 'NONE', *, *, #16270, .T. ) ;
#32645 = CARTESIAN_POINT ( 'NONE',  ( 168.9999999999999716, -270.4999999999999432, -339.9999999999998863 ) ) ;
#32646 = DIRECTION ( 'NONE',  ( 0.000000000000000000, -0.000000000000000000, 1.000000000000000000 ) ) ;
#32647 = CARTESIAN_POINT ( 'NONE',  ( -0.03684434657425742637, -1.221810944802247167, 9.969517326150317160 ) ) ;
#32648 = ORIENTED_EDGE ( 'NONE', *, *, #26581, .F. ) ;
#32649 = CARTESIAN_POINT ( 'NONE',  ( 10.01251772323701594, 8.486842105263161073, -18.46084505325461578 ) ) ;
#32650 = CARTESIAN_POINT ( 'NONE',  ( 210.0000000000000568, 0.000000000000000000, -119.1817124430720440 ) ) ;
#32651 = LINE ( 'NONE', #44422, #39126 ) ;
#32652 = EDGE_CURVE ( 'NONE', #38860, #46422, #41814, .T. ) ;
#32653 = FACE_OUTER_BOUND ( 'NONE', #23337, .T. ) ;
#32654 = DIRECTION ( 'NONE',  ( -1.000000000000000000, 0.000000000000000000, 0.000000000000000000 ) ) ;
#32655 = CARTESIAN_POINT ( 'NONE',  ( -6.695973446814940111, -1.750000000000024203, -119.1817124430720440 ) ) ;
#32656 = EDGE_LOOP ( 'NONE', ( #42667, #13258, #8723, #9465, #48364 ) ) ;
#32657 = AXIS2_PLACEMENT_3D ( 'NONE', #38619, #3175, #35282 ) ;
#32658 = ORIENTED_EDGE ( 'NONE', *, *, #29517, .F. ) ;
#32659 = ORIENTED_EDGE ( 'NONE', *, *, #20668, .F. ) ;
#32660 = CARTESIAN_POINT ( 'NONE',  ( 193.3040265531851105, -1.750000000000010658, -119.1817124430720440 ) ) ;
#32661 = PLANE ( 'NONE',  #28354 ) ;
#32662 = CARTESIAN_POINT ( 'NONE',  ( -7.608425291889091113, 36.72004717559254772, 7.697694107796188234 ) ) ;
#32663 = CARTESIAN_POINT ( 'NONE',  ( 341.9999999999999432, 167.8284271247463835, -342.8284271247465540 ) ) ;
#32664 = ORIENTED_EDGE ( 'NONE', *, *, #3585, .T. ) ;
#32665 = CARTESIAN_POINT ( 'NONE',  ( 5.551115123125782702E-14, -180.9999999999999716, 341.9999999999997726 ) ) ;
#32666 = ORIENTED_EDGE ( 'NONE', *, *, #7997, .T. ) ;
#32667 = CARTESIAN_POINT ( 'NONE',  ( 183.0000000000000000, -268.5000000000002842, -114.9999999999999147 ) ) ;
#32668 = CARTESIAN_POINT ( 'NONE',  ( -84.94597344681494633, 2.143131898507880377E-16, 165.0000000000000000 ) ) ;
#32669 = CARTESIAN_POINT ( 'NONE',  ( 224.9999999999999716, -164.9999999999999716, 62.29650858650038003 ) ) ;
#32670 = DIRECTION ( 'NONE',  ( 0.000000000000000000, 0.000000000000000000, 1.000000000000000000 ) ) ;
#32671 = LINE ( 'NONE', #1627, #37263 ) ;
#32672 = CARTESIAN_POINT ( 'NONE',  ( 344.0000000000000000, -165.0000000000001137, 340.0000000000000568 ) ) ;
#32673 = ORIENTED_EDGE ( 'NONE', *, *, #13046, .F. ) ;
#32674 = FACE_OUTER_BOUND ( 'NONE', #27299, .T. ) ;
#32675 = PRODUCT_DEFINITION_SHAPE ( 'NONE', 'NONE',  #25918 ) ;
#32676 = CARTESIAN_POINT ( 'NONE',  ( -14.49999999999999822, 12.98684210526315930, 19.37312575500899925 ) ) ;
#32677 = DIRECTION ( 'NONE',  ( -0.000000000000000000, -0.000000000000000000, -1.000000000000000000 ) ) ;
#32678 = LINE ( 'NONE', #380, #14202 ) ;
#32679 = VERTEX_POINT ( 'NONE', #23330 ) ;
#32680 = DIRECTION ( 'NONE',  ( 0.000000000000000000, -5.664403186863042467E-17, -1.000000000000000000 ) ) ;
#32681 = ORIENTED_EDGE ( 'NONE', *, *, #10709, .F. ) ;
#32682 = EDGE_CURVE ( 'NONE', #576, #13837, #37989, .T. ) ;
#32683 = DIRECTION ( 'NONE',  ( 1.000000000000000000, -3.172065799423185948E-16, 1.587271980518778491E-16 ) ) ;
#32684 = DIRECTION ( 'NONE',  ( 3.172065745548403743E-16, 1.000000000000000000, 0.000000000000000000 ) ) ;
#32685 = AXIS2_PLACEMENT_3D ( 'NONE', #36092, #16320, #35847 ) ;
#32686 = ORIENTED_EDGE ( 'NONE', *, *, #39135, .T. ) ;
#32687 = VECTOR ( 'NONE', #7239, 1000.000000000000000 ) ;
#32688 = CARTESIAN_POINT ( 'NONE',  ( 30.65355587399079340, -13.36566953343588260, -8.917361510505369182 ) ) ;
#32689 = LINE ( 'NONE', #36813, #13868 ) ;
#32691 = VECTOR ( 'NONE', #40622, 1000.000000000000000 ) ;
#32690 = FACE_BOUND ( 'NONE', #23188, .T. ) ;
#32692 = VECTOR ( 'NONE', #24885, 1000.000000000000000 ) ;
#32693 = CARTESIAN_POINT ( 'NONE',  ( 5.083187235775197266, 8.611690166631179366, 9.646707543097347681 ) ) ;
#32694 = ADVANCED_FACE ( 'NONE', ( #19472 ), #14366, .F. ) ;
#32695 = ORIENTED_EDGE ( 'NONE', *, *, #39751, .T. ) ;
#32696 = VECTOR ( 'NONE', #8753, 1000.000000000000000 ) ;
#32697 = ORIENTED_EDGE ( 'NONE', *, *, #19919, .F. ) ;
#32698 = DIRECTION ( 'NONE',  ( 1.000000000000000000, 0.000000000000000000, 0.000000000000000000 ) ) ;
#32699 = ADVANCED_FACE ( 'NONE', ( #31043 ), #31425, .T. ) ;
#32700 = DIRECTION ( 'NONE',  ( -1.000000000000000000, 0.000000000000000000, 0.000000000000000000 ) ) ;
#32701 = VECTOR ( 'NONE', #30873, 1000.000000000000114 ) ;
#32702 = ORIENTED_EDGE ( 'NONE', *, *, #33113, .T. ) ;
#32703 = ORIENTED_EDGE ( 'NONE', *, *, #41485, .T. ) ;
#32704 = CARTESIAN_POINT ( 'NONE',  ( -126.6959734468149321, 0.000000000000000000, 165.0000000000000000 ) ) ;
#32705 = CARTESIAN_POINT ( 'NONE',  ( 72.27890028733797578, 1.750000000000009548, 81.84341382277507648 ) ) ;
#32706 = FACE_OUTER_BOUND ( 'NONE', #15337, .T. ) ;
#32707 = CARTESIAN_POINT ( 'NONE',  ( -124.9459734468149463, 2.143131898507847836E-16, -160.9317124430720014 ) ) ;
#32708 = EDGE_LOOP ( 'NONE', ( #1214, #47945, #26961, #1564 ) ) ;
#32709 = EDGE_LOOP ( 'NONE', ( #45785, #39225, #27270 ) ) ;
#32710 = ORIENTED_EDGE ( 'NONE', *, *, #18925, .F. ) ;
#32711 = B_SPLINE_CURVE_WITH_KNOTS ( 'NONE', 3,
 ( #28039, #1104, #31663, #12144 ),
 .UNSPECIFIED., .F., .F.,
 ( 4, 4 ),
 ( 0.000000000000000000, 0.002368422649471282979 ),
 .UNSPECIFIED. ) ;
#32712 = EDGE_CURVE ( 'NONE', #18412, #22853, #26415, .T. ) ;
#32713 = LINE ( 'NONE', #9856, #32450 ) ;
#32714 = ADVANCED_FACE ( 'NONE', ( #46639 ), #27727, .T. ) ;
#32715 = FACE_OUTER_BOUND ( 'NONE', #10485, .T. ) ;
#32716 = CARTESIAN_POINT ( 'NONE',  ( -10.28825587112213746, 13.03847615613166333, 3.266473740018926541 ) ) ;
#32717 = ORIENTED_EDGE ( 'NONE', *, *, #19692, .F. ) ;
#32718 = ORIENTED_EDGE ( 'NONE', *, *, #15093, .F. ) ;
#32719 = CARTESIAN_POINT ( 'NONE',  ( -204.9459734468148895, -1.025126265847088991, 2.568287556927986159 ) ) ;
#32720 = EDGE_LOOP ( 'NONE', ( #19187, #29031, #44696 ) ) ;
#32721 = VERTEX_POINT ( 'NONE', #43583 ) ;
#32722 = DIRECTION ( 'NONE',  ( -1.000000000000000000, -8.673617379884028076E-17, 0.000000000000000000 ) ) ;
#32723 = CARTESIAN_POINT ( 'NONE',  ( 14.49999999999999822, -46.51315789473684248, 5.916985404131814619 ) ) ;
#32725 = ORIENTED_EDGE ( 'NONE', *, *, #7691, .T. ) ;
#32724 = AXIS2_PLACEMENT_3D ( 'NONE', #35602, #47590, #36102 ) ;
#32726 = FACE_OUTER_BOUND ( 'NONE', #12368, .T. ) ;
#32727 = CARTESIAN_POINT ( 'NONE',  ( 6.123233995736766282E-16, 28.48684210526315752, 5.000000000000000000 ) ) ;
#32728 = CARTESIAN_POINT ( 'NONE',  ( -194.9999999999999432, -173.0000000000000000, 132.0000000000000853 ) ) ;
#32729 = VECTOR ( 'NONE', #49028, 1000.000000000000000 ) ;
#32730 = FACE_OUTER_BOUND ( 'NONE', #36515, .T. ) ;
#32731 = ORIENTED_EDGE ( 'NONE', *, *, #34194, .F. ) ;
#32732 = AXIS2_PLACEMENT_3D ( 'NONE', #44799, #29423, #9670 ) ;
#32734 = VECTOR ( 'NONE', #1506, 1000.000000000000000 ) ;
#32733 = CARTESIAN_POINT ( 'NONE',  ( 169.0000000000000000, -174.9999999999999716, -115.0000000000001563 ) ) ;
#32735 = CARTESIAN_POINT ( 'NONE',  ( 181.0000000000000000, -180.9999999999999716, -340.0000000000001137 ) ) ;
#32736 = LINE ( 'NONE', #20677, #26932 ) ;
#32737 = CARTESIAN_POINT ( 'NONE',  ( 355.9999999999999432, -185.0000000000002558, -360.0000000000003411 ) ) ;
#32738 = EDGE_CURVE ( 'NONE', #50107, #8682, #27692, .T. ) ;
#32739 = CIRCLE ( 'NONE', #3227, 4.000000000000003553 ) ;
#32740 = EDGE_CURVE ( 'NONE', #45593, #2472, #16388, .T. ) ;
#32741 = EDGE_CURVE ( 'NONE', #15045, #43660, #43079, .T. ) ;
#32742 = CARTESIAN_POINT ( 'NONE',  ( 113.3040265531850537, 1.749999999999997335, 120.8182875569279702 ) ) ;
#32743 = B_SPLINE_CURVE_WITH_KNOTS ( 'NONE', 3,
 ( #39493, #4331, #43061, #39237 ),
 .UNSPECIFIED., .F., .F.,
 ( 4, 4 ),
 ( 0.7998230999345288250, 0.9869080488566185361 ),
 .UNSPECIFIED. ) ;
#32744 = EDGE_CURVE ( 'NONE', #32625, #13604, #19985, .T. ) ;
#32745 = LINE ( 'NONE', #40947, #8156 ) ;
#32746 = CARTESIAN_POINT ( 'NONE',  ( -164.9459734468149747, 0.000000000000000000, 162.5682875569279702 ) ) ;
#32747 = FACE_OUTER_BOUND ( 'NONE', #26010, .T. ) ;
#32748 = EDGE_CURVE ( 'NONE', #30357, #30497, #31810, .T. ) ;
#32749 = ORIENTED_EDGE ( 'NONE', *, *, #35320, .T. ) ;
#32750 = CARTESIAN_POINT ( 'NONE',  ( 0.3370904143228959926, -0.2449105217885284291, 10.00000000000000000 ) ) ;
#32751 = CARTESIAN_POINT ( 'NONE',  ( 153.3040265531850537, 1.750000000000010214, 40.81828755692798438 ) ) ;
#32752 = CARTESIAN_POINT ( 'NONE',  ( 210.0000000000000568, 0.000000000000000000, 40.81828755692798438 ) ) ;
#32753 = LINE ( 'NONE', #21439, #41231 ) ;
#32754 = CARTESIAN_POINT ( 'NONE',  ( -206.6959734468149463, -1.750000000000010658, -79.18171244307201562 ) ) ;
#32755 = ORIENTED_EDGE ( 'NONE', *, *, #27768, .F. ) ;
#32756 = FACE_OUTER_BOUND ( 'NONE', #33385, .T. ) ;
#32757 = ORIENTED_EDGE ( 'NONE', *, *, #13923, .T. ) ;
#32758 = AXIS2_PLACEMENT_3D ( 'NONE', #39774, #35431, #42579 ) ;
#32759 = CARTESIAN_POINT ( 'NONE',  ( 1.142975459103954705, 16.61830776097024653, -2.870787844569587133 ) ) ;
#32760 = CARTESIAN_POINT ( 'NONE',  ( 357.1715728752537871, 183.0000000000000853, 357.9999999999998295 ) ) ;
#32761 = VECTOR ( 'NONE', #3837, 1000.000000000000000 ) ;
#32762 =( BOUNDED_CURVE ( )  B_SPLINE_CURVE ( 3, ( #42076, #30049, #48729, #5920 ),
 .UNSPECIFIED., .F., .F. ) 
 B_SPLINE_CURVE_WITH_KNOTS ( ( 4, 4 ),
 ( 4.712388980384689674, 6.283185307179586232 ),
 .UNSPECIFIED. ) 
 CURVE ( )  GEOMETRIC_REPRESENTATION_ITEM ( )  RATIONAL_B_SPLINE_CURVE ( ( 1.000000000000000000, 0.8047378541243649375, 0.8047378541243649375, 1.000000000000000000 ) ) 
 REPRESENTATION_ITEM ( '' )  );
#32763 = VECTOR ( 'NONE', #385, 1000.000000000000000 ) ;
#32764 = ORIENTED_EDGE ( 'NONE', *, *, #15993, .T. ) ;
#32765 = CARTESIAN_POINT ( 'NONE',  ( -1.275994128725546739, 0.1230186051320636409, 9.948547179989615685 ) ) ;
#32766 = DIRECTION ( 'NONE',  ( -0.000000000000000000, -0.000000000000000000, 1.000000000000000000 ) ) ;
#32767 = VERTEX_POINT ( 'NONE', #47898 ) ;
#32768 = ORIENTED_EDGE ( 'NONE', *, *, #42364, .T. ) ;
#32769 = AXIS2_PLACEMENT_3D ( 'NONE', #7213, #30564, #41851 ) ;
#32770 =( BOUNDED_CURVE ( )  B_SPLINE_CURVE ( 3, ( #41113, #29316, #45430, #37541 ),
 .UNSPECIFIED., .F., .F. ) 
 B_SPLINE_CURVE_WITH_KNOTS ( ( 4, 4 ),
 ( 3.141592653589793116, 4.712388980384689674 ),
 .UNSPECIFIED. ) 
 CURVE ( )  GEOMETRIC_REPRESENTATION_ITEM ( )  RATIONAL_B_SPLINE_CURVE ( ( 1.000000000000000000, 0.8047378541243649375, 0.8047378541243649375, 1.000000000000000000 ) ) 
 REPRESENTATION_ITEM ( '' )  );
#32771 = DIRECTION ( 'NONE',  ( -1.000000000000000000, -0.000000000000000000, -0.000000000000000000 ) ) ;
#32772 = EDGE_CURVE ( 'NONE', #12798, #40675, #36099, .T. ) ;
#32773 = EDGE_CURVE ( 'NONE', #3643, #34063, #44432, .T. ) ;
#32774 = ORIENTED_EDGE ( 'NONE', *, *, #38467, .F. ) ;
#32775 = CARTESIAN_POINT ( 'NONE',  ( 115.0540265531850395, 2.143131898507847836E-16, -80.93171244307201562 ) ) ;
#32776 = CARTESIAN_POINT ( 'NONE',  ( 210.0000000000000568, 0.000000000000000000, 80.81828755692798438 ) ) ;
#32777 = DIRECTION ( 'NONE',  ( 0.000000000000000000, 0.000000000000000000, 1.000000000000000000 ) ) ;
#32778 = VECTOR ( 'NONE', #39273, 1000.000000000000000 ) ;
#32779 = ADVANCED_FACE ( 'NONE', ( #16145 ), #27945, .F. ) ;
#32780 = EDGE_LOOP ( 'NONE', ( #7607, #27962, #42465, #4253, #40071, #36386 ) ) ;
#32781 = EDGE_CURVE ( 'NONE', #574, #4352, #4091, .T. ) ;
#32782 = CARTESIAN_POINT ( 'NONE',  ( 1.040834085586084257E-14, -6.912230148066169200, -5.000000000000000000 ) ) ;
#32783 = FILL_AREA_STYLE_COLOUR ( '', #21255 ) ;
#32784 = ORIENTED_EDGE ( 'NONE', *, *, #44055, .F. ) ;
#32785 = ORIENTED_EDGE ( 'NONE', *, *, #25555, .F. ) ;
#32786 = ORIENTED_EDGE ( 'NONE', *, *, #1116, .F. ) ;
#32787 = CARTESIAN_POINT ( 'NONE',  ( -87.72109971266203843, 1.750000000000010436, 79.79316129108087807 ) ) ;
#32788 = EDGE_CURVE ( 'NONE', #32004, #14784, #28199, .T. ) ;
#32789 = EDGE_CURVE ( 'NONE', #405, #33858, #20489, .T. ) ;
#32790 =( BOUNDED_CURVE ( )  B_SPLINE_CURVE ( 3, ( #26456, #38288, #10800, #42093 ),
 .UNSPECIFIED., .F., .F. ) 
 B_SPLINE_CURVE_WITH_KNOTS ( ( 4, 4 ),
 ( 3.141592653589793116, 4.712388980384689674 ),
 .UNSPECIFIED. ) 
 CURVE ( )  GEOMETRIC_REPRESENTATION_ITEM ( )  RATIONAL_B_SPLINE_CURVE ( ( 1.000000000000000000, 0.8047378541243649375, 0.8047378541243649375, 1.000000000000000000 ) ) 
 REPRESENTATION_ITEM ( '' )  );
#32791 = CARTESIAN_POINT ( 'NONE',  ( 355.9999999999999432, 174.9999999999996305, -360.0000000000003411 ) ) ;
#32792 = ORIENTED_EDGE ( 'NONE', *, *, #41794, .T. ) ;
#32793 = DIRECTION ( 'NONE',  ( 0.2599384441937669932, -0.8000082703740931667, -0.5407575913134976542 ) ) ;
#32794 = DIRECTION ( 'NONE',  ( 0.000000000000000000, 0.000000000000000000, 1.000000000000000000 ) ) ;
#32795 = CARTESIAN_POINT ( 'NONE',  ( 193.3040265531851105, 0.000000000000000000, 165.0000000000000000 ) ) ;
#32796 = CARTESIAN_POINT ( 'NONE',  ( -45.67084718096785423, -1.750000000000009548, -160.2068387089191219 ) ) ;
#32797 = CARTESIAN_POINT ( 'NONE',  ( 343.9999999999999432, -183.0000000000001421, -349.9999999999998863 ) ) ;
#32798 = CARTESIAN_POINT ( 'NONE',  ( 18.69789054174343690, -27.49790346457731616, -2.408242355805840784 ) ) ;
#32799 = CARTESIAN_POINT ( 'NONE',  ( 0.000000000000000000, 17.00000000000000000, 0.000000000000000000 ) ) ;
#32800 = DIRECTION ( 'NONE',  ( -0.000000000000000000, -0.000000000000000000, -1.000000000000000000 ) ) ;
#32801 = CARTESIAN_POINT ( 'NONE',  ( 153.3040265531850537, 0.000000000000000000, -165.0000000000000000 ) ) ;
#32802 = VECTOR ( 'NONE', #7398, 1000.000000000000000 ) ;
#32803 = ADVANCED_FACE ( 'NONE', ( #44077 ), #8945, .F. ) ;
#32804 = AXIS2_PLACEMENT_3D ( 'NONE', #27064, #42697, #7066 ) ;
#32805 = CARTESIAN_POINT ( 'NONE',  ( 0.000000000000000000, 23.48684210526316107, 0.000000000000000000 ) ) ;
#32806 = VECTOR ( 'NONE', #5915, 1000.000000000000000 ) ;
#32807 = EDGE_CURVE ( 'NONE', #37393, #40932, #46892, .T. ) ;
#32808 = EDGE_CURVE ( 'NONE', #3579, #48120, #35157, .T. ) ;
#32809 = AXIS2_PLACEMENT_3D ( 'NONE', #12715, #42998, #42733 ) ;
#32810 = DIRECTION ( 'NONE',  ( -1.000000000000000000, 0.000000000000000000, 0.000000000000000000 ) ) ;
#32811 = ORIENTED_EDGE ( 'NONE', *, *, #24236, .F. ) ;
#32812 = CIRCLE ( 'NONE', #7429, 2.000000000000001776 ) ;
#32813 = CARTESIAN_POINT ( 'NONE',  ( -1.019713130072858798, -3.848720492505054658, 6.098637220230962441E-17 ) ) ;
#32814 = VECTOR ( 'NONE', #39547, 1000.000000000000000 ) ;
#32815 = B_SPLINE_CURVE_WITH_KNOTS ( 'NONE', 3,
 ( #10422, #21208, #21970, #14519 ),
 .UNSPECIFIED., .F., .F.,
 ( 4, 4 ),
 ( 0.0001970727314178603461, 0.006335152926028601167 ),
 .UNSPECIFIED. ) ;
#32816 = CARTESIAN_POINT ( 'NONE',  ( -165.0000000000000284, 16.00000000000000000, -90.00000000000000000 ) ) ;
#32817 = PLANE ( 'NONE',  #44637 ) ;
#32818 = DIRECTION ( 'NONE',  ( 1.000000000000000000, 0.000000000000000000, 0.000000000000000000 ) ) ;
#32819 = AXIS2_PLACEMENT_3D ( 'NONE', #33090, #45341, #10229 ) ;
#32820 = ORIENTED_EDGE ( 'NONE', *, *, #43493, .T. ) ;
#32821 = CARTESIAN_POINT ( 'NONE',  ( -164.9999999999994031, 17.00000000000000000, -54.99999999999999289 ) ) ;
#32822 = B_SPLINE_CURVE_WITH_KNOTS ( 'NONE', 3,
 ( #24186, #47232, #28022, #15711 ),
 .UNSPECIFIED., .F., .F.,
 ( 4, 4 ),
 ( 0.000000000000000000, 8.326314924661335100E-06 ),
 .UNSPECIFIED. ) ;
#32823 = DIRECTION ( 'NONE',  ( 0.000000000000000000, 0.000000000000000000, -1.000000000000000000 ) ) ;
#32824 = ORIENTED_EDGE ( 'NONE', *, *, #46529, .F. ) ;
#32825 = CARTESIAN_POINT ( 'NONE',  ( 46.76852358249013975, -17.86468378716709537, -9.367992836599954742 ) ) ;
#32827 = EDGE_CURVE ( 'NONE', #40281, #30823, #6996, .T. ) ;
#32826 = LINE ( 'NONE', #1271, #31404 ) ;
#32828 = CARTESIAN_POINT ( 'NONE',  ( 112.2789002873379758, 1.749999999999997113, -120.2068387089191219 ) ) ;
#32829 = ORIENTED_EDGE ( 'NONE', *, *, #32109, .F. ) ;
#32830 = CARTESIAN_POINT ( 'NONE',  ( 2.499999999999956035, -194.9999999999999716, -240.0000000000000000 ) ) ;
#32831 = EDGE_LOOP ( 'NONE', ( #5668, #6501, #15199, #31150, #5016 ) ) ;
#32832 = VERTEX_POINT ( 'NONE', #31305 ) ;
#32833 = ORIENTED_EDGE ( 'NONE', *, *, #26782, .F. ) ;
#32834 = CYLINDRICAL_SURFACE ( 'NONE', #44202, 3.749999999999975575 ) ;
#32835 = LINE ( 'NONE', #29226, #49431 ) ;
#32836 =( BOUNDED_CURVE ( )  B_SPLINE_CURVE ( 3, ( #22935, #16258, #11908, #31160 ),
 .UNSPECIFIED., .F., .F. ) 
 B_SPLINE_CURVE_WITH_KNOTS ( ( 4, 4 ),
 ( 1.570796326794896558, 3.141592653589793116 ),
 .UNSPECIFIED. ) 
 CURVE ( )  GEOMETRIC_REPRESENTATION_ITEM ( )  RATIONAL_B_SPLINE_CURVE ( ( 1.000000000000000000, 0.8047378541243649375, 0.8047378541243649375, 1.000000000000000000 ) ) 
 REPRESENTATION_ITEM ( '' )  );
#32837 = EDGE_CURVE ( 'NONE', #17816, #43954, #47395, .T. ) ;
#32838 = ORIENTED_EDGE ( 'NONE', *, *, #3052, .F. ) ;
#32839 = FACE_OUTER_BOUND ( 'NONE', #23904, .T. ) ;
#32840 = FACE_OUTER_BOUND ( 'NONE', #35316, .T. ) ;
#32841 = LINE ( 'NONE', #33093, #31361 ) ;
#32842 = DIRECTION ( 'NONE',  ( 2.958228394578793832E-31, 0.000000000000000000, 1.000000000000000000 ) ) ;
#32843 = ORIENTED_EDGE ( 'NONE', *, *, #31509, .F. ) ;
#32844 = DIRECTION ( 'NONE',  ( 1.000000000000000000, 0.000000000000000000, 0.000000000000000000 ) ) ;
#32845 = AXIS2_PLACEMENT_3D ( 'NONE', #35232, #39332, #75 ) ;
#32846 = EDGE_CURVE ( 'NONE', #31251, #35508, #22444, .T. ) ;
#32847 = AXIS2_PLACEMENT_3D ( 'NONE', #38754, #3576, #23856 ) ;
#32848 = ORIENTED_EDGE ( 'NONE', *, *, #2036, .F. ) ;
#32849 = EDGE_CURVE ( 'NONE', #37221, #30766, #37587, .T. ) ;
#32850 = DIRECTION ( 'NONE',  ( -0.000000000000000000, -0.000000000000000000, -1.000000000000000000 ) ) ;
#32851 = CARTESIAN_POINT ( 'NONE',  ( 9.185112145816566098, 0.000000000000000000, 0.000000000000000000 ) ) ;
#32852 = ORIENTED_EDGE ( 'NONE', *, *, #33068, .T. ) ;
#32853 = ORIENTED_EDGE ( 'NONE', *, *, #7184, .T. ) ;
#32854 = ORIENTED_EDGE ( 'NONE', *, *, #29415, .T. ) ;
#32855 = FACE_OUTER_BOUND ( 'NONE', #46645, .T. ) ;
#32856 = EDGE_CURVE ( 'NONE', #7083, #26946, #34009, .T. ) ;
#32857 = LINE ( 'NONE', #48437, #20946 ) ;
#32858 = CIRCLE ( 'NONE', #2505, 1.750000000000015543 ) ;
#32859 = ORIENTED_EDGE ( 'NONE', *, *, #2294, .T. ) ;
#32860 = EDGE_CURVE ( 'NONE', #5763, #47457, #42787, .T. ) ;
#32861 = CARTESIAN_POINT ( 'NONE',  ( -26.18032376592659105, 21.95228666728381128, 7.455576670931136185 ) ) ;
#32862 = CARTESIAN_POINT ( 'NONE',  ( -85.67084718096784002, -1.750000000000010436, 79.79316129108087807 ) ) ;
#32863 = ADVANCED_FACE ( 'NONE', ( #48399 ), #20741, .T. ) ;
#32864 = CARTESIAN_POINT ( 'NONE',  ( -1.011271242968693862, 0.7347315653655780432, 3.333333333333333481 ) ) ;
#32865 = ORIENTED_EDGE ( 'NONE', *, *, #15627, .T. ) ;
#32866 = CARTESIAN_POINT ( 'NONE',  ( 80.00000000000122213, 17.00000000000000000, 30.00000000000000000 ) ) ;
#32867 = LINE ( 'NONE', #21543, #11173 ) ;
#32868 = EDGE_CURVE ( 'NONE', #38709, #40720, #44559, .T. ) ;
#32869 = DIRECTION ( 'NONE',  ( 0.000000000000000000, -1.000000000000000000, 0.000000000000000000 ) ) ;
#32870 = ORIENTED_EDGE ( 'NONE', *, *, #37397, .F. ) ;
#32871 = ORIENTED_EDGE ( 'NONE', *, *, #43711, .F. ) ;
#32872 = ITEM_DEFINED_TRANSFORMATION ( 'NONE', 'NONE', #30780,  #30773 ) ;
#32873 = DIRECTION ( 'NONE',  ( -1.000000000000000000, 5.326388832052271710E-25, -1.587271980518778491E-16 ) ) ;
#32874 = DIRECTION ( 'NONE',  ( -1.000000000000000000, 0.000000000000000000, -0.000000000000000000 ) ) ;
#32875 =( BOUNDED_CURVE ( )  B_SPLINE_CURVE ( 3, ( #8062, #32160, #23701, #43943 ),
 .UNSPECIFIED., .F., .F. ) 
 B_SPLINE_CURVE_WITH_KNOTS ( ( 4, 4 ),
 ( 3.141592653589793116, 4.712388980384689674 ),
 .UNSPECIFIED. ) 
 CURVE ( )  GEOMETRIC_REPRESENTATION_ITEM ( )  RATIONAL_B_SPLINE_CURVE ( ( 1.000000000000000000, 0.8047378541243649375, 0.8047378541243649375, 1.000000000000000000 ) ) 
 REPRESENTATION_ITEM ( '' )  );
#32876 = LINE ( 'NONE', #17211, #31439 ) ;
#32877 = CARTESIAN_POINT ( 'NONE',  ( -47.23269937569316568, 16.43609759007082616, -2.408242355805840784 ) ) ;
#32878 = EDGE_LOOP ( 'NONE', ( #6296, #5317, #37890, #6641 ) ) ;
#32879 = CARTESIAN_POINT ( 'NONE',  ( 19.52505477809945944, 36.96330698207086840, 8.846626183609803462 ) ) ;
#32880 = CARTESIAN_POINT ( 'NONE',  ( -32.43949840348904701, -7.871562655726274116, -9.367992836599954742 ) ) ;
#32881 = LINE ( 'NONE', #36225, #23352 ) ;
#32882 = VECTOR ( 'NONE', #8596, 1000.000000000000000 ) ;
#32883 = ORIENTED_EDGE ( 'NONE', *, *, #20381, .F. ) ;
#32884 = CARTESIAN_POINT ( 'NONE',  ( -168.4459734468149463, 0.000000000000000000, 2.568287556927978166 ) ) ;
#32885 = ORIENTED_EDGE ( 'NONE', *, *, #15510, .F. ) ;
#32886 = CARTESIAN_POINT ( 'NONE',  ( 34.38425513258721367, -36.82177522737821107, 8.807470649214879543 ) ) ;
#32887 = ORIENTED_EDGE ( 'NONE', *, *, #23419, .F. ) ;
#32888 = PLANE ( 'NONE',  #18847 ) ;
#32889 = AXIS2_PLACEMENT_3D ( 'NONE', #50577, #8047, #46733 ) ;
#32890 = CARTESIAN_POINT ( 'NONE',  ( -204.9459734468148895, 1.025126265847089657, -120.9317124430720440 ) ) ;
#32891 = VECTOR ( 'NONE', #45263, 1000.000000000000000 ) ;
#32892 = LINE ( 'NONE', #5414, #10953 ) ;
#32893 = EDGE_LOOP ( 'NONE', ( #25901, #17691, #2328, #15498 ) ) ;
#32894 = EDGE_CURVE ( 'NONE', #9162, #13539, #34269, .T. ) ;
#32896 = CARTESIAN_POINT ( 'NONE',  ( 0.000000000000000000, 0.000000000000000000, 900.0000000000000000 ) ) ;
#32895 = B_SPLINE_CURVE_WITH_KNOTS ( 'NONE', 3,
 ( #1842, #40341, #28536, #47736 ),
 .UNSPECIFIED., .F., .F.,
 ( 4, 4 ),
 ( 0.001248798139576341119, 0.001653158300360187301 ),
 .UNSPECIFIED. ) ;
#32897 = EDGE_LOOP ( 'NONE', ( #22716, #8358, #13593, #47730 ) ) ;
#32898 = DIRECTION ( 'NONE',  ( 0.000000000000000000, 0.000000000000000000, 1.000000000000000000 ) ) ;
#32899 = CARTESIAN_POINT ( 'NONE',  ( 111.5540265531850679, 0.000000000000000000, 165.0000000000000000 ) ) ;
#32900 = CARTESIAN_POINT ( 'NONE',  ( 195.0540265531851105, 2.143131898507880377E-16, 159.0682875569279702 ) ) ;
#32901 = FACE_OUTER_BOUND ( 'NONE', #7856, .T. ) ;
#32902 = CARTESIAN_POINT ( 'NONE',  ( -0.3862712429686977478, 1.188820645368937390, -3.333333333333333481 ) ) ;
#32903 = ORIENTED_EDGE ( 'NONE', *, *, #28660, .T. ) ;
#32904 = ORIENTED_EDGE ( 'NONE', *, *, #36038, .F. ) ;
#32905 = CARTESIAN_POINT ( 'NONE',  ( 356.0000000000000568, 185.0000000000001137, 359.9999999999998295 ) ) ;
#32906 = EDGE_CURVE ( 'NONE', #24906, #10600, #48008, .T. ) ;
#32907 = EDGE_LOOP ( 'NONE', ( #45090, #30099, #19319, #46775, #19579, #46848 ) ) ;
#32908 = EDGE_CURVE ( 'NONE', #18422, #24013, #31113, .T. ) ;
#32909 = CARTESIAN_POINT ( 'NONE',  ( 181.0000000000000000, -7.999999999999952038, -340.0000000000001137 ) ) ;
#32910 = FACE_OUTER_BOUND ( 'NONE', #8411, .T. ) ;
#32911 = ORIENTED_EDGE ( 'NONE', *, *, #10431, .F. ) ;
#32912 = DIRECTION ( 'NONE',  ( 0.000000000000000000, 0.000000000000000000, -1.000000000000000000 ) ) ;
#32913 = AXIS2_PLACEMENT_3D ( 'NONE', #9918, #33294, #22230 ) ;
#32914 = EDGE_CURVE ( 'NONE', #45083, #42215, #8550, .T. ) ;
#32915 = DIRECTION ( 'NONE',  ( 0.000000000000000000, 1.000000000000000000, 7.004339610132985974E-48 ) ) ;
#32916 = ORIENTED_EDGE ( 'NONE', *, *, #5750, .T. ) ;
#32917 = CARTESIAN_POINT ( 'NONE',  ( 339.9999999999999432, -169.0000000000001137, -344.0000000000002842 ) ) ;
#32918 = CARTESIAN_POINT ( 'NONE',  ( -1.424123654778022274, -0.3625862473323341328, 9.958264684458713489 ) ) ;
#32919 = AXIS2_PLACEMENT_3D ( 'NONE', #25095, #48634, #33047 ) ;
#32920 = EDGE_CURVE ( 'NONE', #7457, #48700, #36420, .T. ) ;
#32921 = CARTESIAN_POINT ( 'NONE',  ( 224.9999999999999716, -164.9999999999999716, 474.9999999999998863 ) ) ;
#32922 = EDGE_CURVE ( 'NONE', #36821, #23935, #3212, .T. ) ;
#32923 = CARTESIAN_POINT ( 'NONE',  ( -14.49999999999999822, 12.98684210526315930, 19.37312575500900280 ) ) ;
#32924 = ORIENTED_EDGE ( 'NONE', *, *, #24897, .F. ) ;
#32925 = ORIENTED_EDGE ( 'NONE', *, *, #23807, .F. ) ;
#32926 = ORIENTED_EDGE ( 'NONE', *, *, #9025, .F. ) ;
#32927 = CARTESIAN_POINT ( 'NONE',  ( 151.5540265531850537, 0.000000000000000000, -40.93171244307202983 ) ) ;
#32928 = EDGE_CURVE ( 'NONE', #41902, #46801, #1260, .T. ) ;
#32929 = CARTESIAN_POINT ( 'NONE',  ( -119.9999999999987921, 17.00000000000000000, 5.000000000000004441 ) ) ;
#32930 = DIRECTION ( 'NONE',  ( 0.000000000000000000, 0.000000000000000000, 1.000000000000000000 ) ) ;
#32931 = CARTESIAN_POINT ( 'NONE',  ( 80.00000000000186162, 17.00000000000000000, 90.00000000000000000 ) ) ;
#32932 = VECTOR ( 'NONE', #13682, 1000.000000000000000 ) ;
#32933 = ORIENTED_EDGE ( 'NONE', *, *, #36517, .F. ) ;
#32934 = LINE ( 'NONE', #17263, #8663 ) ;
#32935 = VERTEX_POINT ( 'NONE', #21244 ) ;
#32936 =( LENGTH_UNIT ( ) NAMED_UNIT ( * ) SI_UNIT ( .MILLI., .METRE. ) );
#32937 = CARTESIAN_POINT ( 'NONE',  ( -351.8129087874521588, 159.2880105690400399, 224.7724958161647635 ) ) ;
#32938 =( BOUNDED_CURVE ( )  B_SPLINE_CURVE ( 3, ( #7160, #10498, #42304, #18690 ),
 .UNSPECIFIED., .F., .F. ) 
 B_SPLINE_CURVE_WITH_KNOTS ( ( 4, 4 ),
 ( 4.712388980384689674, 6.283185307179586232 ),
 .UNSPECIFIED. ) 
 CURVE ( )  GEOMETRIC_REPRESENTATION_ITEM ( )  RATIONAL_B_SPLINE_CURVE ( ( 1.000000000000000000, 0.8047378541243649375, 0.8047378541243649375, 1.000000000000000000 ) ) 
 REPRESENTATION_ITEM ( '' )  );
#32939 = CARTESIAN_POINT ( 'NONE',  ( -114.9999999999984652, 16.00000000000000000, 35.00000000000000000 ) ) ;
#32940 = DIRECTION ( 'NONE',  ( 0.000000000000000000, 0.000000000000000000, -1.000000000000000000 ) ) ;
#32941 = LINE ( 'NONE', #2128, #47084 ) ;
#32942 = CARTESIAN_POINT ( 'NONE',  ( 0.3656201545664388708, -2.182515578491310393, 9.881002359080277131 ) ) ;
#32943 = LINE ( 'NONE', #13408, #36300 ) ;
#32944 = VERTEX_POINT ( 'NONE', #20999 ) ;
#32945 = CARTESIAN_POINT ( 'NONE',  ( -19.99999999999783995, 16.00000000000000000, 95.00000000000000000 ) ) ;
#32946 =( BOUNDED_CURVE ( )  B_SPLINE_CURVE ( 3, ( #40129, #47276, #47772, #48023 ),
 .UNSPECIFIED., .F., .F. ) 
 B_SPLINE_CURVE_WITH_KNOTS ( ( 4, 4 ),
 ( 4.712388980384689674, 6.283185307179586232 ),
 .UNSPECIFIED. ) 
 CURVE ( )  GEOMETRIC_REPRESENTATION_ITEM ( )  RATIONAL_B_SPLINE_CURVE ( ( 1.000000000000000000, 0.8047378541243649375, 0.8047378541243649375, 1.000000000000000000 ) ) 
 REPRESENTATION_ITEM ( '' )  );
#32947 = DIRECTION ( 'NONE',  ( -0.000000000000000000, -0.000000000000000000, -1.000000000000000000 ) ) ;
#32948 = DIRECTION ( 'NONE',  ( -1.000000000000000000, 0.000000000000000000, 1.586032892321651989E-16 ) ) ;
#32949 = CARTESIAN_POINT ( 'NONE',  ( 0.1287570809895575430, 0.3962735484563150168, 10.00000000000000000 ) ) ;
#32950 = EDGE_LOOP ( 'NONE', ( #36326, #13459, #30876, #28472 ) ) ;
#32951 = FACE_OUTER_BOUND ( 'NONE', #17452, .T. ) ;
#32952 = ORIENTED_EDGE ( 'NONE', *, *, #4484, .T. ) ;
#32954 = EDGE_CURVE ( 'NONE', #49618, #30042, #33973, .T. ) ;
#32953 = CARTESIAN_POINT ( 'NONE',  ( 135.0000000000012790, 16.00000000000000000, 5.000000000000004441 ) ) ;
#32955 = VECTOR ( 'NONE', #34433, 1000.000000000000000 ) ;
#32956 = CARTESIAN_POINT ( 'NONE',  ( -6.695973446814940111, 1.750000000000024203, 120.8182875569279702 ) ) ;
#32957 = CARTESIAN_POINT ( 'NONE',  ( 71.55402655318505367, 0.000000000000000000, 82.56828755692799859 ) ) ;
#32958 = EDGE_CURVE ( 'NONE', #16715, #34606, #17397, .T. ) ;
#32959 = ORIENTED_EDGE ( 'NONE', *, *, #19286, .F. ) ;
#32960 = VECTOR ( 'NONE', #28760, 1000.000000000000000 ) ;
#32961 = DIRECTION ( 'NONE',  ( 0.000000000000000000, 0.000000000000000000, -1.000000000000000000 ) ) ;
#32962 = CARTESIAN_POINT ( 'NONE',  ( 1.011271242968694084, -0.7347315653655782652, 10.00000000000000000 ) ) ;
#32963 = CARTESIAN_POINT ( 'NONE',  ( 360.0000000000000000, -169.0000000000000568, -344.0000000000002842 ) ) ;
#32964 = CARTESIAN_POINT ( 'NONE',  ( -208.4459734468149463, 0.000000000000000000, -40.93171244307202983 ) ) ;
#32965 = ORIENTED_EDGE ( 'NONE', *, *, #27381, .F. ) ;
#32966 = ORIENTED_EDGE ( 'NONE', *, *, #23470, .F. ) ;
#32967 = CARTESIAN_POINT ( 'NONE',  ( 151.5540265531850537, -1.025126265847089879, -117.4317124430720156 ) ) ;
#32968 = CARTESIAN_POINT ( 'NONE',  ( 47.22310614333766665, 16.46562252335956344, -3.760136334089591248 ) ) ;
#32969 = VERTEX_POINT ( 'NONE', #32816 ) ;
#32970 = ORIENTED_EDGE ( 'NONE', *, *, #23160, .F. ) ;
#32971 = FACE_OUTER_BOUND ( 'NONE', #408, .T. ) ;
#32972 = LINE ( 'NONE', #13449, #47021 ) ;
#32973 = DIRECTION ( 'NONE',  ( 0.000000000000000000, -1.000000000000000000, 3.469446951953611033E-15 ) ) ;
#32974 = CARTESIAN_POINT ( 'NONE',  ( 169.0000000000000284, 175.0000000000000284, 359.9999999999998863 ) ) ;
#32975 = ORIENTED_EDGE ( 'NONE', *, *, #14234, .T. ) ;
#32976 = VERTEX_POINT ( 'NONE', #41694 ) ;
#32977 = ORIENTED_EDGE ( 'NONE', *, *, #16468, .F. ) ;
#32978 = SPHERICAL_SURFACE ( 'NONE', #2930, 0.5000000000000000000 ) ;
#32979 = DIRECTION ( 'NONE',  ( -1.156482317317871478E-16, 1.000000000000000000, 0.000000000000000000 ) ) ;
#32980 = ORIENTED_EDGE ( 'NONE', *, *, #7705, .T. ) ;
#32981 = VECTOR ( 'NONE', #41738, 1000.000000000000000 ) ;
#32982 = ORIENTED_EDGE ( 'NONE', *, *, #26302, .F. ) ;
#32983 = EDGE_CURVE ( 'NONE', #1474, #40766, #6546, .T. ) ;
#32984 = CARTESIAN_POINT ( 'NONE',  ( 111.5540265531850537, 0.000000000000000000, 162.5682875569279702 ) ) ;
#32985 = VECTOR ( 'NONE', #22423, 1000.000000000000000 ) ;
#32986 = DIRECTION ( 'NONE',  ( -1.000000000000000000, 0.000000000000000000, 0.000000000000000000 ) ) ;
#32987 = ORIENTED_EDGE ( 'NONE', *, *, #40948, .T. ) ;
#32988 = ORIENTED_EDGE ( 'NONE', *, *, #47491, .T. ) ;
#32989 = VECTOR ( 'NONE', #26809, 1000.000000000000000 ) ;
#32990 = CARTESIAN_POINT ( 'NONE',  ( 7.499999999999944045, -224.9999999999999716, -240.0000000000000000 ) ) ;
#32991 = CARTESIAN_POINT ( 'NONE',  ( 6.204997580903516941, 7.611558401714507482, 229.0000000000000000 ) ) ;
#32992 = ORIENTED_EDGE ( 'NONE', *, *, #25841, .F. ) ;
#32993 = CARTESIAN_POINT ( 'NONE',  ( -165.2900739183569954, -61.66198943095990614, -18.55102910462098365 ) ) ;
#32994 = LINE ( 'NONE', #16825, #17234 ) ;
#32995 = CARTESIAN_POINT ( 'NONE',  ( 164.9999999999999716, 17.00000000000000000, 34.99999999999999289 ) ) ;
#32996 = DIRECTION ( 'NONE',  ( 0.000000000000000000, 0.000000000000000000, -1.000000000000000000 ) ) ;
#32997 = VECTOR ( 'NONE', #34674, 1000.000000000000000 ) ;
#32998 = CARTESIAN_POINT ( 'NONE',  ( -45.67084718096785423, -1.750000000000010436, -120.2068387089191219 ) ) ;
#32999 = ORIENTED_EDGE ( 'NONE', *, *, #18294, .T. ) ;
#33000 = CARTESIAN_POINT ( 'NONE',  ( -0.3862712429686809279, -1.188820645368943163, -10.00000000000000000 ) ) ;
#33001 = CARTESIAN_POINT ( 'NONE',  ( 210.0000000000000568, 0.000000000000000000, -117.4317124430720298 ) ) ;
#33002 = B_SPLINE_SURFACE_WITH_KNOTS ( 'NONE', 3, 3, ( 
 ( #35938, #1285, #32589, #8479 ),
 ( #43860, #776, #5110, #47669 ),
 ( #16936, #17175, #31836, #24629 ),
 ( #12821, #8975, #12558, #48426 ) ),
 .UNSPECIFIED., .F., .F., .F.,
 ( 4, 4 ),
 ( 4, 4 ),
 ( 0.000000000000000000, 1.000000000000000000 ),
 ( 0.000000000000000000, 1.000000000000000000 ),
 .UNSPECIFIED. ) ;
#33003 = CARTESIAN_POINT ( 'NONE',  ( -204.9459734468149463, 2.143131898507880377E-16, -0.9317124430720247208 ) ) ;
#33004 = CARTESIAN_POINT ( 'NONE',  ( -225.0000000000000568, 164.9999999999999716, 132.0000000000000000 ) ) ;
#33005 = CARTESIAN_POINT ( 'NONE',  ( -164.9999999999981526, 17.00000000000000000, 90.00000000000000000 ) ) ;
#33006 = CARTESIAN_POINT ( 'NONE',  ( 8.277096487746778308, -33.14818118907697198, 7.455576670931136185 ) ) ;
#33007 = CARTESIAN_POINT ( 'NONE',  ( 0.000000000000000000, 0.000000000000000000, 10.00000000000000000 ) ) ;
#33008 = AXIS2_PLACEMENT_3D ( 'NONE', #11120, #31395, #49805 ) ;
#33009 = CARTESIAN_POINT ( 'NONE',  ( 153.3040265531850537, 1.750000000000009992, -159.1817124430720298 ) ) ;
#33010 = VERTEX_POINT ( 'NONE', #27827 ) ;
#33011 = CARTESIAN_POINT ( 'NONE',  ( -14.49999999999999822, 13.48684210526315930, -19.37312575500899570 ) ) ;
#33012 = LINE ( 'NONE', #48598, #4118 ) ;
#33013=STYLED_ITEM('',(#50782),#5698);
#33014 = CARTESIAN_POINT ( 'NONE',  ( -128.4459734468149463, 1.025126265847081219, 2.568287556927973281 ) ) ;
#33015 = CARTESIAN_POINT ( 'NONE',  ( 73.30402655318508209, 1.750000000000009992, 0.8182875569279768335 ) ) ;
#33016 = CARTESIAN_POINT ( 'NONE',  ( 32.27890028733795447, 1.750000000000009548, 39.79316129108089228 ) ) ;
#33017 = ORIENTED_EDGE ( 'NONE', *, *, #12431, .T. ) ;
#33018 = CARTESIAN_POINT ( 'NONE',  ( 350.0000000000000000, 181.0000000000000284, -358.0000000000002274 ) ) ;
#33019 = EDGE_LOOP ( 'NONE', ( #20744, #23824, #26110, #49724, #16815, #32833 ) ) ;
#33020 = CARTESIAN_POINT ( 'NONE',  ( -0.1287570809895602630, -0.3962735484563142396, 10.00000000000000000 ) ) ;
#33021 = VECTOR ( 'NONE', #573, 1000.000000000000000 ) ;
#33022 = CARTESIAN_POINT ( 'NONE',  ( -48.44597344681495343, 0.000000000000000000, -0.9317124430720247208 ) ) ;
#33023 = ORIENTED_EDGE ( 'NONE', *, *, #36838, .F. ) ;
#33024 = CIRCLE ( 'NONE', #13370, 1.750000000000015543 ) ;
#33025 = CARTESIAN_POINT ( 'NONE',  ( 113.3040265531850537, 0.000000000000000000, 165.0000000000000000 ) ) ;
#33026 = LINE ( 'NONE', #13501, #43759 ) ;
#33027 = ORIENTED_EDGE ( 'NONE', *, *, #3855, .F. ) ;
#33028 = ORIENTED_EDGE ( 'NONE', *, *, #38493, .F. ) ;
#33029 = CARTESIAN_POINT ( 'NONE',  ( -215.0000000000000568, 164.9999999999999716, 10.00000000000000000 ) ) ;
#33030 = CARTESIAN_POINT ( 'NONE',  ( 16.52264463346132572, -2.779753662172757878, 9.403735324607438884 ) ) ;
#33031 = CARTESIAN_POINT ( 'NONE',  ( -208.4459734468149463, 0.000000000000000000, 165.0000000000000000 ) ) ;
#33032 = ORIENTED_EDGE ( 'NONE', *, *, #3386, .T. ) ;
#33033 = DIRECTION ( 'NONE',  ( 0.000000000000000000, 0.000000000000000000, 1.000000000000000000 ) ) ;
#33034 = CARTESIAN_POINT ( 'NONE',  ( 168.9999999999999716, -252.5000000000000000, -114.9999999999999574 ) ) ;
#33035 = ORIENTED_EDGE ( 'NONE', *, *, #14239, .T. ) ;
#33036 = ORIENTED_EDGE ( 'NONE', *, *, #16338, .F. ) ;
#33037 = ORIENTED_EDGE ( 'NONE', *, *, #9816, .T. ) ;
#33038 = FACE_OUTER_BOUND ( 'NONE', #349, .T. ) ;
#33039 = ADVANCED_FACE ( 'NONE', ( #11164 ), #31845, .T. ) ;
#33040 = CARTESIAN_POINT ( 'NONE',  ( -1.901953004002570502, -1.028591558669202488, 9.885585981620943485 ) ) ;
#33041 = EDGE_LOOP ( 'NONE', ( #36314, #27809, #37934, #33023 ) ) ;
#33042 = EDGE_CURVE ( 'NONE', #15322, #27386, #16027, .T. ) ;
#33043 = CARTESIAN_POINT ( 'NONE',  ( -10.70590866674912967, 12.76446523155714985, -3.546734833711462365 ) ) ;
#33044 = CARTESIAN_POINT ( 'NONE',  ( -4.945973446814916130, 1.025126265847097651, -117.4317124430720014 ) ) ;
#33045 = EDGE_CURVE ( 'NONE', #50559, #35762, #38623, .T. ) ;
#33046 = CARTESIAN_POINT ( 'NONE',  ( -8.445973446814976526, 0.000000000000000000, 165.0000000000000000 ) ) ;
#33047 = DIRECTION ( 'NONE',  ( 0.000000000000000000, 0.000000000000000000, 1.000000000000000000 ) ) ;
#33048 = AXIS2_PLACEMENT_3D ( 'NONE', #14047, #6614, #14306 ) ;
#33049 = DIRECTION ( 'NONE',  ( 0.000000000000000000, 0.3790464617558786942, -0.9253776417389547593 ) ) ;
#33050 = VECTOR ( 'NONE', #33128, 1000.000000000000000 ) ;
#33051 = CARTESIAN_POINT ( 'NONE',  ( -64.99999999999940314, 17.00000000000000000, -54.99999999999999289 ) ) ;
#33052 = CYLINDRICAL_SURFACE ( 'NONE', #48524, 1.750000000000001554 ) ;
#33053 = EDGE_CURVE ( 'NONE', #14054, #24991, #3442, .T. ) ;
#33054 = CARTESIAN_POINT ( 'NONE',  ( 0.000000000000000000, -164.9999999999999716, 0.000000000000000000 ) ) ;
#33055 = AXIS2_PLACEMENT_3D ( 'NONE', #44327, #21495, #36687 ) ;
#33056 = ADVANCED_FACE ( 'NONE', ( #34784 ), #15759, .F. ) ;
#33057 = CARTESIAN_POINT ( 'NONE',  ( 33.01266944765062306, -5.813986777101467496, 1.847720168420772691 ) ) ;
#33058 = VECTOR ( 'NONE', #19981, 1000.000000000000000 ) ;
#33059 = DIRECTION ( 'NONE',  ( 0.000000000000000000, 0.000000000000000000, -1.000000000000000000 ) ) ;
#33060 = VERTEX_POINT ( 'NONE', #46761 ) ;
#33061 = DIRECTION ( 'NONE',  ( 2.168404344971008627E-19, -0.7071067811865474617, -0.7071067811865475727 ) ) ;
#33062 = CARTESIAN_POINT ( 'NONE',  ( -85.67084718096784002, -1.750000000000009326, -158.1565861772249377 ) ) ;
#33063 = DIRECTION ( 'NONE',  ( 0.000000000000000000, 0.000000000000000000, -1.000000000000000000 ) ) ;
#33064 = EDGE_CURVE ( 'NONE', #1662, #576, #7828, .T. ) ;
#33065 = EDGE_CURVE ( 'NONE', #34472, #1515, #43366, .T. ) ;
#33066 = DIRECTION ( 'NONE',  ( 1.000000000000000000, 0.000000000000000000, 0.000000000000000000 ) ) ;
#33067 =( BOUNDED_CURVE ( )  B_SPLINE_CURVE ( 3, ( #42475, #19129, #31212, #46549 ),
 .UNSPECIFIED., .F., .F. ) 
 B_SPLINE_CURVE_WITH_KNOTS ( ( 4, 4 ),
 ( 1.570796326794896558, 3.141592653589793116 ),
 .UNSPECIFIED. ) 
 CURVE ( )  GEOMETRIC_REPRESENTATION_ITEM ( )  RATIONAL_B_SPLINE_CURVE ( ( 1.000000000000000000, 0.8047378541243649375, 0.8047378541243649375, 1.000000000000000000 ) ) 
 REPRESENTATION_ITEM ( '' )  );
#33069 = ORIENTED_EDGE ( 'NONE', *, *, #27524, .T. ) ;
#33068 = EDGE_CURVE ( 'NONE', #30056, #46777, #14627, .T. ) ;
#33070 = CARTESIAN_POINT ( 'NONE',  ( -124.9459734468149321, 1.025126265847081886, -80.93171244307201562 ) ) ;
#33071 = ADVANCED_FACE ( 'NONE', ( #42691 ), #46515, .F. ) ;
#33072 = CARTESIAN_POINT ( 'NONE',  ( -3.630679331413954714, -37.33064849398144958, -8.600750091277037157 ) ) ;
#33073 = ORIENTED_EDGE ( 'NONE', *, *, #50257, .T. ) ;
#33074 = ADVANCED_FACE ( 'NONE', ( #30665 ), #38881, .T. ) ;
#33075 = CARTESIAN_POINT ( 'NONE',  ( 33.01266944765062306, -5.813986777101467496, 1.847720168420772691 ) ) ;
#33076 = LINE ( 'NONE', #49670, #42870 ) ;
#33077 = CARTESIAN_POINT ( 'NONE',  ( -69.99999999999783995, 17.00000000000000000, 95.00000000000000000 ) ) ;
#33078 =( BOUNDED_CURVE ( )  B_SPLINE_CURVE ( 3, ( #35062, #22717, #38388, #3200 ),
 .UNSPECIFIED., .F., .F. ) 
 B_SPLINE_CURVE_WITH_KNOTS ( ( 4, 4 ),
 ( 1.570796326794891673, 2.917357902480690601 ),
 .UNSPECIFIED. ) 
 CURVE ( )  GEOMETRIC_REPRESENTATION_ITEM ( )  RATIONAL_B_SPLINE_CURVE ( ( 1.000000000000000000, 0.8545200852688804583, 0.8545200852688804583, 1.000000000000000000 ) ) 
 REPRESENTATION_ITEM ( '' )  );
#33079 = EDGE_CURVE ( 'NONE', #11140, #5897, #28078, .T. ) ;
#33080 = VERTEX_POINT ( 'NONE', #126 ) ;
#33081 = DIRECTION ( 'NONE',  ( 0.000000000000000000, -1.000000000000000000, 0.000000000000000000 ) ) ;
#33082 = VERTEX_POINT ( 'NONE', #11924 ) ;
#33083 = ORIENTED_EDGE ( 'NONE', *, *, #43378, .F. ) ;
#33084 = FACE_OUTER_BOUND ( 'NONE', #6514, .T. ) ;
#33085 = ORIENTED_EDGE ( 'NONE', *, *, #14351, .T. ) ;
#33086 = CARTESIAN_POINT ( 'NONE',  ( 191.5540265531850537, -1.025126265847089657, 79.06828755692797017 ) ) ;
#33087 = CARTESIAN_POINT ( 'NONE',  ( 1.011271242968688311, -0.7347315653655855927, 10.00000000000000000 ) ) ;
#33088 = VECTOR ( 'NONE', #29033, 1000.000000000000000 ) ;
#33089 = VERTEX_POINT ( 'NONE', #43215 ) ;
#33090 = CARTESIAN_POINT ( 'NONE',  ( -64.99999999999909051, 17.00000000000000000, 0.000000000000000000 ) ) ;
#33091 = CARTESIAN_POINT ( 'NONE',  ( 342.0000000000000568, 177.9999999999999432, -3.000000000000002665 ) ) ;
#33092 = VECTOR ( 'NONE', #5584, 1000.000000000000000 ) ;
#33093 = CARTESIAN_POINT ( 'NONE',  ( 355.9999999999999432, -185.0000000000001421, -360.0000000000003411 ) ) ;
#33094 =( BOUNDED_CURVE ( )  B_SPLINE_CURVE ( 3, ( #48115, #36129, #1479, #40216 ),
 .UNSPECIFIED., .F., .F. ) 
 B_SPLINE_CURVE_WITH_KNOTS ( ( 4, 4 ),
 ( 3.141592653589793116, 4.712388980384689674 ),
 .UNSPECIFIED. ) 
 CURVE ( )  GEOMETRIC_REPRESENTATION_ITEM ( )  RATIONAL_B_SPLINE_CURVE ( ( 1.000000000000000000, 0.8047378541243649375, 0.8047378541243649375, 1.000000000000000000 ) ) 
 REPRESENTATION_ITEM ( '' )  );
#33095 = CARTESIAN_POINT ( 'NONE',  ( 228.9999999999999716, -169.9999999999999716, 4.999999999999616307 ) ) ;
#33096 = EDGE_CURVE ( 'NONE', #48718, #6330, #29456, .T. ) ;
#33097 = ORIENTED_EDGE ( 'NONE', *, *, #17552, .F. ) ;
#33098 = AXIS2_PLACEMENT_3D ( 'NONE', #19226, #30541, #26429 ) ;
#33099 = CARTESIAN_POINT ( 'NONE',  ( -54.99999999999997868, -52.50000000000000711, 5.000000000000000000 ) ) ;
#33100 = AXIS2_PLACEMENT_3D ( 'NONE', #1501, #36414, #28194 ) ;
#33101 = ADVANCED_FACE ( 'NONE', ( #24990, #32951 ), #1638, .T. ) ;
#33102 = VERTEX_POINT ( 'NONE', #43710 ) ;
#33103 = ADVANCED_FACE ( 'NONE', ( #43462 ), #36803, .F. ) ;
#33104 = DIRECTION ( 'NONE',  ( -1.000000000000000000, -0.000000000000000000, -0.000000000000000000 ) ) ;
#33105 = DIRECTION ( 'NONE',  ( 0.000000000000000000, 0.000000000000000000, -1.000000000000000000 ) ) ;
#33106 = ORIENTED_EDGE ( 'NONE', *, *, #5559, .T. ) ;
#33107 = ORIENTED_EDGE ( 'NONE', *, *, #9855, .T. ) ;
#33108 = VERTEX_POINT ( 'NONE', #16530 ) ;
#33109 = CARTESIAN_POINT ( 'NONE',  ( 195.0540265531851105, 2.143131898507880377E-16, 165.0000000000000000 ) ) ;
#33110 = CARTESIAN_POINT ( 'NONE',  ( 14.49999999999999822, 12.98684210526315930, 19.37312575500900280 ) ) ;
#33111 = PRODUCT ( 'fann', 'fann', '', ( #28504 ) ) ;
#33112 = ORIENTED_EDGE ( 'NONE', *, *, #43776, .T. ) ;
#33113 = EDGE_CURVE ( 'NONE', #13147, #38490, #25135, .T. ) ;
#33114 = CARTESIAN_POINT ( 'NONE',  ( 1.011271242968683648, 0.7347315653655930312, 10.00000000000000000 ) ) ;
#33115 = CARTESIAN_POINT ( 'NONE',  ( -0.6595498452743703277, 16.59563386392009576, 3.266473740018926541 ) ) ;
#33116 = CARTESIAN_POINT ( 'NONE',  ( 355.9999999999999432, 174.9999999999996589, -358.0000000000003411 ) ) ;
#33117 = AXIS2_PLACEMENT_3D ( 'NONE', #26031, #17567, #33738 ) ;
#33118 = ORIENTED_EDGE ( 'NONE', *, *, #24834, .F. ) ;
#33119 = DIRECTION ( 'NONE',  ( -1.000000000000000000, 0.000000000000000000, 0.000000000000000000 ) ) ;
#33120 = CARTESIAN_POINT ( 'NONE',  ( 153.3040265531850537, -1.750000000000010658, -79.18171244307201562 ) ) ;
#33121 = CARTESIAN_POINT ( 'NONE',  ( -30.12518629743573584, -14.70074613238887551, 1.847720168420772691 ) ) ;
#33122 = EDGE_CURVE ( 'NONE', #2781, #43783, #32440, .T. ) ;
#33123 = ORIENTED_EDGE ( 'NONE', *, *, #31652, .T. ) ;
#33124 = DIRECTION ( 'NONE',  ( -0.000000000000000000, -0.000000000000000000, -1.000000000000000000 ) ) ;
#33125 = LINE ( 'NONE', #5141, #9469 ) ;
#33126 = VECTOR ( 'NONE', #20441, 1000.000000000000000 ) ;
#33127 = ADVANCED_FACE ( 'NONE', ( #36042 ), #28829, .F. ) ;
#33128 = DIRECTION ( 'NONE',  ( 0.000000000000000000, 0.000000000000000000, 1.000000000000000000 ) ) ;
#33129 = CARTESIAN_POINT ( 'NONE',  ( -166.6959734468149463, 0.000000000000000000, 165.0000000000000000 ) ) ;
#33130 = EDGE_LOOP ( 'NONE', ( #39002, #37225, #19004, #36994, #49061, #421 ) ) ;
#33131 = CARTESIAN_POINT ( 'NONE',  ( 17.34922095635755568, 33.24536858281893359, 8.914903342594564961 ) ) ;
#33132 = CIRCLE ( 'NONE', #44569, 50.00000000000000000 ) ;
#33133 = CARTESIAN_POINT ( 'NONE',  ( -204.9459734468149463, 2.143131898507880377E-16, 82.56828755692798438 ) ) ;
#33134 = FACE_OUTER_BOUND ( 'NONE', #20817, .T. ) ;
#33135 = CARTESIAN_POINT ( 'NONE',  ( -84.94597344681494633, 2.143131898507880377E-16, 79.06828755692797017 ) ) ;
#33136 = VECTOR ( 'NONE', #30219, 1000.000000000000000 ) ;
#33137 = CARTESIAN_POINT ( 'NONE',  ( 191.5540265531850537, 1.025126265847089435, -40.93171244307204404 ) ) ;
#33139 = ORIENTED_EDGE ( 'NONE', *, *, #17045, .F. ) ;
#33138 = EDGE_CURVE ( 'NONE', #19018, #49333, #28073, .T. ) ;
#33140 = CARTESIAN_POINT ( 'NONE',  ( 358.3431457505075741, -185.0000000000000000, 359.9999999999997726 ) ) ;
#33141 = ADVANCED_FACE ( 'NONE', ( #47778 ), #28573, .T. ) ;
#33142 = VERTEX_POINT ( 'NONE', #36301 ) ;
#33143 = PLANE ( 'NONE',  #13869 ) ;
#33144 = VERTEX_POINT ( 'NONE', #1139 ) ;
#33145 = EDGE_CURVE ( 'NONE', #44889, #43082, #43109, .T. ) ;
#33146 = CARTESIAN_POINT ( 'NONE',  ( 154.1026953830863420, 103.9380105690400597, -17.65743994998277699 ) ) ;
#33147 = CARTESIAN_POINT ( 'NONE',  ( 210.0000000000000568, 0.000000000000000000, 160.8182875569279702 ) ) ;
#33148 = ADVANCED_FACE ( 'NONE', ( #9082 ), #35806, .F. ) ;
#33149 = CARTESIAN_POINT ( 'NONE',  ( -24.39427009666018265, -44.07992421011638129, 8.807470649214879543 ) ) ;
#33150 = VERTEX_POINT ( 'NONE', #9333 ) ;
#33151 = EDGE_CURVE ( 'NONE', #41405, #5869, #21252, .T. ) ;
#33152 = EDGE_CURVE ( 'NONE', #12938, #37443, #47535, .T. ) ;
#33153 = FACE_OUTER_BOUND ( 'NONE', #41728, .T. ) ;
#33154 = EDGE_LOOP ( 'NONE', ( #3940, #6194, #37824, #8039 ) ) ;
#33155 = DIRECTION ( 'NONE',  ( -0.000000000000000000, -0.000000000000000000, -1.000000000000000000 ) ) ;
#33156 = DIRECTION ( 'NONE',  ( -0.9770330068457271366, 0.000000000000000000, -0.2130880182788259247 ) ) ;
#33157 = CARTESIAN_POINT ( 'NONE',  ( -25.61277432017861955, 22.36370378792854297, 7.906207997025717304 ) ) ;
#33158 = LINE ( 'NONE', #28533, #20934 ) ;
#33159 = CYLINDRICAL_SURFACE ( 'NONE', #4432, 1.750000000000008438 ) ;
#33160 = ORIENTED_EDGE ( 'NONE', *, *, #35010, .T. ) ;
#33161 = EDGE_LOOP ( 'NONE', ( #28288, #25626, #21913 ) ) ;
#33162 = LINE ( 'NONE', #17242, #30858 ) ;
#33163 = EDGE_LOOP ( 'NONE', ( #23747, #12251, #5670, #31035 ) ) ;
#33164 = ADVANCED_FACE ( 'NONE', ( #39895 ), #16777, .F. ) ;
#33165 = DIRECTION ( 'NONE',  ( 0.000000000000000000, 0.000000000000000000, -1.000000000000000000 ) ) ;
#33166 = CARTESIAN_POINT ( 'NONE',  ( 153.3040265531850537, 0.000000000000000000, 165.0000000000000000 ) ) ;
#33167 = VERTEX_POINT ( 'NONE', #40391 ) ;
#33168 = CARTESIAN_POINT ( 'NONE',  ( 341.9999999999999432, -181.0000000000001421, 356.0000000000000568 ) ) ;
#33169 = AXIS2_PLACEMENT_3D ( 'NONE', #5352, #9200, #48656 ) ;
#33170 = DIRECTION ( 'NONE',  ( 0.000000000000000000, 0.000000000000000000, -1.000000000000000000 ) ) ;
#33171 = ORIENTED_EDGE ( 'NONE', *, *, #33873, .F. ) ;
#33172 = AXIS2_PLACEMENT_3D ( 'NONE', #9297, #48996, #36775 ) ;
#33173 = CARTESIAN_POINT ( 'NONE',  ( -5.670847180967843570, -1.750000000000023315, -160.2068387089191219 ) ) ;
#33174 = CARTESIAN_POINT ( 'NONE',  ( -47.23269937569316568, 16.43609759007082616, -2.408242355805840784 ) ) ;
#33175 = PLANE ( 'NONE',  #31520 ) ;
#33176 = CARTESIAN_POINT ( 'NONE',  ( -194.9999999999999432, 164.9999999999999716, 231.9999999999999147 ) ) ;
#33177 = ORIENTED_EDGE ( 'NONE', *, *, #45262, .F. ) ;
#33178 = EDGE_LOOP ( 'NONE', ( #37189, #12643, #18059, #43236 ) ) ;
#33179 = EDGE_LOOP ( 'NONE', ( #47539, #27204, #25170, #33965, #7568, #14823 ) ) ;
#33180 = CARTESIAN_POINT ( 'NONE',  ( -126.6959734468149321, 1.749999999999997335, 120.8182875569279702 ) ) ;
#33181 = CARTESIAN_POINT ( 'NONE',  ( -44.94597344681493922, 2.143131898507880377E-16, 42.56828755692798438 ) ) ;
#33182 = FACE_OUTER_BOUND ( 'NONE', #13338, .T. ) ;
#33183 = CARTESIAN_POINT ( 'NONE',  ( -4.672045878990125800, 50.00000000000000711, 1.847720168420772691 ) ) ;
#33184 = ORIENTED_EDGE ( 'NONE', *, *, #34048, .F. ) ;
#33185 = PLANE ( 'NONE',  #41391 ) ;
#33186 = ORIENTED_EDGE ( 'NONE', *, *, #23253, .T. ) ;
#33187 = CARTESIAN_POINT ( 'NONE',  ( -19.99999999999783995, 17.00000000000000000, 95.00000000000000000 ) ) ;
#33188 = CARTESIAN_POINT ( 'NONE',  ( 236.0000000000000000, -169.9999999999999716, 444.9999999999998295 ) ) ;
#33189 = LINE ( 'NONE', #44692, #28304 ) ;
#33190 = VECTOR ( 'NONE', #49274, 1000.000000000000000 ) ;
#33191 = DIRECTION ( 'NONE',  ( 0.000000000000000000, 0.000000000000000000, 1.000000000000000000 ) ) ;
#33192 = FACE_OUTER_BOUND ( 'NONE', #11906, .T. ) ;
#33193 = AXIS2_PLACEMENT_3D ( 'NONE', #47460, #16206, #31099 ) ;
#33194 = CARTESIAN_POINT ( 'NONE',  ( -127.7210997126620242, 1.749999999999996669, -0.2068387089191042749 ) ) ;
#33195 = ORIENTED_EDGE ( 'NONE', *, *, #49981, .T. ) ;
#33196 = DIRECTION ( 'NONE',  ( -1.000000000000000000, 1.445602896647339410E-16, 0.000000000000000000 ) ) ;
#33197 = DIRECTION ( 'NONE',  ( 3.172065745548403743E-16, 1.000000000000000000, 0.000000000000000000 ) ) ;
#33198 = CARTESIAN_POINT ( 'NONE',  ( -0.1473596192760168455, -1.496323530725124584, 9.936141075690080982 ) ) ;
#33199 = EDGE_CURVE ( 'NONE', #44740, #41339, #41725, .T. ) ;
#33200 = FACE_BOUND ( 'NONE', #18783, .T. ) ;
#33201 = EDGE_CURVE ( 'NONE', #39980, #14882, #35937, .T. ) ;
#33202 = ORIENTED_EDGE ( 'NONE', *, *, #47726, .F. ) ;
#33203 = AXIS2_PLACEMENT_3D ( 'NONE', #18609, #21969, #30430 ) ;
#33204 = CARTESIAN_POINT ( 'NONE',  ( -166.6959734468149463, 0.000000000000000000, 165.0000000000000000 ) ) ;
#33205 = ORIENTED_EDGE ( 'NONE', *, *, #34690, .T. ) ;
#33206 = LINE ( 'NONE', #36558, #27044 ) ;
#33207 = LINE ( 'NONE', #17286, #24187 ) ;
#33208 = ADVANCED_FACE ( 'NONE', ( #45194 ), #49782, .F. ) ;
#33209 = CARTESIAN_POINT ( 'NONE',  ( 8.019230367735008969, -14.74354227315958887, -9.233365092205394475 ) ) ;
#33210 = ADVANCED_BREP_SHAPE_REPRESENTATION ( '', ( #39479, #45486 ), #32386 ) ;
#33211 = EDGE_CURVE ( 'NONE', #31704, #20835, #45451, .T. ) ;
#33212 = EDGE_CURVE ( 'NONE', #6277, #38645, #25997, .T. ) ;
#33213 = ORIENTED_EDGE ( 'NONE', *, *, #37053, .T. ) ;
#33214 = CARTESIAN_POINT ( 'NONE',  ( 13.35436367797824353, 31.26996044524050333, 7.906207997025717304 ) ) ;
#33215 = CARTESIAN_POINT ( 'NONE',  ( -64.99999999999846523, 17.00000000000000000, 60.00000000000000000 ) ) ;
#33216 = CARTESIAN_POINT ( 'NONE',  ( 358.0000000000000000, 169.0000000000000000, -344.0000000000001137 ) ) ;
#33217 = CARTESIAN_POINT ( 'NONE',  ( 4.412346620047078893, 9.007664521157071391, 9.516222621873129839 ) ) ;
#33218 = ADVANCED_FACE ( 'NONE', ( #10346 ), #37059, .T. ) ;
#33219 = ORIENTED_EDGE ( 'NONE', *, *, #6466, .F. ) ;
#33220 = ORIENTED_EDGE ( 'NONE', *, *, #12725, .F. ) ;
#33221 = CARTESIAN_POINT ( 'NONE',  ( -3.940019464150765760, -50.00000000000000711, -8.466730184410787174 ) ) ;
#33222 = CARTESIAN_POINT ( 'NONE',  ( 73.30402655318508209, -1.750000000000010658, -79.18171244307201562 ) ) ;
#33223 = AXIS2_PLACEMENT_3D ( 'NONE', #6314, #40708, #2210 ) ;
#33224 = ORIENTED_EDGE ( 'NONE', *, *, #2361, .F. ) ;
#33225 = ORIENTED_EDGE ( 'NONE', *, *, #35125, .F. ) ;
#33226 = DIRECTION ( 'NONE',  ( -0.000000000000000000, -0.000000000000000000, -1.000000000000000000 ) ) ;
#33227 = DIRECTION ( 'NONE',  ( 0.000000000000000000, 5.664403186863042467E-17, 1.000000000000000000 ) ) ;
#33228 = CARTESIAN_POINT ( 'NONE',  ( 167.0000000000000000, -174.9999999999999716, -111.0000000000001563 ) ) ;
#33229 = LINE ( 'NONE', #17558, #42788 ) ;
#33230 = AXIS2_PLACEMENT_3D ( 'NONE', #43518, #4532, #36103 ) ;
#33231 = ORIENTED_EDGE ( 'NONE', *, *, #16697, .F. ) ;
#33232 = ORIENTED_EDGE ( 'NONE', *, *, #5097, .F. ) ;
#33233 = LINE ( 'NONE', #48815, #41442 ) ;
#33235 = AXIS2_PLACEMENT_3D ( 'NONE', #6231, #15436, #22367 ) ;
#33234 = CARTESIAN_POINT ( 'NONE',  ( 1.019713130072856355, 3.848720492505100843, 4.370690007832189750E-16 ) ) ;
#33236 = ORIENTED_EDGE ( 'NONE', *, *, #45211, .T. ) ;
#33237 = AXIS2_PLACEMENT_3D ( 'NONE', #21282, #9990, #25648 ) ;
#33238 = ORIENTED_EDGE ( 'NONE', *, *, #49753, .T. ) ;
#33239 = DIRECTION ( 'NONE',  ( 0.000000000000000000, 1.000000000000000000, 0.000000000000000000 ) ) ;
#33240 =( BOUNDED_CURVE ( )  B_SPLINE_CURVE ( 3, ( #49936, #30493, #50452, #25899 ),
 .UNSPECIFIED., .F., .F. ) 
 B_SPLINE_CURVE_WITH_KNOTS ( ( 4, 4 ),
 ( 1.570796326794896558, 3.141592653589793116 ),
 .UNSPECIFIED. ) 
 CURVE ( )  GEOMETRIC_REPRESENTATION_ITEM ( )  RATIONAL_B_SPLINE_CURVE ( ( 1.000000000000000000, 0.8047378541243649375, 0.8047378541243649375, 1.000000000000000000 ) ) 
 REPRESENTATION_ITEM ( '' )  );
#33241 = CARTESIAN_POINT ( 'NONE',  ( 360.0000000000000000, -169.0000000000001137, -344.0000000000003411 ) ) ;
#33242 = AXIS2_PLACEMENT_3D ( 'NONE', #14418, #30084, #41115 ) ;
#33243 = ORIENTED_EDGE ( 'NONE', *, *, #47892, .F. ) ;
#33244 = ORIENTED_EDGE ( 'NONE', *, *, #43065, .T. ) ;
#33245 = EDGE_CURVE ( 'NONE', #26648, #25407, #33945, .T. ) ;
#33246 = DIRECTION ( 'NONE',  ( 0.000000000000000000, 0.000000000000000000, 1.000000000000000000 ) ) ;
#33247 = LINE ( 'NONE', #48824, #10834 ) ;
#33248 = EDGE_LOOP ( 'NONE', ( #28738, #29582, #37133, #9594 ) ) ;
#33249 = DIRECTION ( 'NONE',  ( 3.172065745548403743E-16, 1.000000000000000000, 0.000000000000000000 ) ) ;
#33250 = CARTESIAN_POINT ( 'NONE',  ( 0.000000000000000000, 0.000000000000000000, 910.0000000000000000 ) ) ;
#33251 = CARTESIAN_POINT ( 'NONE',  ( 85.00000000000056843, 17.00000000000000000, -54.99999999999999289 ) ) ;
#33252 = DIRECTION ( 'NONE',  ( 1.000000000000000000, 0.000000000000000000, 0.000000000000000000 ) ) ;
#33253 = LINE ( 'NONE', #36610, #29070 ) ;
#33254 = VERTEX_POINT ( 'NONE', #13678 ) ;
#33255 = FACE_OUTER_BOUND ( 'NONE', #7687, .T. ) ;
#33256 = CARTESIAN_POINT ( 'NONE',  ( 0.3862712429686727678, 1.188820645368945605, -3.333333333333333481 ) ) ;
#33257 = CARTESIAN_POINT ( 'NONE',  ( -1.249999999999999778, 0.000000000000000000, 10.00000000000000000 ) ) ;
#33258 = CARTESIAN_POINT ( 'NONE',  ( -14.99999999999937472, 17.00000000000000000, -54.99999999999999289 ) ) ;
#33259 = AXIS2_PLACEMENT_3D ( 'NONE', #23921, #7783, #12130 ) ;
#33260 = CARTESIAN_POINT ( 'NONE',  ( 356.0000000000000568, 165.0000000000000000, -90.00000000000018474 ) ) ;
#33261 = CARTESIAN_POINT ( 'NONE',  ( -205.6708471809678827, 1.750000000000010214, -118.1565861772249519 ) ) ;
#33262 = AXIS2_PLACEMENT_3D ( 'NONE', #42920, #49563, #15238 ) ;
#33263 = CARTESIAN_POINT ( 'NONE',  ( 0.4166666666666664631, 0.000000000000000000, 10.00000000000000000 ) ) ;
#33264 = DIRECTION ( 'NONE',  ( -0.000000000000000000, -0.000000000000000000, -1.000000000000000000 ) ) ;
#33265 = AXIS2_PLACEMENT_3D ( 'NONE', #1811, #17454, #36739 ) ;
#33266 = CARTESIAN_POINT ( 'NONE',  ( 29.61572577327002520, 16.11461842845735859, 8.807470649214879543 ) ) ;
#33267 = ORIENTED_EDGE ( 'NONE', *, *, #26643, .F. ) ;
#33268 = DIRECTION ( 'NONE',  ( -0.000000000000000000, -0.000000000000000000, -1.000000000000000000 ) ) ;
#33269 = VECTOR ( 'NONE', #26646, 1000.000000000000000 ) ;
#33270 = CARTESIAN_POINT ( 'NONE',  ( -88.44597344681497475, 0.000000000000000000, 165.0000000000000000 ) ) ;
#33271 = VECTOR ( 'NONE', #20032, 1000.000000000000000 ) ;
#33272 = DIRECTION ( 'NONE',  ( -0.000000000000000000, -0.000000000000000000, -1.000000000000000000 ) ) ;
#33273 = ADVANCED_FACE ( 'NONE', ( #6733 ), #6244, .T. ) ;
#33274 = DIRECTION ( 'NONE',  ( -1.000000000000000000, -0.000000000000000000, -0.000000000000000000 ) ) ;
#33275 = LINE ( 'NONE', #37127, #21729 ) ;
#33276 = ORIENTED_EDGE ( 'NONE', *, *, #18103, .T. ) ;
#33277 = FACE_OUTER_BOUND ( 'NONE', #22670, .T. ) ;
#33278 = ORIENTED_EDGE ( 'NONE', *, *, #8260, .F. ) ;
#33279 = AXIS2_PLACEMENT_3D ( 'NONE', #15815, #19910, #15566 ) ;
#33280 = DIRECTION ( 'NONE',  ( 0.000000000000000000, -1.000000000000000000, -3.186989995019654210E-49 ) ) ;
#33281 = VECTOR ( 'NONE', #10287, 1000.000000000000000 ) ;
#33282 = CARTESIAN_POINT ( 'NONE',  ( 113.3040265531850537, -1.749999999999997335, 120.8182875569279702 ) ) ;
#33283 = EDGE_LOOP ( 'NONE', ( #49815, #27689, #11346, #9562 ) ) ;
#33284 = LINE ( 'NONE', #22218, #34451 ) ;
#33285 = LINE ( 'NONE', #32529, #38880 ) ;
#33286 = ORIENTED_EDGE ( 'NONE', *, *, #6542, .T. ) ;
#33287 = EDGE_LOOP ( 'NONE', ( #14332, #5453, #41923, #47723 ) ) ;
#33288 = CARTESIAN_POINT ( 'NONE',  ( 80.00000000000061107, 16.00000000000000000, -54.99999999999999289 ) ) ;
#33289 = CARTESIAN_POINT ( 'NONE',  ( 0.1287570809895575430, 0.3962735484563150168, 10.00000000000000000 ) ) ;
#33290 = DIRECTION ( 'NONE',  ( 0.000000000000000000, 0.000000000000000000, 1.000000000000000000 ) ) ;
#33291 = VECTOR ( 'NONE', #22086, 1000.000000000000000 ) ;
#33292 = VERTEX_POINT ( 'NONE', #44705 ) ;
#33293 = PLANE ( 'NONE',  #32526 ) ;
#33294 = DIRECTION ( 'NONE',  ( -1.000000000000000000, -0.000000000000000000, -0.000000000000000000 ) ) ;
#33295 = VERTEX_POINT ( 'NONE', #21627 ) ;
#33296 = VECTOR ( 'NONE', #32089, 1000.000000000000000 ) ;
#33297 = ORIENTED_EDGE ( 'NONE', *, *, #30939, .T. ) ;
#33298 = ORIENTED_EDGE ( 'NONE', *, *, #19260, .F. ) ;
#33299 = CARTESIAN_POINT ( 'NONE',  ( 111.5540265531850679, 0.000000000000000000, 159.0682875569279702 ) ) ;
#33300 = DIRECTION ( 'NONE',  ( 0.000000000000000000, 0.000000000000000000, 1.000000000000000000 ) ) ;
#33301 = DIRECTION ( 'NONE',  ( 0.000000000000000000, 0.000000000000000000, -1.000000000000000000 ) ) ;
#33302 = ORIENTED_EDGE ( 'NONE', *, *, #38922, .F. ) ;
#33303 = ADVANCED_FACE ( 'NONE', ( #9582 ), #48791, .T. ) ;
#33304 = CARTESIAN_POINT ( 'NONE',  ( 115.0540265531850395, 2.143131898507847836E-16, -120.9317124430720156 ) ) ;
#33305 = LINE ( 'NONE', #48381, #196 ) ;
#33306 = CARTESIAN_POINT ( 'NONE',  ( -114.9999999999981526, 17.00000000000000000, 90.00000000000000000 ) ) ;
#33307 = DIRECTION ( 'NONE',  ( 0.000000000000000000, 0.000000000000000000, 1.000000000000000000 ) ) ;
#33308 = VECTOR ( 'NONE', #36981, 1000.000000000000000 ) ;
#33309 = SPHERICAL_SURFACE ( 'NONE', #23262, 0.5000000000000000000 ) ;
#33310 = DIRECTION ( 'NONE',  ( 0.000000000000000000, 1.000000000000000000, -1.604368532695312981E-16 ) ) ;
#33311 = CARTESIAN_POINT ( 'NONE',  ( 23.31729631074197329, 24.19776167542427814, -8.016098858316199838 ) ) ;
#33312 = LINE ( 'NONE', #25342, #49359 ) ;
#33313 = CARTESIAN_POINT ( 'NONE',  ( -9.260964247899874380, 13.84230907185616744, -9.683996418299976483 ) ) ;
#33314 = CARTESIAN_POINT ( 'NONE',  ( -10.28825587112213746, 13.03847615613166333, 3.266473740018926541 ) ) ;
#33315 = ORIENTED_EDGE ( 'NONE', *, *, #31574, .T. ) ;
#33316 = CARTESIAN_POINT ( 'NONE',  ( 350.0000000000000000, -174.9999999999999432, -350.0000000000001705 ) ) ;
#33317 = CARTESIAN_POINT ( 'NONE',  ( -28.96803024440907137, -18.11533787072017176, 7.455576670931136185 ) ) ;
#33318 = LINE ( 'NONE', #25350, #41005 ) ;
#33319 = EDGE_LOOP ( 'NONE', ( #5620, #45566, #24289, #38506, #28566, #2273 ) ) ;
#33320 = CARTESIAN_POINT ( 'NONE',  ( -88.44597344681497475, 0.000000000000000000, -120.9317124430720725 ) ) ;
#33321 = DIRECTION ( 'NONE',  ( 0.000000000000000000, 0.000000000000000000, 1.000000000000000000 ) ) ;
#33322 = AXIS2_PLACEMENT_3D ( 'NONE', #39170, #7096, #26844 ) ;
#33323 = ORIENTED_EDGE ( 'NONE', *, *, #27740, .T. ) ;
#33324 = CARTESIAN_POINT ( 'NONE',  ( 1.193089574352119264, 0.2545860991493882342, 9.963925895596188909 ) ) ;
#33325 = DIRECTION ( 'NONE',  ( -1.000000000000000000, 0.000000000000000000, -7.793956916774525800E-48 ) ) ;
#33326 = EDGE_CURVE ( 'NONE', #23001, #30787, #33696, .T. ) ;
#33327 = DIRECTION ( 'NONE',  ( 1.333906992743555050E-23, -1.000000000000000000, 0.000000000000000000 ) ) ;
#33328 = DIRECTION ( 'NONE',  ( -1.000000000000000000, 0.000000000000000000, 0.000000000000000000 ) ) ;
#33329 = ORIENTED_EDGE ( 'NONE', *, *, #2002, .F. ) ;
#33330 = FACE_OUTER_BOUND ( 'NONE', #50135, .T. ) ;
#33331 = VERTEX_POINT ( 'NONE', #40878 ) ;
#33332 = ORIENTED_EDGE ( 'NONE', *, *, #27057, .T. ) ;
#33333 = DIRECTION ( 'NONE',  ( -1.000000000000000000, -0.000000000000000000, -0.000000000000000000 ) ) ;
#33334 = ORIENTED_EDGE ( 'NONE', *, *, #8923, .T. ) ;
#33335 = FACE_OUTER_BOUND ( 'NONE', #22842, .T. ) ;
#33336 = CARTESIAN_POINT ( 'NONE',  ( -168.4459734468149747, 1.025126265847089213, 162.5682875569279133 ) ) ;
#33337 = EDGE_LOOP ( 'NONE', ( #39550, #46634, #12236, #7330 ) ) ;
#33338 = CARTESIAN_POINT ( 'NONE',  ( -128.4459734468149463, 1.025126265847081442, -160.9317124430720014 ) ) ;
#33339 = ADVANCED_FACE ( 'NONE', ( #18023 ), #44944, .T. ) ;
#33340 = CARTESIAN_POINT ( 'NONE',  ( 210.0000000000000568, 2.143131898507881856E-16, -80.93171244307202983 ) ) ;
#33341 = ADVANCED_FACE ( 'NONE', ( #6480 ), #1886, .T. ) ;
#33342 = DIRECTION ( 'NONE',  ( 1.000000000000000000, 0.000000000000000000, 7.793956916774525800E-48 ) ) ;
#33343 = ORIENTED_EDGE ( 'NONE', *, *, #30250, .F. ) ;
#33344 = VECTOR ( 'NONE', #16355, 1000.000000000000000 ) ;
#33345 = CARTESIAN_POINT ( 'NONE',  ( -0.6126904405382037622, -1.085824959725731231, 9.981352469109934233 ) ) ;
#33346 = ADVANCED_FACE ( 'NONE', ( #2141 ), #24479, .T. ) ;
#33347 = CARTESIAN_POINT ( 'NONE',  ( -14.99999999999845812, 17.00000000000000000, 35.00000000000000000 ) ) ;
#33348 = ORIENTED_EDGE ( 'NONE', *, *, #48711, .T. ) ;
#33349 = CARTESIAN_POINT ( 'NONE',  ( 111.5540265531850537, 2.143131898507880377E-16, -160.9317124430720298 ) ) ;
#33350 = ORIENTED_EDGE ( 'NONE', *, *, #3053, .F. ) ;
#33351 = VERTEX_POINT ( 'NONE', #26748 ) ;
#33352 = VERTEX_POINT ( 'NONE', #46454 ) ;
#33353 = DIRECTION ( 'NONE',  ( 0.000000000000000000, 0.000000000000000000, -1.000000000000000000 ) ) ;
#33354 = LINE ( 'NONE', #37223, #49567 ) ;
#33355 = ADVANCED_FACE ( 'NONE', ( #11608 ), #31000, .T. ) ;
#33356 = EDGE_LOOP ( 'NONE', ( #10065, #45105 ) ) ;
#33357 = EDGE_CURVE ( 'NONE', #13072, #14294, #39096, .T. ) ;
#33358 = DIRECTION ( 'NONE',  ( -1.000000000000000000, 0.000000000000000000, 0.000000000000000000 ) ) ;
#33359 = DIRECTION ( 'NONE',  ( 1.860490536778032451E-50, 0.000000000000000000, -1.000000000000000000 ) ) ;
#33360 = CYLINDRICAL_SURFACE ( 'NONE', #46005, 1.750000000000001554 ) ;
#33361 = EDGE_CURVE ( 'NONE', #28480, #4867, #18773, .T. ) ;
#33362 = EDGE_CURVE ( 'NONE', #18141, #24669, #23409, .T. ) ;
#33363 = DIRECTION ( 'NONE',  ( 0.000000000000000000, 0.000000000000000000, 1.000000000000000000 ) ) ;
#33364 = AXIS2_PLACEMENT_3D ( 'NONE', #28667, #36906, #44292 ) ;
#33365 = B_SPLINE_CURVE_WITH_KNOTS ( 'NONE', 3,
 ( #46026, #39151, #11428, #42460 ),
 .UNSPECIFIED., .F., .F.,
 ( 4, 4 ),
 ( 0.9890644561681869451, 1.000000000000000000 ),
 .UNSPECIFIED. ) ;
#33366 = EDGE_LOOP ( 'NONE', ( #9650, #91, #14600, #12667 ) ) ;
#33367 = DIRECTION ( 'NONE',  ( -1.000000000000000000, 0.000000000000000000, 0.000000000000000000 ) ) ;
#33368 = CARTESIAN_POINT ( 'NONE',  ( -0.6883547519190790220, 1.010122381805031333, 9.969517326150315384 ) ) ;
#33369 = ADVANCED_FACE ( 'NONE', ( #19029 ), #3898, .F. ) ;
#33370 = CARTESIAN_POINT ( 'NONE',  ( -16.02661358026017879, -4.530191650547607196, -9.683996418299976483 ) ) ;
#33371 = ORIENTED_EDGE ( 'NONE', *, *, #38426, .T. ) ;
#33372 = ITEM_DEFINED_TRANSFORMATION ( 'NONE', 'NONE', #1262,  #45486 ) ;
#33373 =( BOUNDED_CURVE ( )  B_SPLINE_CURVE ( 3, ( #42564, #35410, #47142, #19211 ),
 .UNSPECIFIED., .F., .F. ) 
 B_SPLINE_CURVE_WITH_KNOTS ( ( 4, 4 ),
 ( 4.712388980384689674, 6.283185307179586232 ),
 .UNSPECIFIED. ) 
 CURVE ( )  GEOMETRIC_REPRESENTATION_ITEM ( )  RATIONAL_B_SPLINE_CURVE ( ( 1.000000000000000000, 0.8047378541243649375, 0.8047378541243649375, 1.000000000000000000 ) ) 
 REPRESENTATION_ITEM ( '' )  );
#33374 = CARTESIAN_POINT ( 'NONE',  ( 7.398363427652525637, -15.19415887381133246, -9.008049429158100807 ) ) ;
#33375 = CARTESIAN_POINT ( 'NONE',  ( -0.1287570809895632329, 0.3962735484563137400, 10.00000000000000000 ) ) ;
#33376 = DIRECTION ( 'NONE',  ( -1.000000000000000000, -0.000000000000000000, -0.000000000000000000 ) ) ;
#33377 = ORIENTED_EDGE ( 'NONE', *, *, #25956, .F. ) ;
#33378 = DIRECTION ( 'NONE',  ( -0.000000000000000000, -0.000000000000000000, -1.000000000000000000 ) ) ;
#33379 = CARTESIAN_POINT ( 'NONE',  ( 181.0000000000000000, 165.0000000000000000, -358.0000000000001705 ) ) ;
#33380 =( BOUNDED_CURVE ( )  B_SPLINE_CURVE ( 3, ( #21817, #40310, #32614, #29007 ),
 .UNSPECIFIED., .F., .F. ) 
 B_SPLINE_CURVE_WITH_KNOTS ( ( 4, 4 ),
 ( 0.000000000000000000, 1.570796326794896558 ),
 .UNSPECIFIED. ) 
 CURVE ( )  GEOMETRIC_REPRESENTATION_ITEM ( )  RATIONAL_B_SPLINE_CURVE ( ( 1.000000000000000000, 0.8047378541243649375, 0.8047378541243649375, 1.000000000000000000 ) ) 
 REPRESENTATION_ITEM ( '' )  );
#33381 = FACE_OUTER_BOUND ( 'NONE', #31446, .T. ) ;
#33382 = CARTESIAN_POINT ( 'NONE',  ( -8.277096487746778308, 50.00000000000000711, 7.455576670931136185 ) ) ;
#33383 = EDGE_CURVE ( 'NONE', #48420, #21503, #10835, .T. ) ;
#33384 = CARTESIAN_POINT ( 'NONE',  ( 195.0540265531851105, 2.143131898507890731E-16, -165.0000000000000000 ) ) ;
#33385 = EDGE_LOOP ( 'NONE', ( #42532, #34220, #16819, #46054 ) ) ;
#33386 = EDGE_CURVE ( 'NONE', #39650, #21642, #34719, .T. ) ;
#33387 = FACE_OUTER_BOUND ( 'NONE', #6099, .T. ) ;
#33388 = ORIENTED_EDGE ( 'NONE', *, *, #5325, .F. ) ;
#33389 = EDGE_CURVE ( 'NONE', #23796, #4361, #42125, .T. ) ;
#33390 = CARTESIAN_POINT ( 'NONE',  ( -0.4166666666666664631, 0.000000000000000000, 10.00000000000000000 ) ) ;
#33391 = EDGE_LOOP ( 'NONE', ( #48099, #13556 ) ) ;
#33392 = B_SPLINE_CURVE_WITH_KNOTS ( 'NONE', 3,
 ( #30907, #27031, #11382, #7546, #19584, #19334 ),
 .UNSPECIFIED., .F., .F.,
 ( 4, 2, 4 ),
 ( 4.246530788431251365E-17, 0.009882509389272368938, 0.01976501877854469624 ),
 .UNSPECIFIED. ) ;
#33393 = DIRECTION ( 'NONE',  ( -1.000000000000000000, -0.000000000000000000, -0.000000000000000000 ) ) ;
#33394 = EDGE_CURVE ( 'NONE', #31274, #22541, #26992, .T. ) ;
#33395 = LINE ( 'NONE', #32375, #47829 ) ;
#33396 =( BOUNDED_CURVE ( )  B_SPLINE_CURVE ( 3, ( #1428, #24774, #40423, #5512 ),
 .UNSPECIFIED., .F., .F. ) 
 B_SPLINE_CURVE_WITH_KNOTS ( ( 4, 4 ),
 ( 1.570796326794889897, 3.141592653589793560 ),
 .UNSPECIFIED. ) 
 CURVE ( )  GEOMETRIC_REPRESENTATION_ITEM ( )  RATIONAL_B_SPLINE_CURVE ( ( 1.000000000000000000, 0.8047378541243632721, 0.8047378541243632721, 1.000000000000000000 ) ) 
 REPRESENTATION_ITEM ( '' )  );
#33397 = CARTESIAN_POINT ( 'NONE',  ( 130.0000000000015064, 17.00000000000000000, 35.00000000000000000 ) ) ;
#33398 = ORIENTED_EDGE ( 'NONE', *, *, #33668, .F. ) ;
#33399 = EDGE_CURVE ( 'NONE', #34606, #15667, #13870, .T. ) ;
#33400 = CARTESIAN_POINT ( 'NONE',  ( -126.6959734468149321, 0.000000000000000000, 165.0000000000000000 ) ) ;
#33401 = CIRCLE ( 'NONE', #4716, 1.750000000000015543 ) ;
#33402 = ORIENTED_EDGE ( 'NONE', *, *, #11424, .T. ) ;
#33403 = CARTESIAN_POINT ( 'NONE',  ( 0.000000000000000000, 181.0000000000000284, -356.0000000000002274 ) ) ;
#33404 = CARTESIAN_POINT ( 'NONE',  ( -46.69597344681494633, 0.000000000000000000, 165.0000000000000000 ) ) ;
#33405 = CARTESIAN_POINT ( 'NONE',  ( 340.0000000000000568, 181.0000000000000284, 341.9999999999997726 ) ) ;
#33406 = LINE ( 'NONE', #48976, #34095 ) ;
#33407 = CARTESIAN_POINT ( 'NONE',  ( 73.30402655318508209, 1.750000000000010214, -39.18171244307202983 ) ) ;
#33408 = ORIENTED_EDGE ( 'NONE', *, *, #23328, .T. ) ;
#33409 = EDGE_LOOP ( 'NONE', ( #28240, #1413, #34089, #27486 ) ) ;
#33410 = FACE_OUTER_BOUND ( 'NONE', #45775, .T. ) ;
#33411 = ORIENTED_EDGE ( 'NONE', *, *, #25960, .F. ) ;
#33412 = CARTESIAN_POINT ( 'NONE',  ( 135.0000000000019043, 16.00000000000000000, 65.00000000000000000 ) ) ;
#33413 = DIRECTION ( 'NONE',  ( 0.000000000000000000, 0.000000000000000000, -1.000000000000000000 ) ) ;
#33414 = EDGE_CURVE ( 'NONE', #28555, #20580, #27068, .T. ) ;
#33415 = ORIENTED_EDGE ( 'NONE', *, *, #22650, .T. ) ;
#33416 = CARTESIAN_POINT ( 'NONE',  ( 0.3501237319956588823, -1.209643720083640739, 9.974012008644017158 ) ) ;
#33417 = CARTESIAN_POINT ( 'NONE',  ( 210.0000000000000568, 0.000000000000000000, -119.1817124430720440 ) ) ;
#33418 = B_SPLINE_SURFACE_WITH_KNOTS ( 'NONE', 3, 3, ( 
 ( #40186, #20679, #18801, #42662 ),
 ( #30376, #34486, #3929, #3152 ),
 ( #30894, #35250, #19569, #46990 ),
 ( #4188, #93, #15475, #46480 ) ),
 .UNSPECIFIED., .F., .F., .F.,
 ( 4, 4 ),
 ( 4, 4 ),
 ( 0.000000000000000000, 1.000000000000000000 ),
 ( 0.000000000000000000, 1.000000000000000000 ),
 .UNSPECIFIED. ) ;
#33419 = ORIENTED_EDGE ( 'NONE', *, *, #9816, .F. ) ;
#33420 = ADVANCED_FACE ( 'NONE', ( #1946 ), #5535, .T. ) ;
#33421 = FACE_OUTER_BOUND ( 'NONE', #50646, .T. ) ;
#33422 = FACE_BOUND ( 'NONE', #19445, .T. ) ;
#33423 = CARTESIAN_POINT ( 'NONE',  ( 32.27890028733795447, -1.750000000000009548, -0.2068387089191121020 ) ) ;
#33424 = CARTESIAN_POINT ( 'NONE',  ( -1.317555876316872210, -0.4584864758884910074, 9.955131761384825140 ) ) ;
#33425 = EDGE_CURVE ( 'NONE', #39856, #20753, #31179, .T. ) ;
#33427 = ORIENTED_EDGE ( 'NONE', *, *, #2418, .T. ) ;
#33426 = EDGE_CURVE ( 'NONE', #38075, #28407, #49649, .T. ) ;
#33428 = ORIENTED_EDGE ( 'NONE', *, *, #13718, .T. ) ;
#33429 = ADVANCED_FACE ( 'NONE', ( #25799 ), #21430, .F. ) ;
#33430 = DIRECTION ( 'NONE',  ( 0.000000000000000000, 0.000000000000000000, 1.000000000000000000 ) ) ;
#33431 = CARTESIAN_POINT ( 'NONE',  ( -127.7210997126620242, -1.749999999999996669, -0.2068387089191042749 ) ) ;
#33432 = EDGE_CURVE ( 'NONE', #47246, #8581, #32745, .T. ) ;
#33433 = CARTESIAN_POINT ( 'NONE',  ( 129.9999999999999432, 16.00000000000000000, -114.9999999999999858 ) ) ;
#33434 = ORIENTED_EDGE ( 'NONE', *, *, #35748, .T. ) ;
#33435 = CARTESIAN_POINT ( 'NONE',  ( -5.000000000000000000, 175.0000000000000284, -353.7500000000001705 ) ) ;
#33436 = ORIENTED_EDGE ( 'NONE', *, *, #18808, .T. ) ;
#33437 = CARTESIAN_POINT ( 'NONE',  ( 73.30402655318508209, -1.750000000000009992, -159.1817124430720298 ) ) ;
#33438 = DIRECTION ( 'NONE',  ( 0.000000000000000000, 0.000000000000000000, 1.000000000000000000 ) ) ;
#33439 = DIRECTION ( 'NONE',  ( 1.000000000000000000, 0.000000000000000000, 0.000000000000000000 ) ) ;
#33440 = VECTOR ( 'NONE', #21880, 1000.000000000000000 ) ;
#33441 = CARTESIAN_POINT ( 'NONE',  ( 210.0000000000000568, 0.000000000000000000, 122.5682875569279844 ) ) ;
#33442 = LINE ( 'NONE', #48779, #31538 ) ;
#33443 = CARTESIAN_POINT ( 'NONE',  ( 31.55402655318503236, 1.025126265847089435, 82.56828755692798438 ) ) ;
#33444 = ORIENTED_EDGE ( 'NONE', *, *, #4979, .T. ) ;
#33445 = CARTESIAN_POINT ( 'NONE',  ( 1.080000014128428498, 0.7606467978644730898, 9.943883492372853183 ) ) ;
#33446 = FACE_BOUND ( 'NONE', #11640, .T. ) ;
#33447 = CARTESIAN_POINT ( 'NONE',  ( -0.1471466405331013361, -1.496299042407428503, 9.944962737616616977 ) ) ;
#33448 = CARTESIAN_POINT ( 'NONE',  ( 130.0000000000002842, 16.00000000000000000, -84.99999999999998579 ) ) ;
#33449 = ORIENTED_EDGE ( 'NONE', *, *, #7722, .T. ) ;
#33450 = EDGE_CURVE ( 'NONE', #32627, #31779, #45009, .T. ) ;
#33451 = CARTESIAN_POINT ( 'NONE',  ( -9.221081804193374865, -13.81382350053984176, 3.266473740018926541 ) ) ;
#33452 = ORIENTED_EDGE ( 'NONE', *, *, #4252, .T. ) ;
#33453 = DIRECTION ( 'NONE',  ( -0.000000000000000000, -0.000000000000000000, -1.000000000000000000 ) ) ;
#33454 = LINE ( 'NONE', #17534, #28278 ) ;
#33455 = CARTESIAN_POINT ( 'NONE',  ( 177.5000000000000284, -112.5000000000000000, -10.00000000000000000 ) ) ;
#33456 = LINE ( 'NONE', #13684, #31157 ) ;
#33457 = ORIENTED_EDGE ( 'NONE', *, *, #32367, .F. ) ;
#33458 = CARTESIAN_POINT ( 'NONE',  ( 30.22736451279166658, 39.84193304692632154, -2.408242355805840784 ) ) ;
#33459 = FACE_OUTER_BOUND ( 'NONE', #15029, .T. ) ;
#33460 = DIRECTION ( 'NONE',  ( -0.000000000000000000, -0.000000000000000000, -1.000000000000000000 ) ) ;
#33461 = EDGE_CURVE ( 'NONE', #39326, #35676, #49097, .T. ) ;
#33462 = VERTEX_POINT ( 'NONE', #48847 ) ;
#33463 = VERTEX_POINT ( 'NONE', #33507 ) ;
#33464 = PLANE ( 'NONE',  #34935 ) ;
#33465 = LINE ( 'NONE', #13934, #9098 ) ;
#33466 = VECTOR ( 'NONE', #36791, 1000.000000000000000 ) ;
#33467 = ORIENTED_EDGE ( 'NONE', *, *, #27182, .T. ) ;
#33468 = ORIENTED_EDGE ( 'NONE', *, *, #27060, .T. ) ;
#33469 = CARTESIAN_POINT ( 'NONE',  ( 73.30402655318508209, -1.750000000000009992, 0.8182875569279768335 ) ) ;
#33470 = CARTESIAN_POINT ( 'NONE',  ( -84.94597344681493212, 1.025126265847089879, -77.43171244307200141 ) ) ;
#33471 = CARTESIAN_POINT ( 'NONE',  ( -49.75871208702130133, -40.58472229863598102, 5.000000000000000000 ) ) ;
#33472 = DIRECTION ( 'NONE',  ( 0.000000000000000000, 0.000000000000000000, 1.000000000000000000 ) ) ;
#33473 = EDGE_CURVE ( 'NONE', #35501, #12321, #9620, .T. ) ;
#33474 = VERTEX_POINT ( 'NONE', #13980 ) ;
#33475 = ORIENTED_EDGE ( 'NONE', *, *, #3828, .F. ) ;
#33476 = DIRECTION ( 'NONE',  ( 0.000000000000000000, 0.000000000000000000, 1.000000000000000000 ) ) ;
#33477 = DIRECTION ( 'NONE',  ( 1.654361225106055350E-24, 1.654361225106055350E-24, -1.000000000000000000 ) ) ;
#33478 = EDGE_CURVE ( 'NONE', #44104, #10041, #44236, .T. ) ;
#33479 = EDGE_CURVE ( 'NONE', #14675, #45829, #9391, .T. ) ;
#33480 = ORIENTED_EDGE ( 'NONE', *, *, #48132, .T. ) ;
#33481 = ORIENTED_EDGE ( 'NONE', *, *, #30207, .T. ) ;
#33482 = CARTESIAN_POINT ( 'NONE',  ( -1.104213410210672430, -0.6509177773818179968, 9.976582533991678048 ) ) ;
#33483 = DIRECTION ( 'NONE',  ( -0.000000000000000000, -0.000000000000000000, 1.000000000000000000 ) ) ;
#33484 = ADVANCED_FACE ( 'NONE', ( #9390 ), #1695, .T. ) ;
#33485 = EDGE_LOOP ( 'NONE', ( #47047, #5196, #35585, #49973 ) ) ;
#33486 = ORIENTED_EDGE ( 'NONE', *, *, #2358, .T. ) ;
#33487 = EDGE_CURVE ( 'NONE', #24426, #9029, #43403, .T. ) ;
#33488 = CARTESIAN_POINT ( 'NONE',  ( 349.9999999999999432, -168.9999999999999432, 355.9999999999997726 ) ) ;
#33489 = LINE ( 'NONE', #32991, #44405 ) ;
#33490 = ORIENTED_EDGE ( 'NONE', *, *, #2380, .F. ) ;
#33491 = EDGE_CURVE ( 'NONE', #11298, #1975, #5719, .T. ) ;
#33492 = PLANE ( 'NONE',  #16849 ) ;
#33493 = DIRECTION ( 'NONE',  ( 0.000000000000000000, 0.000000000000000000, 1.000000000000000000 ) ) ;
#33494 = DIRECTION ( 'NONE',  ( -0.000000000000000000, -0.000000000000000000, -1.000000000000000000 ) ) ;
#33495 = LINE ( 'NONE', #5774, #50655 ) ;
#33496 = LINE ( 'NONE', #49085, #40531 ) ;
#33497 = B_SPLINE_CURVE_WITH_KNOTS ( 'NONE', 3,
 ( #48229, #9771, #2091, #25434 ),
 .UNSPECIFIED., .F., .F.,
 ( 4, 4 ),
 ( 0.0003760194760237283622, 0.0006307719036365527603 ),
 .UNSPECIFIED. ) ;
#33498 = ORIENTED_EDGE ( 'NONE', *, *, #2626, .F. ) ;
#33499 = DIRECTION ( 'NONE',  ( -1.000000000000000000, 0.000000000000000000, 0.000000000000000000 ) ) ;
#33500 = DIRECTION ( 'NONE',  ( -0.000000000000000000, -0.000000000000000000, 1.000000000000000000 ) ) ;
#33501 = ADVANCED_FACE ( 'NONE', ( #17085 ), #13228, .T. ) ;
#33502 = DIRECTION ( 'NONE',  ( -1.000000000000000000, 0.000000000000000000, 0.000000000000000000 ) ) ;
#33503 = CYLINDRICAL_SURFACE ( 'NONE', #46323, 4.000000000000003553 ) ;
#33504 = LINE ( 'NONE', #25795, #30599 ) ;
#33505 = DIRECTION ( 'NONE',  ( -1.000000000000000000, -0.000000000000000000, -0.000000000000000000 ) ) ;
#33506 = DIRECTION ( 'NONE',  ( 0.000000000000000000, -1.000000000000000000, 3.469446951953611033E-15 ) ) ;
#33507 = CARTESIAN_POINT ( 'NONE',  ( 181.0000000000000000, -272.5000000000000000, -114.9999999999999147 ) ) ;
#33508 = ORIENTED_EDGE ( 'NONE', *, *, #50350, .T. ) ;
#33509 = CARTESIAN_POINT ( 'NONE',  ( 31.44259251615245887, 38.95901822126169378, -9.367992836599951190 ) ) ;
#33510 = CARTESIAN_POINT ( 'NONE',  ( -64.99999999999783995, 17.00000000000000000, 95.00000000000000000 ) ) ;
#33511 = CARTESIAN_POINT ( 'NONE',  ( 164.9999999999999716, 16.00000000000000000, 30.00000000000000000 ) ) ;
#33512 = FACE_OUTER_BOUND ( 'NONE', #19885, .T. ) ;
#33513 = CARTESIAN_POINT ( 'NONE',  ( -22.82242230425432439, 2.683863964738837371, 230.0000000000000000 ) ) ;
#33514 = ORIENTED_EDGE ( 'NONE', *, *, #17194, .F. ) ;
#33515 = B_SPLINE_SURFACE_WITH_KNOTS ( 'NONE', 3, 3, ( 
 ( #48706, #44135, #13346, #24912 ),
 ( #32877, #13097, #40558, #2304 ),
 ( #21552, #37242, #48459, #44381 ),
 ( #17212, #21303, #17939, #29258 ) ),
 .UNSPECIFIED., .F., .F., .F.,
 ( 4, 4 ),
 ( 4, 4 ),
 ( 0.000000000000000000, 1.000000000000000000 ),
 ( 0.000000000000000000, 1.000000000000000000 ),
 .UNSPECIFIED. ) ;
#33516 = EDGE_LOOP ( 'NONE', ( #25982, #42365, #32141, #3397, #10244, #27241 ) ) ;
#33517 = CARTESIAN_POINT ( 'NONE',  ( 164.9999999999999716, -268.4999999999999432, -349.9999999999999432 ) ) ;
#33518 = EDGE_CURVE ( 'NONE', #36323, #12663, #44768, .T. ) ;
#33519 = ORIENTED_EDGE ( 'NONE', *, *, #28938, .T. ) ;
#33520 = CARTESIAN_POINT ( 'NONE',  ( 1.011271242968683648, 0.7347315653655930312, 10.00000000000000000 ) ) ;
#33521 = CARTESIAN_POINT ( 'NONE',  ( 341.9999999999999432, 182.1715728752539007, -357.1715728752538439 ) ) ;
#33522 = ORIENTED_EDGE ( 'NONE', *, *, #16404, .T. ) ;
#33523 = ORIENTED_EDGE ( 'NONE', *, *, #11111, .T. ) ;
#33524 = ORIENTED_EDGE ( 'NONE', *, *, #16558, .F. ) ;
#33525 =( BOUNDED_CURVE ( )  B_SPLINE_CURVE ( 3, ( #24804, #19930, #44026, #43278 ),
 .UNSPECIFIED., .F., .F. ) 
 B_SPLINE_CURVE_WITH_KNOTS ( ( 4, 4 ),
 ( 1.570796326794896558, 3.141592653589793116 ),
 .UNSPECIFIED. ) 
 CURVE ( )  GEOMETRIC_REPRESENTATION_ITEM ( )  RATIONAL_B_SPLINE_CURVE ( ( 1.000000000000000000, 0.8047378541243649375, 0.8047378541243649375, 1.000000000000000000 ) ) 
 REPRESENTATION_ITEM ( '' )  );
#33526 = CARTESIAN_POINT ( 'NONE',  ( -0.3910393408547386818, -3.877122853643371947, 9.741991644047244492 ) ) ;
#33527 = CARTESIAN_POINT ( 'NONE',  ( 37.09503908879513290, -5.733418411338704779, 4.835783797351805191 ) ) ;
#33528 = AXIS2_PLACEMENT_3D ( 'NONE', #19151, #23534, #50152 ) ;
#33529 = DIRECTION ( 'NONE',  ( 0.000000000000000000, 0.000000000000000000, 1.000000000000000000 ) ) ;
#33530 = EDGE_LOOP ( 'NONE', ( #3131, #29040, #38899, #44238 ) ) ;
#33531 = ADVANCED_FACE ( 'NONE', ( #30405 ), #7307, .T. ) ;
#33532 = VECTOR ( 'NONE', #19281, 1000.000000000000000 ) ;
#33533 = CARTESIAN_POINT ( 'NONE',  ( -210.0000000000000568, 0.000000000000000000, 2.568287556927987048 ) ) ;
#33534 = EDGE_CURVE ( 'NONE', #10975, #12244, #40963, .T. ) ;
#33535 = FACE_OUTER_BOUND ( 'NONE', #8100, .T. ) ;
#33536 = PRESENTATION_STYLE_ASSIGNMENT (( #26839 ) ) ;
#33537 = ORIENTED_EDGE ( 'NONE', *, *, #42841, .F. ) ;
#33538 = VERTEX_POINT ( 'NONE', #34787 ) ;
#33539 = CARTESIAN_POINT ( 'NONE',  ( -88.44597344681497475, 0.000000000000000000, -157.4317124430720014 ) ) ;
#33540 = VECTOR ( 'NONE', #20293, 1000.000000000000000 ) ;
#33541 = CIRCLE ( 'NONE', #14663, 4.000000000000003553 ) ;
#33542 = VECTOR ( 'NONE', #29447, 1000.000000000000000 ) ;
#33543 = CYLINDRICAL_SURFACE ( 'NONE', #10357, 1.750000000000008438 ) ;
#33544 = DIRECTION ( 'NONE',  ( -1.000000000000000000, -0.000000000000000000, -0.000000000000000000 ) ) ;
#33545 = B_SPLINE_CURVE_WITH_KNOTS ( 'NONE', 3,
 ( #35152, #4082, #3307, #19978 ),
 .UNSPECIFIED., .F., .F.,
 ( 4, 4 ),
 ( 0.0001535465953327018473, 0.0005837444810856221586 ),
 .UNSPECIFIED. ) ;
#33546 = ORIENTED_EDGE ( 'NONE', *, *, #37488, .T. ) ;
#33547 = EDGE_CURVE ( 'NONE', #30823, #4890, #15273, .T. ) ;
#33548 = CARTESIAN_POINT ( 'NONE',  ( -6.695973446814940111, -1.750000000000023759, -39.18171244307202983 ) ) ;
#33549 = CARTESIAN_POINT ( 'NONE',  ( -208.4459734468149463, 0.000000000000000000, 39.06828755692798438 ) ) ;
#33550 = EDGE_CURVE ( 'NONE', #47536, #25574, #50358, .T. ) ;
#33551 = VECTOR ( 'NONE', #8029, 1000.000000000000000 ) ;
#33552 = CYLINDRICAL_SURFACE ( 'NONE', #39148, 1.750000000000008438 ) ;
#33553 = CARTESIAN_POINT ( 'NONE',  ( -44.94597344681493922, -1.025126265847089213, -160.9317124430720014 ) ) ;
#33554 = CARTESIAN_POINT ( 'NONE',  ( -45.67084718096785423, -1.750000000000009326, 159.7931612910809065 ) ) ;
#33556 = ADVANCED_FACE ( 'NONE', ( #41443 ), #26053, .T. ) ;
#33555 = DIRECTION ( 'NONE',  ( 0.000000000000000000, -0.000000000000000000, -1.000000000000000000 ) ) ;
#33557 = CARTESIAN_POINT ( 'NONE',  ( 27.31081730472575941, 41.96092862852144378, 3.199614146704519602 ) ) ;
#33558 = CARTESIAN_POINT ( 'NONE',  ( 0.8808108730164768696, 0.8497440890325094198, 9.966990753364711964 ) ) ;
#33559 = CARTESIAN_POINT ( 'NONE',  ( -36.76598589393961447, -7.383243274241610088, -8.192531242611266862 ) ) ;
#33560 = CARTESIAN_POINT ( 'NONE',  ( -1.011271242968683426, -0.7347315653655928092, -10.00000000000000000 ) ) ;
#33561 = CARTESIAN_POINT ( 'NONE',  ( -28.55116071645519327, 41.05976639056880373, -2.408242355805840784 ) ) ;
#33562 = ORIENTED_EDGE ( 'NONE', *, *, #47793, .F. ) ;
#33563 = LINE ( 'NONE', #40754, #33542 ) ;
#33564 = CARTESIAN_POINT ( 'NONE',  ( 0.1287570809895630941, -0.3962735484563133515, 10.00000000000000000 ) ) ;
#33565 = CARTESIAN_POINT ( 'NONE',  ( -0.5000000000000000000, 0.5000000000000000000, 1000.000000000000000 ) ) ;
#33566 = AXIS2_PLACEMENT_3D ( 'NONE', #40256, #4834, #32316 ) ;
#33567 = ORIENTED_EDGE ( 'NONE', *, *, #24918, .T. ) ;
#33568 = LINE ( 'NONE', #21005, #1916 ) ;
#33569 = VECTOR ( 'NONE', #24484, 1000.000000000000000 ) ;
#33570 = CARTESIAN_POINT ( 'NONE',  ( -1.780619886013952602, -1.041246721325602920, 9.886433018048069954 ) ) ;
#33571 = VERTEX_POINT ( 'NONE', #19093 ) ;
#33572 = DIRECTION ( 'NONE',  ( -0.000000000000000000, -0.000000000000000000, 1.000000000000000000 ) ) ;
#33573 = DIRECTION ( 'NONE',  ( 0.000000000000000000, 1.000000000000000000, -1.604368532695312981E-16 ) ) ;
#33574 = FACE_OUTER_BOUND ( 'NONE', #41304, .T. ) ;
#33575 = AXIS2_PLACEMENT_3D ( 'NONE', #29045, #32912, #44663 ) ;
#33576 = DIRECTION ( 'NONE',  ( 0.000000000000000000, 2.537652627714642000E-15, 1.000000000000000000 ) ) ;
#33577 = EDGE_LOOP ( 'NONE', ( #13239, #5494, #22642, #50310 ) ) ;
#33578 = CARTESIAN_POINT ( 'NONE',  ( -14.99999999999782041, 17.00000000000000000, 95.00000000000000000 ) ) ;
#33579 = ORIENTED_EDGE ( 'NONE', *, *, #48951, .F. ) ;
#33580 = ORIENTED_EDGE ( 'NONE', *, *, #38861, .T. ) ;
#33581 = ADVANCED_FACE ( 'NONE', ( #14750, #2932 ), #37619, .F. ) ;
#33582 = CARTESIAN_POINT ( 'NONE',  ( 350.0000000000000000, -168.9999999999999432, -344.0000000000001705 ) ) ;
#33583 = AXIS2_PLACEMENT_3D ( 'NONE', #13184, #29097, #1402 ) ;
#33584 = ORIENTED_EDGE ( 'NONE', *, *, #36847, .T. ) ;
#33585 = CARTESIAN_POINT ( 'NONE',  ( -167.7210997126620384, 1.750000000000009548, 41.84341382277508359 ) ) ;
#33586 = DIRECTION ( 'NONE',  ( -1.000000000000000000, -0.000000000000000000, -0.000000000000000000 ) ) ;
#33587 = ORIENTED_EDGE ( 'NONE', *, *, #39388, .F. ) ;
#33588 = CARTESIAN_POINT ( 'NONE',  ( -0.3656201545664206076, 2.182515578491385000, 9.881002359080270026 ) ) ;
#33589 = B_SPLINE_CURVE_WITH_KNOTS ( 'NONE', 3,
 ( #16159, #31818, #47403, #32063 ),
 .UNSPECIFIED., .F., .F.,
 ( 4, 4 ),
 ( 0.0004299334430849446756, 0.0007706806524480028925 ),
 .UNSPECIFIED. ) ;
#33590 = FACE_OUTER_BOUND ( 'NONE', #45394, .T. ) ;
#33591 = CARTESIAN_POINT ( 'NONE',  ( 344.0000000000000000, 167.0000000000000000, -342.0000000000001137 ) ) ;
#33592 = ORIENTED_EDGE ( 'NONE', *, *, #17825, .F. ) ;
#33593 = FACE_OUTER_BOUND ( 'NONE', #44354, .T. ) ;
#33594 = CARTESIAN_POINT ( 'NONE',  ( -5.647304616913629616, 2.688010569040066411, 742.8425600500171413 ) ) ;
#33595 = PLANE ( 'NONE',  #28346 ) ;
#33596 = ORIENTED_EDGE ( 'NONE', *, *, #17538, .T. ) ;
#33597 = CARTESIAN_POINT ( 'NONE',  ( 166.9999999999999716, 165.0000000000000000, -344.0000000000001137 ) ) ;
#33598 = CARTESIAN_POINT ( 'NONE',  ( 339.9999999999999432, 166.6568542494923406, -341.6568542494925396 ) ) ;
#33599 = ORIENTED_EDGE ( 'NONE', *, *, #6428, .F. ) ;
#33600 = ORIENTED_EDGE ( 'NONE', *, *, #43491, .F. ) ;
#33601 = ORIENTED_EDGE ( 'NONE', *, *, #29265, .F. ) ;
#33602 = CARTESIAN_POINT ( 'NONE',  ( -4.207128120815918256E-14, 3.058192377181588826E-14, 10.00000000000000000 ) ) ;
#33603 = CARTESIAN_POINT ( 'NONE',  ( 28.52604530808654815, 41.07801380285680892, -3.760136334089591248 ) ) ;
#33604 = ORIENTED_EDGE ( 'NONE', *, *, #15004, .T. ) ;
#33605 = VECTOR ( 'NONE', #37636, 1000.000000000000000 ) ;
#33606 = AXIS2_PLACEMENT_3D ( 'NONE', #37745, #17724, #14109 ) ;
#33607 = CARTESIAN_POINT ( 'NONE',  ( -208.4459734468149463, 0.000000000000000000, 82.56828755692798438 ) ) ;
#33608 = CARTESIAN_POINT ( 'NONE',  ( 0.000000000000000000, -175.0000000000000000, 10.00000000000000000 ) ) ;
#33609 = FACE_BOUND ( 'NONE', #24882, .T. ) ;
#33610 = VECTOR ( 'NONE', #32683, 1000.000000000000000 ) ;
#33611 = CARTESIAN_POINT ( 'NONE',  ( 194.3291528190321742, -1.750000000000009326, 1.843413822775066269 ) ) ;
#33612 = VERTEX_POINT ( 'NONE', #46013 ) ;
#33613 =( BOUNDED_CURVE ( )  B_SPLINE_CURVE ( 3, ( #47233, #588, #9031, #28023 ),
 .UNSPECIFIED., .F., .F. ) 
 B_SPLINE_CURVE_WITH_KNOTS ( ( 4, 4 ),
 ( 1.570796326794896558, 3.141592653589793116 ),
 .UNSPECIFIED. ) 
 CURVE ( )  GEOMETRIC_REPRESENTATION_ITEM ( )  RATIONAL_B_SPLINE_CURVE ( ( 1.000000000000000000, 0.8047378541243649375, 0.8047378541243649375, 1.000000000000000000 ) ) 
 REPRESENTATION_ITEM ( '' )  );
#33614 = FACE_OUTER_BOUND ( 'NONE', #16467, .T. ) ;
#33616 = EDGE_CURVE ( 'NONE', #19710, #34629, #41950, .T. ) ;
#33615 = LINE ( 'NONE', #2297, #24298 ) ;
#33617 = AXIS2_PLACEMENT_3D ( 'NONE', #18368, #45796, #1978 ) ;
#33618 = AXIS2_PLACEMENT_3D ( 'NONE', #47629, #31788, #5064 ) ;
#33619 = CYLINDRICAL_SURFACE ( 'NONE', #29742, 1.750000000000008438 ) ;
#33620 = ORIENTED_EDGE ( 'NONE', *, *, #48365, .T. ) ;
#33621 = CONTEXT_DEPENDENT_SHAPE_REPRESENTATION ( #23350, #42960 ) ;
#33623 = CARTESIAN_POINT ( 'NONE',  ( -19.99999999999971223, 17.00000000000000000, -60.00000000000000000 ) ) ;
#33622 = AXIS2_PLACEMENT_3D ( 'NONE', #45205, #41397, #6257 ) ;
#33624 = CARTESIAN_POINT ( 'NONE',  ( -126.6959734468149321, 1.749999999999997335, 120.8182875569279702 ) ) ;
#33625 = CARTESIAN_POINT ( 'NONE',  ( -14.99999999999812594, 17.00000000000000000, 65.00000000000000000 ) ) ;
#33626 = DIRECTION ( 'NONE',  ( 0.000000000000000000, 0.000000000000000000, -1.000000000000000000 ) ) ;
#33627 = VERTEX_POINT ( 'NONE', #46264 ) ;
#33628 = DIRECTION ( 'NONE',  ( -1.000000000000000000, 0.000000000000000000, 0.000000000000000000 ) ) ;
#33629 = CARTESIAN_POINT ( 'NONE',  ( 22.69295089195473736, 45.31600496604706052, 7.455576670931136185 ) ) ;
#33630 = CARTESIAN_POINT ( 'NONE',  ( 0.3862712429686894766, -1.188820645368940276, 3.333333333333333481 ) ) ;
#33631 = CARTESIAN_POINT ( 'NONE',  ( -0.4166666666666664631, 0.000000000000000000, 10.00000000000000000 ) ) ;
#33632 = DIRECTION ( 'NONE',  ( -0.000000000000000000, -1.000000000000000000, -0.000000000000000000 ) ) ;
#33633 = ORIENTED_EDGE ( 'NONE', *, *, #36299, .F. ) ;
#33634 = CARTESIAN_POINT ( 'NONE',  ( -14.49999999999999822, 12.98684210526315930, 19.37312575500900280 ) ) ;
#33635 = ORIENTED_EDGE ( 'NONE', *, *, #37933, .F. ) ;
#33636 = FACE_OUTER_BOUND ( 'NONE', #19954, .T. ) ;
#33637 = ORIENTED_EDGE ( 'NONE', *, *, #41222, .T. ) ;
#33638 = CARTESIAN_POINT ( 'NONE',  ( 164.9999999999999716, 17.00000000000000000, 4.999999999999990230 ) ) ;
#33639 = DIRECTION ( 'NONE',  ( 3.469446951953611231E-16, -0.000000000000000000, -1.000000000000000000 ) ) ;
#33640 = VERTEX_POINT ( 'NONE', #11166 ) ;
#33641 = AXIS2_PLACEMENT_3D ( 'NONE', #47540, #39636, #4233 ) ;
#33642 = VECTOR ( 'NONE', #12294, 1000.000000000000000 ) ;
#33643 = ORIENTED_EDGE ( 'NONE', *, *, #11230, .F. ) ;
#33644 = CARTESIAN_POINT ( 'NONE',  ( 135.0000000000006253, 17.00000000000000000, -54.99999999999999289 ) ) ;
#33645 = DIRECTION ( 'NONE',  ( 0.000000000000000000, 0.000000000000000000, 1.000000000000000000 ) ) ;
#33646 = DIRECTION ( 'NONE',  ( 0.000000000000000000, 0.000000000000000000, 1.000000000000000000 ) ) ;
#33647 = CARTESIAN_POINT ( 'NONE',  ( 75.05402655318509630, 2.143131898507880377E-16, 159.0682875569279702 ) ) ;
#33648 = VECTOR ( 'NONE', #35328, 1000.000000000000000 ) ;
#33649 = LINE ( 'NONE', #49238, #16733 ) ;
#33650 = EDGE_LOOP ( 'NONE', ( #23695, #2345, #36189, #7698 ) ) ;
#33651 = AXIS2_PLACEMENT_3D ( 'NONE', #35736, #6169, #45132 ) ;
#33652 = VERTEX_POINT ( 'NONE', #3444 ) ;
#33653 = CARTESIAN_POINT ( 'NONE',  ( 0.2099955233291934398, 1.205406147626143509, 9.993783931180535873 ) ) ;
#33654 = EDGE_LOOP ( 'NONE', ( #7153, #5813, #5912, #17703 ) ) ;
#33655 = LINE ( 'NONE', #28794, #31690 ) ;
#33656 = CARTESIAN_POINT ( 'NONE',  ( 358.0000000000000000, -182.1715728752539007, -357.1715728752540713 ) ) ;
#33657 = ORIENTED_EDGE ( 'NONE', *, *, #42173, .T. ) ;
#33658 = DIRECTION ( 'NONE',  ( 1.000000000000000000, 0.000000000000000000, -0.000000000000000000 ) ) ;
#33659 = CARTESIAN_POINT ( 'NONE',  ( -10.50000000000003375, 8.875661936878628921, -18.94832733001756253 ) ) ;
#33660 = ORIENTED_EDGE ( 'NONE', *, *, #26362, .T. ) ;
#33661 = CARTESIAN_POINT ( 'NONE',  ( 4.763548243873389154, -16.57409059453848599, 8.727788335465566760 ) ) ;
#33662 = CARTESIAN_POINT ( 'NONE',  ( -168.4459734468149463, 0.000000000000000000, -120.9317124430720156 ) ) ;
#33663 = CARTESIAN_POINT ( 'NONE',  ( 210.0000000000000568, 0.000000000000000000, -79.18171244307201562 ) ) ;
#33664 = CARTESIAN_POINT ( 'NONE',  ( -128.4459734468149179, 0.000000000000000000, 159.0682875569279986 ) ) ;
#33665 =( BOUNDED_CURVE ( )  B_SPLINE_CURVE ( 3, ( #31220, #4761, #7609, #667 ),
 .UNSPECIFIED., .F., .F. ) 
 B_SPLINE_CURVE_WITH_KNOTS ( ( 4, 4 ),
 ( 0.000000000000000000, 1.570796326794896558 ),
 .UNSPECIFIED. ) 
 CURVE ( )  GEOMETRIC_REPRESENTATION_ITEM ( )  RATIONAL_B_SPLINE_CURVE ( ( 1.000000000000000000, 0.8047378541243649375, 0.8047378541243649375, 1.000000000000000000 ) ) 
 REPRESENTATION_ITEM ( '' )  );
#33666 = DIRECTION ( 'NONE',  ( 0.000000000000000000, 0.9749645535258947282, 0.2223603367690671906 ) ) ;
#33667 = ORIENTED_EDGE ( 'NONE', *, *, #11444, .T. ) ;
#33668 = EDGE_CURVE ( 'NONE', #6629, #38277, #29897, .T. ) ;
#33669 = ORIENTED_EDGE ( 'NONE', *, *, #4979, .F. ) ;
#33670 = ORIENTED_EDGE ( 'NONE', *, *, #42192, .F. ) ;
#33672 = EDGE_CURVE ( 'NONE', #48660, #12455, #26813, .T. ) ;
#33671 = CARTESIAN_POINT ( 'NONE',  ( 8.176860274785711979, -5.756644512789521606, 9.282506307616484875 ) ) ;
#33673 =( BOUNDED_CURVE ( )  B_SPLINE_CURVE ( 3, ( #13039, #33070, #13289, #1267 ),
 .UNSPECIFIED., .F., .F. ) 
 B_SPLINE_CURVE_WITH_KNOTS ( ( 4, 4 ),
 ( 0.000000000000000000, 1.570796326794896558 ),
 .UNSPECIFIED. ) 
 CURVE ( )  GEOMETRIC_REPRESENTATION_ITEM ( )  RATIONAL_B_SPLINE_CURVE ( ( 1.000000000000000000, 0.8047378541243649375, 0.8047378541243649375, 1.000000000000000000 ) ) 
 REPRESENTATION_ITEM ( '' )  );
#33674 = LINE ( 'NONE', #37040, #42937 ) ;
#33675 = DIRECTION ( 'NONE',  ( -0.000000000000000000, -1.000000000000000000, -0.000000000000000000 ) ) ;
#33676 = ORIENTED_EDGE ( 'NONE', *, *, #24401, .T. ) ;
#33677 = EDGE_CURVE ( 'NONE', #34075, #38020, #2494, .T. ) ;
#33678 = DIRECTION ( 'NONE',  ( -1.000000000000000000, 0.000000000000000000, 0.000000000000000000 ) ) ;
#33680 = ORIENTED_EDGE ( 'NONE', *, *, #45087, .T. ) ;
#33679 = VECTOR ( 'NONE', #5605, 1000.000000000000000 ) ;
#33681 =( NAMED_UNIT ( * ) PLANE_ANGLE_UNIT ( ) SI_UNIT ( $, .RADIAN. ) );
#33682 = ADVANCED_FACE ( 'NONE', ( #14233 ), #3183, .F. ) ;
#33683 = LINE ( 'NONE', #14670, #46599 ) ;
#33684 = DIRECTION ( 'NONE',  ( -0.000000000000000000, -0.000000000000000000, -1.000000000000000000 ) ) ;
#33685 = CARTESIAN_POINT ( 'NONE',  ( -6.508636631827791064, -15.75743548351446854, 8.953103998512858652 ) ) ;
#33686 = FACE_OUTER_BOUND ( 'NONE', #50182, .T. ) ;
#33687 = CARTESIAN_POINT ( 'NONE',  ( 181.0000000000000853, -164.9999999999999432, -340.0000000000001137 ) ) ;
#33688 = CARTESIAN_POINT ( 'NONE',  ( 210.0000000000000568, 0.000000000000000000, -77.43171244307200141 ) ) ;
#33689 = ORIENTED_EDGE ( 'NONE', *, *, #7407, .F. ) ;
#33690 = FACE_OUTER_BOUND ( 'NONE', #33366, .T. ) ;
#33692 = VECTOR ( 'NONE', #439, 1000.000000000000000 ) ;
#33691 = CARTESIAN_POINT ( 'NONE',  ( 4.204997580903516941, -7.388441598285492518, 229.0000000000000000 ) ) ;
#33693 = FACE_OUTER_BOUND ( 'NONE', #16441, .T. ) ;
#33694 = DIRECTION ( 'NONE',  ( -1.000000000000000000, 0.000000000000000000, 0.000000000000000000 ) ) ;
#33695 = ORIENTED_EDGE ( 'NONE', *, *, #858, .T. ) ;
#33696 = LINE ( 'NONE', #38056, #32729 ) ;
#33697 = VERTEX_POINT ( 'NONE', #38625 ) ;
#33698 = FACE_OUTER_BOUND ( 'NONE', #42257, .T. ) ;
#33699 = DIRECTION ( 'NONE',  ( 0.000000000000000000, 0.000000000000000000, 1.000000000000000000 ) ) ;
#33700 = EDGE_CURVE ( 'NONE', #8841, #24012, #34518, .T. ) ;
#33701 = CARTESIAN_POINT ( 'NONE',  ( -8.445973446814976526, 0.000000000000000000, -40.93171244307205825 ) ) ;
#33702 = EDGE_CURVE ( 'NONE', #30636, #46117, #18020, .T. ) ;
#33703 = ORIENTED_EDGE ( 'NONE', *, *, #15993, .F. ) ;
#33704 = ADVANCED_FACE ( 'NONE', ( #22446 ), #38118, .T. ) ;
#33705 = EDGE_CURVE ( 'NONE', #16909, #21703, #31943, .T. ) ;
#33706 = B_SPLINE_CURVE_WITH_KNOTS ( 'NONE', 3,
 ( #37743, #41571, #1822, #16969 ),
 .UNSPECIFIED., .F., .F.,
 ( 4, 4 ),
 ( 3.806888117163228439E-16, 0.009762429729296128247 ),
 .UNSPECIFIED. ) ;
#33707 = LINE ( 'NONE', #17793, #28689 ) ;
#33708 = ORIENTED_EDGE ( 'NONE', *, *, #27646, .T. ) ;
#33709 = CARTESIAN_POINT ( 'NONE',  ( 153.3040265531850537, 1.750000000000010658, -79.18171244307201562 ) ) ;
#33710 = CARTESIAN_POINT ( 'NONE',  ( -48.33712804702535237, -13.03701565032741705, -9.367992836599951190 ) ) ;
#33711 = EDGE_CURVE ( 'NONE', #49869, #9153, #3512, .T. ) ;
#33712 = CARTESIAN_POINT ( 'NONE',  ( 130.0000000000008811, 17.00000000000000000, -24.99999999999999289 ) ) ;
#33713 = EDGE_CURVE ( 'NONE', #3086, #10429, #8331, .T. ) ;
#33714 = EDGE_LOOP ( 'NONE', ( #5478, #42163, #29589, #14578, #44402, #30173 ) ) ;
#33715 = EDGE_LOOP ( 'NONE', ( #10880, #14961, #49609, #2868 ) ) ;
#33716 = DIRECTION ( 'NONE',  ( -0.000000000000000000, -0.000000000000000000, -1.000000000000000000 ) ) ;
#33717 = DIRECTION ( 'NONE',  ( 0.000000000000000000, 0.000000000000000000, 1.000000000000000000 ) ) ;
#33718 = AXIS2_PLACEMENT_3D ( 'NONE', #28588, #1409, #47296 ) ;
#33719 = ORIENTED_EDGE ( 'NONE', *, *, #40312, .T. ) ;
#33720 = ORIENTED_EDGE ( 'NONE', *, *, #34901, .T. ) ;
#33721 = CARTESIAN_POINT ( 'NONE',  ( 75.05402655318509630, -1.025126265847089435, 162.5682875569279133 ) ) ;
#33722 = DIRECTION ( 'NONE',  ( 0.000000000000000000, 0.000000000000000000, 1.000000000000000000 ) ) ;
#33723 = DIRECTION ( 'NONE',  ( -1.000000000000000000, 0.000000000000000000, -2.958228394578794270E-31 ) ) ;
#33724 = ORIENTED_EDGE ( 'NONE', *, *, #25001, .F. ) ;
#33725 = DIRECTION ( 'NONE',  ( 0.000000000000000000, 0.000000000000000000, 1.000000000000000000 ) ) ;
#33726 = ORIENTED_EDGE ( 'NONE', *, *, #15825, .F. ) ;
#33727 = VECTOR ( 'NONE', #19825, 1000.000000000000000 ) ;
#33728 = VECTOR ( 'NONE', #25616, 1000.000000000000000 ) ;
#33729 = EDGE_CURVE ( 'NONE', #20088, #17600, #4470, .T. ) ;
#33730 = EDGE_CURVE ( 'NONE', #46304, #50236, #43217, .T. ) ;
#33731 = DIRECTION ( 'NONE',  ( 0.000000000000000000, -0.000000000000000000, -1.000000000000000000 ) ) ;
#33732 = DIRECTION ( 'NONE',  ( 0.000000000000000000, 0.000000000000000000, -1.000000000000000000 ) ) ;
#33733 = EDGE_CURVE ( 'NONE', #41468, #35739, #43713, .T. ) ;
#33734 = EDGE_CURVE ( 'NONE', #13689, #43486, #15513, .T. ) ;
#33735 = EDGE_LOOP ( 'NONE', ( #48980, #38760, #28739, #43338, #47340, #27046, #46371, #25748, #31563, #12024, #14945, #25556, #25825, #17511, #22660, #7038, #29124, #18296, #41312, #16060, #3032, #47680, #45230, #12879, #29328 ) ) ;
#33736 = EDGE_LOOP ( 'NONE', ( #37552, #32371, #13550, #2760 ) ) ;
#33737 = CARTESIAN_POINT ( 'NONE',  ( -48.44597344681496054, -1.025126265847089657, -37.43171244307202272 ) ) ;
#33738 = DIRECTION ( 'NONE',  ( 1.000000000000000000, 0.000000000000000000, 0.000000000000000000 ) ) ;
#33739 = ORIENTED_EDGE ( 'NONE', *, *, #35426, .T. ) ;
#33740 = EDGE_LOOP ( 'NONE', ( #22861, #42776, #22348, #29309, #5948, #50325, #38472, #46845 ) ) ;
#33741 = EDGE_CURVE ( 'NONE', #49918, #7079, #16532, .T. ) ;
#33742 = DIRECTION ( 'NONE',  ( 0.000000000000000000, 1.000000000000000000, 0.000000000000000000 ) ) ;
#33743 = CARTESIAN_POINT ( 'NONE',  ( 71.55402655318505367, 0.000000000000000000, -40.93171244307205825 ) ) ;
#33744 = ORIENTED_EDGE ( 'NONE', *, *, #18348, .T. ) ;
#33745 = CARTESIAN_POINT ( 'NONE',  ( -0.9599924130074112272, 0.8495346730527952861, 9.948547179989619238 ) ) ;
#33746 = DIRECTION ( 'NONE',  ( 1.000000000000000000, 0.000000000000000000, 0.000000000000000000 ) ) ;
#33747 = PLANE ( 'NONE',  #36716 ) ;
#33748 = DIRECTION ( 'NONE',  ( 1.000000000000000000, 0.000000000000000000, 0.000000000000000000 ) ) ;
#33749 = DIRECTION ( 'NONE',  ( 1.000000000000000000, 0.000000000000000000, 0.000000000000000000 ) ) ;
#33750 = ORIENTED_EDGE ( 'NONE', *, *, #32528, .T. ) ;
#33751 = ADVANCED_FACE ( 'NONE', ( #20367 ), #19859, .T. ) ;
#33752 = VECTOR ( 'NONE', #45881, 1000.000000000000000 ) ;
#33753 = LINE ( 'NONE', #6790, #21566 ) ;
#33754 = FACE_OUTER_BOUND ( 'NONE', #32070, .T. ) ;
#33755 = CARTESIAN_POINT ( 'NONE',  ( -166.6959734468149463, -1.750000000000010658, -119.1817124430720440 ) ) ;
#33756 = CARTESIAN_POINT ( 'NONE',  ( 153.3040265531850537, -1.750000000000009992, 160.8182875569279702 ) ) ;
#33757 = CARTESIAN_POINT ( 'NONE',  ( 1.222012661920449439, -0.2471648704738783342, 9.981352469109934233 ) ) ;
#33758 = VECTOR ( 'NONE', #8075, 1000.000000000000000 ) ;
#33759 = EDGE_CURVE ( 'NONE', #19764, #28669, #20118, .T. ) ;
#33760 = LINE ( 'NONE', #13227, #45788 ) ;
#33761 = CARTESIAN_POINT ( 'NONE',  ( 10.01251772323701594, 8.486842105263161073, -18.46084505325461578 ) ) ;
#33762 = CARTESIAN_POINT ( 'NONE',  ( -167.4999999999999432, 47.50000000000000000, -10.00000000000000000 ) ) ;
#33763 = ORIENTED_EDGE ( 'NONE', *, *, #27378, .F. ) ;
#33764 = FILL_AREA_STYLE ('',( #30411 ) ) ;
#33765 = EDGE_CURVE ( 'NONE', #14506, #23447, #862, .T. ) ;
#33766 = EDGE_CURVE ( 'NONE', #33142, #614, #3709, .T. ) ;
#33767 = CARTESIAN_POINT ( 'NONE',  ( 155.0540265531850537, 2.143131898507880377E-16, 165.0000000000000000 ) ) ;
#33768 = CARTESIAN_POINT ( 'NONE',  ( 0.000000000000000000, -175.0000000000000284, -353.7500000000001705 ) ) ;
#33769 = CARTESIAN_POINT ( 'NONE',  ( 2.774199659188286482, 2.805557815409694289, 6.494306517201427376 ) ) ;
#33770 = CARTESIAN_POINT ( 'NONE',  ( -48.44597344681495343, 0.000000000000000000, 39.06828755692798438 ) ) ;
#33771 = ADVANCED_FACE ( 'NONE', ( #7830 ), #19610, .F. ) ;
#33772 = ORIENTED_EDGE ( 'NONE', *, *, #17063, .T. ) ;
#33773 = VERTEX_POINT ( 'NONE', #39391 ) ;
#33774 = DIRECTION ( 'NONE',  ( -1.000000000000000000, 0.000000000000000000, -0.000000000000000000 ) ) ;
#33775 = ADVANCED_FACE ( 'NONE', ( #633 ), #23477, .T. ) ;
#33776 = DIRECTION ( 'NONE',  ( 0.000000000000000000, -1.000000000000000000, 1.604368532695312981E-16 ) ) ;
#33777 = EDGE_CURVE ( 'NONE', #48573, #13052, #38445, .T. ) ;
#33778 = ORIENTED_EDGE ( 'NONE', *, *, #33045, .F. ) ;
#33779 = CARTESIAN_POINT ( 'NONE',  ( 113.3040265531850537, 0.000000000000000000, 165.0000000000000000 ) ) ;
#33780 = DIRECTION ( 'NONE',  ( 0.000000000000000000, 1.000000000000000000, 0.000000000000000000 ) ) ;
#33781 = ORIENTED_EDGE ( 'NONE', *, *, #44492, .F. ) ;
#33782 = ORIENTED_EDGE ( 'NONE', *, *, #38811, .T. ) ;
#33783 = CIRCLE ( 'NONE', #26374, 1.880036658038868103 ) ;
#33784 = ORIENTED_EDGE ( 'NONE', *, *, #28505, .F. ) ;
#33785 = ADVANCED_FACE ( 'NONE', ( #39138 ), #28075, .T. ) ;
#33786 = DIRECTION ( 'NONE',  ( -4.996003610813203446E-16, -1.000000000000000000, 0.000000000000000000 ) ) ;
#33787 = CARTESIAN_POINT ( 'NONE',  ( -208.4459734468148611, 1.025126265847089657, -120.9317124430720440 ) ) ;
#33788 = CARTESIAN_POINT ( 'NONE',  ( 0.000000000000000000, -175.0000000000000284, 346.2500000000002274 ) ) ;
#33789 = ORIENTED_EDGE ( 'NONE', *, *, #4829, .T. ) ;
#33790 = CARTESIAN_POINT ( 'NONE',  ( 8.277096487746778308, -50.00000000000000711, 7.455576670931136185 ) ) ;
#33791 = EDGE_CURVE ( 'NONE', #49222, #9732, #47572, .T. ) ;
#33792 = VECTOR ( 'NONE', #11568, 1000.000000000000000 ) ;
#33793 = CARTESIAN_POINT ( 'NONE',  ( 339.9999999999999432, -180.9999999999999716, -356.0000000000002274 ) ) ;
#33794 = LINE ( 'NONE', #15306, #22175 ) ;
#33795 = ORIENTED_EDGE ( 'NONE', *, *, #34275, .T. ) ;
#33796 = VERTEX_POINT ( 'NONE', #39897 ) ;
#33797 = DIRECTION ( 'NONE',  ( -1.586032892321652236E-16, -1.000000000000000000, -2.288264760618012091E-48 ) ) ;
#33798 = CARTESIAN_POINT ( 'NONE',  ( -206.6959734468149463, 0.000000000000000000, 165.0000000000000000 ) ) ;
#33799 = CARTESIAN_POINT ( 'NONE',  ( 357.9999999999999432, -181.0000000000000853, 355.9999999999999432 ) ) ;
#33800 = ORIENTED_EDGE ( 'NONE', *, *, #25789, .F. ) ;
#33801 = CARTESIAN_POINT ( 'NONE',  ( -41.53730588968662829, -19.98817461849951016, 8.807470649214881320 ) ) ;
#33802 = CARTESIAN_POINT ( 'NONE',  ( 0.000000000000000000, 0.000000000000000000, 5.000000000000000000 ) ) ;
#33803 = CARTESIAN_POINT ( 'NONE',  ( 360.0000000000000000, -168.9999999999999432, 343.9999999999998295 ) ) ;
#33804 = DIRECTION ( 'NONE',  ( 0.000000000000000000, 0.000000000000000000, -1.000000000000000000 ) ) ;
#33805 = B_SPLINE_CURVE_WITH_KNOTS ( 'NONE', 3,
 ( #4086, #35154, #16384, #47642 ),
 .UNSPECIFIED., .F., .F.,
 ( 4, 4 ),
 ( 0.000000000000000000, 0.0002610106747150285275 ),
 .UNSPECIFIED. ) ;
#33806 = CARTESIAN_POINT ( 'NONE',  ( -44.94597344681493922, 2.143131898507880377E-16, 159.0682875569279702 ) ) ;
#33807 = ORIENTED_EDGE ( 'NONE', *, *, #36590, .F. ) ;
#33808 = DIRECTION ( 'NONE',  ( 1.000000000000000000, -7.930164457481157120E-16, 1.587271980518778491E-16 ) ) ;
#33809 = AXIS2_PLACEMENT_3D ( 'NONE', #8973, #44844, #21024 ) ;
#33810 = LINE ( 'NONE', #14029, #8442 ) ;
#33811 = DIRECTION ( 'NONE',  ( 0.000000000000000000, 0.000000000000000000, 1.000000000000000000 ) ) ;
#33812 = CARTESIAN_POINT ( 'NONE',  ( 164.9999999999999716, 17.00000000000000000, -114.9999999999999858 ) ) ;
#33813 =( BOUNDED_CURVE ( )  B_SPLINE_CURVE ( 3, ( #3114, #45687, #2854, #17771 ),
 .UNSPECIFIED., .F., .F. ) 
 B_SPLINE_CURVE_WITH_KNOTS ( ( 4, 4 ),
 ( 0.000000000000000000, 1.570796326794896558 ),
 .UNSPECIFIED. ) 
 CURVE ( )  GEOMETRIC_REPRESENTATION_ITEM ( )  RATIONAL_B_SPLINE_CURVE ( ( 1.000000000000000000, 0.8047378541243649375, 0.8047378541243649375, 1.000000000000000000 ) ) 
 REPRESENTATION_ITEM ( '' )  );
#33814 = CYLINDRICAL_SURFACE ( 'NONE', #15053, 1.750000000000015543 ) ;
#33815 = VECTOR ( 'NONE', #31282, 1000.000000000000000 ) ;
#33816 = EDGE_LOOP ( 'NONE', ( #17170, #7276, #34607, #6689 ) ) ;
#33817 = DIRECTION ( 'NONE',  ( -1.000000000000000000, 0.000000000000000000, 0.000000000000000000 ) ) ;
#33818 = VECTOR ( 'NONE', #38549, 1000.000000000000000 ) ;
#33819 = CARTESIAN_POINT ( 'NONE',  ( 0.3862712429686894766, -1.188820645368940276, 10.00000000000000000 ) ) ;
#33820 = CARTESIAN_POINT ( 'NONE',  ( 358.0000000000001137, 169.0000000000000000, 343.9999999999998295 ) ) ;
#33821 = CIRCLE ( 'NONE', #11687, 50.00000000000000000 ) ;
#33822 = ORIENTED_EDGE ( 'NONE', *, *, #38193, .T. ) ;
#33823 = DIRECTION ( 'NONE',  ( -1.000000000000000000, -0.000000000000000000, -0.000000000000000000 ) ) ;
#33824 = EDGE_CURVE ( 'NONE', #42504, #16599, #13680, .T. ) ;
#33825 = EDGE_CURVE ( 'NONE', #24412, #15793, #40641, .T. ) ;
#33826 = AXIS2_PLACEMENT_3D ( 'NONE', #22630, #11081, #38803 ) ;
#33827 = LINE ( 'NONE', #45583, #40133 ) ;
#33828 = ORIENTED_EDGE ( 'NONE', *, *, #28252, .T. ) ;
#33829 = CARTESIAN_POINT ( 'NONE',  ( -65.00000000000002842, 17.00000000000000000, -90.00000000000000000 ) ) ;
#33830 = PLANE ( 'NONE',  #25471 ) ;
#33831 = CARTESIAN_POINT ( 'NONE',  ( -166.6959734468149463, 1.750000000000009992, -159.1817124430720298 ) ) ;
#33832 = CARTESIAN_POINT ( 'NONE',  ( -44.94597344681493922, 2.143131898507880377E-16, 122.5682875569279702 ) ) ;
#33833 =( BOUNDED_CURVE ( )  B_SPLINE_CURVE ( 3, ( #15723, #35498, #20582, #11884 ),
 .UNSPECIFIED., .F., .F. ) 
 B_SPLINE_CURVE_WITH_KNOTS ( ( 4, 4 ),
 ( 4.712388980384689674, 6.283185307179586232 ),
 .UNSPECIFIED. ) 
 CURVE ( )  GEOMETRIC_REPRESENTATION_ITEM ( )  RATIONAL_B_SPLINE_CURVE ( ( 1.000000000000000000, 0.8047378541243649375, 0.8047378541243649375, 1.000000000000000000 ) ) 
 REPRESENTATION_ITEM ( '' )  );
#33834 = EDGE_CURVE ( 'NONE', #13231, #10537, #4971, .T. ) ;
#33835 = ORIENTED_EDGE ( 'NONE', *, *, #49699, .F. ) ;
#33836 = B_SPLINE_SURFACE_WITH_KNOTS ( 'NONE', 3, 3, ( 
 ( #14638, #6435, #14121, #10787 ),
 ( #2576, #22085, #18222, #48736 ),
 ( #1836, #33157, #49739, #10533 ),
 ( #37759, #26193, #6683, #33901 ) ),
 .UNSPECIFIED., .F., .F., .F.,
 ( 4, 4 ),
 ( 4, 4 ),
 ( 0.000000000000000000, 1.000000000000000000 ),
 ( 0.000000000000000000, 1.000000000000000000 ),
 .UNSPECIFIED. ) ;
#33837 = ORIENTED_EDGE ( 'NONE', *, *, #39751, .F. ) ;
#33838 = ORIENTED_EDGE ( 'NONE', *, *, #37795, .T. ) ;
#33839 = EDGE_CURVE ( 'NONE', #16057, #25771, #30375, .T. ) ;
#33840 = CYLINDRICAL_SURFACE ( 'NONE', #1698, 2.000000000000001776 ) ;
#33841 = EDGE_CURVE ( 'NONE', #29675, #9554, #33206, .T. ) ;
#33842 = VERTEX_POINT ( 'NONE', #24992 ) ;
#33843 = CARTESIAN_POINT ( 'NONE',  ( 340.0000000000000568, 181.0000000000000284, 343.9999999999997726 ) ) ;
#33844 = CARTESIAN_POINT ( 'NONE',  ( -0.3862712429686809279, -1.188820645368943163, -3.333333333333333481 ) ) ;
#33845 = CARTESIAN_POINT ( 'NONE',  ( 0.000000000000000000, 28.48684210526315752, 0.000000000000000000 ) ) ;
#33846 = FACE_OUTER_BOUND ( 'NONE', #23908, .T. ) ;
#33847 = ADVANCED_FACE ( 'NONE', ( #9828 ), #25484, .F. ) ;
#33848 = DIRECTION ( 'NONE',  ( -0.000000000000000000, -1.000000000000000000, 2.537652627714643577E-15 ) ) ;
#33849 = ORIENTED_EDGE ( 'NONE', *, *, #35606, .T. ) ;
#33850 = LINE ( 'NONE', #10233, #30560 ) ;
#33851 = LINE ( 'NONE', #11253, #14302 ) ;
#33852 = DIRECTION ( 'NONE',  ( -1.156482317317870492E-16, 1.000000000000000000, 0.000000000000000000 ) ) ;
#33853 = EDGE_LOOP ( 'NONE', ( #21283, #15295, #39457, #42066 ) ) ;
#33854 = CARTESIAN_POINT ( 'NONE',  ( 210.0000000000000568, 0.000000000000000000, 40.81828755692798438 ) ) ;
#33855 = CARTESIAN_POINT ( 'NONE',  ( 339.9999999999999432, -164.9999999999999432, -344.0000000000001705 ) ) ;
#33856 = ORIENTED_EDGE ( 'NONE', *, *, #1225, .T. ) ;
#33857 = VERTEX_POINT ( 'NONE', #29338 ) ;
#33858 = VERTEX_POINT ( 'NONE', #5227 ) ;
#33859 = DIRECTION ( 'NONE',  ( 0.000000000000000000, 0.000000000000000000, -1.000000000000000000 ) ) ;
#33860 = VECTOR ( 'NONE', #28994, 1000.000000000000000 ) ;
#33861 = DIRECTION ( 'NONE',  ( -0.000000000000000000, -0.000000000000000000, -1.000000000000000000 ) ) ;
#33862 = ORIENTED_EDGE ( 'NONE', *, *, #49636, .T. ) ;
#33863 = AXIS2_PLACEMENT_3D ( 'NONE', #48153, #21756, #2251 ) ;
#33864 = DIRECTION ( 'NONE',  ( -0.000000000000000000, -0.000000000000000000, -1.000000000000000000 ) ) ;
#33865 = CARTESIAN_POINT ( 'NONE',  ( 166.9999999999999716, -272.4999999999999432, -355.9999999999999432 ) ) ;
#33866 = CARTESIAN_POINT ( 'NONE',  ( 0.000000000000000000, 16.00000000000000000, 0.000000000000000000 ) ) ;
#33867 = CARTESIAN_POINT ( 'NONE',  ( -126.6959734468149321, -1.749999999999997113, 40.81828755692798438 ) ) ;
#33868 = VECTOR ( 'NONE', #2196, 1000.000000000000000 ) ;
#33869 = ORIENTED_EDGE ( 'NONE', *, *, #32712, .F. ) ;
#33870 = CARTESIAN_POINT ( 'NONE',  ( 1.104609456715839766, 0.6504863887005235545, 9.948547179989622791 ) ) ;
#33871 = DIRECTION ( 'NONE',  ( 0.000000000000000000, 0.000000000000000000, 1.000000000000000000 ) ) ;
#33872 = CARTESIAN_POINT ( 'NONE',  ( -25.60949810002096783, -43.19700938445173932, 1.847720168420772691 ) ) ;
#33873 = EDGE_CURVE ( 'NONE', #45829, #44745, #12668, .T. ) ;
#33874 = ORIENTED_EDGE ( 'NONE', *, *, #36594, .F. ) ;
#33875 = CARTESIAN_POINT ( 'NONE',  ( 355.9999999999999432, -174.9999999999999432, 359.9999999999998295 ) ) ;
#33876 = DIRECTION ( 'NONE',  ( -0.000000000000000000, -0.000000000000000000, -1.000000000000000000 ) ) ;
#33877 = CARTESIAN_POINT ( 'NONE',  ( -29.61572577327014955, -16.11461842845715253, 8.807470649214879543 ) ) ;
#33878 = DIRECTION ( 'NONE',  ( -0.000000000000000000, -0.000000000000000000, -1.000000000000000000 ) ) ;
#33879 = ORIENTED_EDGE ( 'NONE', *, *, #32983, .F. ) ;
#33880 = DIRECTION ( 'NONE',  ( -0.000000000000000000, -1.000000000000000000, -0.000000000000000000 ) ) ;
#33881 = CARTESIAN_POINT ( 'NONE',  ( -1.011271242968693862, 0.7347315653655780432, 10.00000000000000000 ) ) ;
#33882 = CARTESIAN_POINT ( 'NONE',  ( -44.94597344681493922, 2.143131898507880377E-16, -157.4317124430720014 ) ) ;
#33883 = CARTESIAN_POINT ( 'NONE',  ( -4.207128120815918256E-14, 3.058192377181588826E-14, 10.00000000000000000 ) ) ;
#33884 = CARTESIAN_POINT ( 'NONE',  ( 71.55402655318506788, 2.143131898507880377E-16, -160.9317124430720298 ) ) ;
#33885 = ORIENTED_EDGE ( 'NONE', *, *, #27489, .T. ) ;
#33886 = CYLINDRICAL_SURFACE ( 'NONE', #24810, 1.750000000000001554 ) ;
#33887 = ORIENTED_EDGE ( 'NONE', *, *, #17975, .F. ) ;
#33888 = DIRECTION ( 'NONE',  ( 1.000000000000000000, 0.000000000000000000, -0.000000000000000000 ) ) ;
#33889 = ORIENTED_EDGE ( 'NONE', *, *, #46791, .T. ) ;
#33890 = CARTESIAN_POINT ( 'NONE',  ( -8.445973446814964092, -1.025126265847097429, 42.56828755692800570 ) ) ;
#33891 = AXIS2_PLACEMENT_3D ( 'NONE', #20296, #28258, #43889 ) ;
#33892 = CARTESIAN_POINT ( 'NONE',  ( 168.9999999999999716, -81.49999999999997158, -340.0000000000001137 ) ) ;
#33893 = CARTESIAN_POINT ( 'NONE',  ( 33.30402655318503946, 1.750000000000010658, 80.81828755692798438 ) ) ;
#33894 = ORIENTED_EDGE ( 'NONE', *, *, #13142, .T. ) ;
#33895 = COLOUR_RGB ( '',0.7921568627450980005, 0.8196078431372548767, 0.9333333333333333481 ) ;
#33896 = CARTESIAN_POINT ( 'NONE',  ( -126.6959734468149321, 1.749999999999997335, 120.8182875569279702 ) ) ;
#33897 = VECTOR ( 'NONE', #14748, 1000.000000000000000 ) ;
#33898 = ORIENTED_EDGE ( 'NONE', *, *, #43098, .F. ) ;
#33899 = CARTESIAN_POINT ( 'NONE',  ( 85.00000000000090949, 17.00000000000000000, 0.000000000000000000 ) ) ;
#33900 = CARTESIAN_POINT ( 'NONE',  ( -165.6708471809677974, -1.750000000000010436, 119.7931612910808781 ) ) ;
#33901 = CARTESIAN_POINT ( 'NONE',  ( -1.011271242968683426, -0.7347315653655928092, 10.00000000000000000 ) ) ;
#33902 = DIRECTION ( 'NONE',  ( -1.586032892321652236E-16, -1.000000000000000000, -6.853681917100419162E-49 ) ) ;
#33903 = EDGE_CURVE ( 'NONE', #50159, #43847, #48283, .T. ) ;
#33904 = CARTESIAN_POINT ( 'NONE',  ( -48.44597344681496054, -1.025126265847089657, -80.93171244307201562 ) ) ;
#33905 = ORIENTED_EDGE ( 'NONE', *, *, #40902, .T. ) ;
#33906 = ORIENTED_EDGE ( 'NONE', *, *, #8586, .T. ) ;
#33907 = CARTESIAN_POINT ( 'NONE',  ( 33.30402655318503946, -1.750000000000010658, 120.8182875569279702 ) ) ;
#33908 = VECTOR ( 'NONE', #33483, 1000.000000000000000 ) ;
#33909 = ORIENTED_EDGE ( 'NONE', *, *, #20192, .T. ) ;
#33910 = CARTESIAN_POINT ( 'NONE',  ( -0.9341213539222554818, -1.950087977540069684, 9.885585981620945262 ) ) ;
#33911 = CARTESIAN_POINT ( 'NONE',  ( -8.445973446814976526, 0.000000000000000000, -80.93171244307204404 ) ) ;
#33912 =( BOUNDED_CURVE ( )  B_SPLINE_CURVE ( 3, ( #25128, #37449, #21512, #21020 ),
 .UNSPECIFIED., .F., .F. ) 
 B_SPLINE_CURVE_WITH_KNOTS ( ( 4, 4 ),
 ( 3.141592653589793116, 4.712388980384689674 ),
 .UNSPECIFIED. ) 
 CURVE ( )  GEOMETRIC_REPRESENTATION_ITEM ( )  RATIONAL_B_SPLINE_CURVE ( ( 1.000000000000000000, 0.8047378541243649375, 0.8047378541243649375, 1.000000000000000000 ) ) 
 REPRESENTATION_ITEM ( '' )  );
#33913 = ORIENTED_EDGE ( 'NONE', *, *, #45883, .F. ) ;
#33914 = LINE ( 'NONE', #30311, #36044 ) ;
#33915 = LINE ( 'NONE', #50005, #7921 ) ;
#33916 = ORIENTED_EDGE ( 'NONE', *, *, #30306, .T. ) ;
#33917 = DIRECTION ( 'NONE',  ( 0.000000000000000000, 0.000000000000000000, -1.000000000000000000 ) ) ;
#33918 = DIRECTION ( 'NONE',  ( -1.000000000000000000, 0.000000000000000000, 0.000000000000000000 ) ) ;
#33919 = LINE ( 'NONE', #28361, #39415 ) ;
#33920 = LINE ( 'NONE', #50010, #37862 ) ;
#33921 = ORIENTED_EDGE ( 'NONE', *, *, #36825, .F. ) ;
#33922 = VECTOR ( 'NONE', #43599, 1000.000000000000000 ) ;
#33923 = ORIENTED_EDGE ( 'NONE', *, *, #13714, .T. ) ;
#33924 = AXIS2_PLACEMENT_3D ( 'NONE', #6005, #25261, #21157 ) ;
#33925 = DIRECTION ( 'NONE',  ( -0.000000000000000000, -0.000000000000000000, -1.000000000000000000 ) ) ;
#33926 = ORIENTED_EDGE ( 'NONE', *, *, #25839, .T. ) ;
#33927 = AXIS2_PLACEMENT_3D ( 'NONE', #203, #15840, #31502 ) ;
#33928 = EDGE_CURVE ( 'NONE', #12513, #36229, #5726, .T. ) ;
#33929 = ORIENTED_EDGE ( 'NONE', *, *, #14343, .F. ) ;
#33930 = VECTOR ( 'NONE', #11013, 1000.000000000000000 ) ;
#33931 = DIRECTION ( 'NONE',  ( 0.000000000000000000, 1.000000000000000000, 0.000000000000000000 ) ) ;
#33932 = DIRECTION ( 'NONE',  ( 0.000000000000000000, -2.537652627714643577E-15, -1.000000000000000000 ) ) ;
#33933 = CARTESIAN_POINT ( 'NONE',  ( 85.00000000000056843, 16.00000000000000000, -54.99999999999999289 ) ) ;
#33934 = DIRECTION ( 'NONE',  ( 0.000000000000000000, -1.000000000000000000, 0.000000000000000000 ) ) ;
#33935 = CARTESIAN_POINT ( 'NONE',  ( 185.0000000000000000, -174.9999999999999716, -356.0000000000001705 ) ) ;
#33936 = CARTESIAN_POINT ( 'NONE',  ( -168.4459734468149747, -1.025126265847089657, -120.9317124430720440 ) ) ;
#33937 = ORIENTED_EDGE ( 'NONE', *, *, #45529, .F. ) ;
#33938 = DIRECTION ( 'NONE',  ( -1.000000000000000000, 0.000000000000000000, 0.000000000000000000 ) ) ;
#33939 = PRODUCT_DEFINITION_SHAPE ( 'NONE', 'NONE',  #29665 ) ;
#33940 = CARTESIAN_POINT ( 'NONE',  ( -225.0000000000000568, -175.0000000000000000, 500.0000000000000000 ) ) ;
#33941 = CARTESIAN_POINT ( 'NONE',  ( 167.0000000000000000, -174.9999999999999716, -99.00000000000014211 ) ) ;
#33942 = VECTOR ( 'NONE', #28682, 1000.000000000000000 ) ;
#33943 = CARTESIAN_POINT ( 'NONE',  ( 17.23491422248386584, -0.5912720620000816441, 8.727788335465566760 ) ) ;
#33944 = ORIENTED_EDGE ( 'NONE', *, *, #10521, .F. ) ;
#33945 = LINE ( 'NONE', #26248, #9777 ) ;
#33946 = ORIENTED_EDGE ( 'NONE', *, *, #25726, .F. ) ;
#33947 = DIRECTION ( 'NONE',  ( -1.000000000000000000, 0.000000000000000000, 0.000000000000000000 ) ) ;
#33948 = LINE ( 'NONE', #6483, #17546 ) ;
#33949 = DIRECTION ( 'NONE',  ( -1.000000000000000000, -0.000000000000000000, -0.000000000000000000 ) ) ;
#33950 = EDGE_LOOP ( 'NONE', ( #45412, #40837, #11255, #8679, #40678, #45849 ) ) ;
#33951 = LINE ( 'NONE', #6742, #35269 ) ;
#33952 = ORIENTED_EDGE ( 'NONE', *, *, #39909, .F. ) ;
#33953 = CARTESIAN_POINT ( 'NONE',  ( 30.12518629743562926, 14.70074613238908157, 1.847720168420772691 ) ) ;
#33954 = CARTESIAN_POINT ( 'NONE',  ( -14.49999999999999822, 13.48684210526315930, 19.37312575500900280 ) ) ;
#33955 = CARTESIAN_POINT ( 'NONE',  ( -114.9999999999997158, 16.00000000000000000, -60.00000000000000000 ) ) ;
#33956 = EDGE_CURVE ( 'NONE', #31581, #40535, #48793, .T. ) ;
#33957 = VECTOR ( 'NONE', #42128, 1000.000000000000000 ) ;
#33958 = ORIENTED_EDGE ( 'NONE', *, *, #24404, .F. ) ;
#33959 = EDGE_LOOP ( 'NONE', ( #20694, #13826, #39380, #39476, #36746, #13076 ) ) ;
#33960 = CARTESIAN_POINT ( 'NONE',  ( -208.4459734468149463, 0.000000000000000000, 162.5682875569279702 ) ) ;
#33961 = AXIS2_PLACEMENT_3D ( 'NONE', #47187, #12084, #31848 ) ;
#33962 = CARTESIAN_POINT ( 'NONE',  ( 14.29087950072012170, 9.652079258044652832, 8.727788335465566760 ) ) ;
#33963 =( BOUNDED_CURVE ( )  B_SPLINE_CURVE ( 3, ( #15713, #34992, #30612, #31385 ),
 .UNSPECIFIED., .F., .F. ) 
 B_SPLINE_CURVE_WITH_KNOTS ( ( 4, 4 ),
 ( 3.141592653589793116, 4.712388980384689674 ),
 .UNSPECIFIED. ) 
 CURVE ( )  GEOMETRIC_REPRESENTATION_ITEM ( )  RATIONAL_B_SPLINE_CURVE ( ( 1.000000000000000000, 0.8047378541243649375, 0.8047378541243649375, 1.000000000000000000 ) ) 
 REPRESENTATION_ITEM ( '' )  );
#33964 = VERTEX_POINT ( 'NONE', #5473 ) ;
#33965 = ORIENTED_EDGE ( 'NONE', *, *, #30104, .F. ) ;
#33966 = LINE ( 'NONE', #13938, #37280 ) ;
#33967 = CARTESIAN_POINT ( 'NONE',  ( -15.42815683172655028, -34.17926237904570996, 7.697694107796190899 ) ) ;
#33968 = DIRECTION ( 'NONE',  ( -0.000000000000000000, -0.000000000000000000, -1.000000000000000000 ) ) ;
#33969 = ORIENTED_EDGE ( 'NONE', *, *, #36185, .T. ) ;
#33970 = CYLINDRICAL_SURFACE ( 'NONE', #27636, 1.750000000000008438 ) ;
#33971 = ORIENTED_EDGE ( 'NONE', *, *, #23017, .T. ) ;
#33972 = EDGE_CURVE ( 'NONE', #21418, #14525, #35645, .T. ) ;
#33973 =( BOUNDED_CURVE ( )  B_SPLINE_CURVE ( 3, ( #26051, #32565, #1755, #28699 ),
 .UNSPECIFIED., .F., .F. ) 
 B_SPLINE_CURVE_WITH_KNOTS ( ( 4, 4 ),
 ( 5.723266580096323608, 6.283185307179586232 ),
 .UNSPECIFIED. ) 
 CURVE ( )  GEOMETRIC_REPRESENTATION_ITEM ( )  RATIONAL_B_SPLINE_CURVE ( ( 1.000000000000000000, 0.9740444450880465510, 0.9740444450880465510, 1.000000000000000000 ) ) 
 REPRESENTATION_ITEM ( '' )  );
#33974 = EDGE_CURVE ( 'NONE', #46680, #34035, #16779, .T. ) ;
#33975 = LINE ( 'NONE', #50320, #16073 ) ;
#33976 = EDGE_CURVE ( 'NONE', #47608, #17007, #40140, .T. ) ;
#33977 = CARTESIAN_POINT ( 'NONE',  ( -48.44597344681496054, -1.025126265847089657, -120.9317124430720440 ) ) ;
#33978 = AXIS2_PLACEMENT_3D ( 'NONE', #33935, #13902, #21883 ) ;
#33979 = EDGE_LOOP ( 'NONE', ( #3073, #14863, #24124, #27027 ) ) ;
#33980 = ORIENTED_EDGE ( 'NONE', *, *, #13144, .F. ) ;
#33981 = VECTOR ( 'NONE', #34376, 1000.000000000000000 ) ;
#33982 = CARTESIAN_POINT ( 'NONE',  ( 112.2789002873379758, -1.749999999999996669, 161.8434138227750907 ) ) ;
#33983 = CARTESIAN_POINT ( 'NONE',  ( -29.61572577327014955, -16.11461842845715253, 8.807470649214879543 ) ) ;
#33984 = ORIENTED_EDGE ( 'NONE', *, *, #39968, .F. ) ;
#33985 = CARTESIAN_POINT ( 'NONE',  ( 358.0000000000000000, -168.9999999999999432, 343.9999999999998295 ) ) ;
#33986 = EDGE_CURVE ( 'NONE', #15558, #9775, #1091, .T. ) ;
#33987 = EDGE_CURVE ( 'NONE', #21583, #18090, #13272, .T. ) ;
#33988 = ORIENTED_EDGE ( 'NONE', *, *, #44672, .F. ) ;
#33989 = FACE_OUTER_BOUND ( 'NONE', #4184, .T. ) ;
#33990 = DIRECTION ( 'NONE',  ( -1.000000000000000000, -0.000000000000000000, -0.000000000000000000 ) ) ;
#33991 = ORIENTED_EDGE ( 'NONE', *, *, #35597, .T. ) ;
#33992 = CARTESIAN_POINT ( 'NONE',  ( -47.72109971266203132, -1.750000000000010214, -78.15658617722490931 ) ) ;
#33993 = ADVANCED_FACE ( 'NONE', ( #21374 ), #17285, .T. ) ;
#33994 = DIRECTION ( 'NONE',  ( 0.000000000000000000, 6.123233995736766036E-17, -1.000000000000000000 ) ) ;
#33995 = CARTESIAN_POINT ( 'NONE',  ( 130.0000000000002842, 17.00000000000000000, -84.99999999999998579 ) ) ;
#33996 = FACE_OUTER_BOUND ( 'NONE', #9946, .T. ) ;
#33997 = EDGE_CURVE ( 'NONE', #10490, #22721, #18271, .T. ) ;
#33998 = AXIS2_PLACEMENT_3D ( 'NONE', #9849, #25502, #30114 ) ;
#33999 = CARTESIAN_POINT ( 'NONE',  ( 31.55402655318503236, 1.025126265847089435, -77.43171244307200141 ) ) ;
#34000 = ORIENTED_EDGE ( 'NONE', *, *, #30391, .T. ) ;
#34001 = CYLINDRICAL_SURFACE ( 'NONE', #12462, 3.500000000000003109 ) ;
#34002 = EDGE_CURVE ( 'NONE', #37518, #10906, #7247, .T. ) ;
#34003 = CARTESIAN_POINT ( 'NONE',  ( -2.188678504086925880, 0.3267089737526900350, 9.881002359080270026 ) ) ;
#34004 = CYLINDRICAL_SURFACE ( 'NONE', #8085, 1.750000000000008438 ) ;
#34005 = CARTESIAN_POINT ( 'NONE',  ( 357.9999999999999432, -181.0000000000000853, 355.9999999999999432 ) ) ;
#34006 = AXIS2_PLACEMENT_3D ( 'NONE', #18309, #13962, #22426 ) ;
#34007 = CARTESIAN_POINT ( 'NONE',  ( -1.810969182959400570, 3.505385724216297127, 6.494306115487985309 ) ) ;
#34008 = FACE_OUTER_BOUND ( 'NONE', #33319, .T. ) ;
#34009 = LINE ( 'NONE', #30148, #37678 ) ;
#34010 = DIRECTION ( 'NONE',  ( 1.000000000000000000, 0.000000000000000000, -4.625929269271635797E-16 ) ) ;
#34011 = ADVANCED_FACE ( 'NONE', ( #2622 ), #18775, .T. ) ;
#34012 = LINE ( 'NONE', #34261, #22213 ) ;
#34013 = ORIENTED_EDGE ( 'NONE', *, *, #34312, .F. ) ;
#34014 = FACE_OUTER_BOUND ( 'NONE', #39103, .T. ) ;
#34015 = AXIS2_PLACEMENT_3D ( 'NONE', #37942, #2258, #5598 ) ;
#34016 = ADVANCED_FACE ( 'NONE', ( #49287 ), #22890, .T. ) ;
#34017 = ADVANCED_FACE ( 'NONE', ( #41637 ), #14439, .T. ) ;
#34018 = CARTESIAN_POINT ( 'NONE',  ( -6.695973446814940111, -1.750000000000023759, 40.81828755692798438 ) ) ;
#34019 = VECTOR ( 'NONE', #32948, 1000.000000000000000 ) ;
#34020 = CARTESIAN_POINT ( 'NONE',  ( -1.114871695981121125, 0.4953159757245923500, 9.963925895596188909 ) ) ;
#34021 = DIRECTION ( 'NONE',  ( -1.586032892321652236E-16, -1.194346094642792789E-32, -1.000000000000000000 ) ) ;
#34022 = CARTESIAN_POINT ( 'NONE',  ( -4.999999999999947597, -222.4999999999999716, -228.6347188485896140 ) ) ;
#34023 = EDGE_CURVE ( 'NONE', #1790, #15177, #30100, .T. ) ;
#34024 = EDGE_LOOP ( 'NONE', ( #3896, #43722, #42472, #1099, #48803, #10900 ) ) ;
#34025 = VERTEX_POINT ( 'NONE', #14946 ) ;
#34026 = CARTESIAN_POINT ( 'NONE',  ( -0.9390173899430289683, -1.130417317737636651, 9.958264684458541183 ) ) ;
#34027 = ADVANCED_FACE ( 'NONE', ( #13915 ), #21896, .F. ) ;
#34028 = CARTESIAN_POINT ( 'NONE',  ( -48.44597344681496054, 1.025126265847089213, -0.9317124430720324924 ) ) ;
#34029 = VECTOR ( 'NONE', #622, 1000.000000000000000 ) ;
#34030 = EDGE_LOOP ( 'NONE', ( #31980, #44657, #29248, #44519, #32852 ) ) ;
#34031 = CARTESIAN_POINT ( 'NONE',  ( 6.174150299305392053, -33.14591993373988998, 8.807470649214879543 ) ) ;
#34032 = CARTESIAN_POINT ( 'NONE',  ( 35.00000000000122213, 17.00000000000000000, 5.000000000000004441 ) ) ;
#34033 = CARTESIAN_POINT ( 'NONE',  ( 32.27890028733795447, 1.750000000000009548, -0.2068387089191121020 ) ) ;
#34034 = VECTOR ( 'NONE', #50200, 1000.000000000000000 ) ;
#34035 = VERTEX_POINT ( 'NONE', #10580 ) ;
#34036 = ORIENTED_EDGE ( 'NONE', *, *, #15258, .T. ) ;
#34037 = ORIENTED_EDGE ( 'NONE', *, *, #46296, .T. ) ;
#34038 = PRODUCT_DEFINITION_FORMATION_WITH_SPECIFIED_SOURCE ( 'ANY', '', #17099, .NOT_KNOWN. ) ;
#34039 = AXIS2_PLACEMENT_3D ( 'NONE', #8564, #366, #35522 ) ;
#34040 = DIRECTION ( 'NONE',  ( -1.156482317317870492E-16, 1.000000000000000000, 0.000000000000000000 ) ) ;
#34041 = CARTESIAN_POINT ( 'NONE',  ( 210.0000000000000568, 0.000000000000000000, 80.81828755692798438 ) ) ;
#34042 = CARTESIAN_POINT ( 'NONE',  ( -1.011271242968693862, 0.7347315653655780432, -10.00000000000000000 ) ) ;
#34043 = ORIENTED_EDGE ( 'NONE', *, *, #4704, .F. ) ;
#34044 = CYLINDRICAL_SURFACE ( 'NONE', #1390, 2.000000000000001776 ) ;
#34045 = CYLINDRICAL_SURFACE ( 'NONE', #9961, 4.000000000000003553 ) ;
#34046 = CARTESIAN_POINT ( 'NONE',  ( 350.0000000000000000, 181.0000000000000284, -340.0000000000001705 ) ) ;
#34047 = ORIENTED_EDGE ( 'NONE', *, *, #40185, .T. ) ;
#34048 = EDGE_CURVE ( 'NONE', #14610, #34262, #26251, .T. ) ;
#34049 = ORIENTED_EDGE ( 'NONE', *, *, #27702, .F. ) ;
#34050 = PLANE ( 'NONE',  #11481 ) ;
#34051 = CARTESIAN_POINT ( 'NONE',  ( -0.3862712429686809279, -1.188820645368943163, -3.333333333333333481 ) ) ;
#34052 = CARTESIAN_POINT ( 'NONE',  ( 358.0000000000000568, -182.1715728752539292, 357.1715728752538439 ) ) ;
#34053 = ORIENTED_EDGE ( 'NONE', *, *, #5264, .F. ) ;
#34054 = CARTESIAN_POINT ( 'NONE',  ( -5.670847180967843570, -1.750000000000023315, -38.15658617722493062 ) ) ;
#34055 = SURFACE_STYLE_USAGE ( .BOTH. , #37914 ) ;
#34056 = EDGE_CURVE ( 'NONE', #26176, #35933, #11095, .T. ) ;
#34057 = AXIS2_PLACEMENT_3D ( 'NONE', #30881, #15457, #46214 ) ;
#34058 = CYLINDRICAL_SURFACE ( 'NONE', #18639, 1.750000000000010214 ) ;
#34059 = DIRECTION ( 'NONE',  ( -1.000000000000000000, 0.000000000000000000, 0.000000000000000000 ) ) ;
#34060 = ADVANCED_FACE ( 'NONE', ( #22142 ), #18529, .F. ) ;
#34061 = CARTESIAN_POINT ( 'NONE',  ( 0.6595498452743703277, -16.59563386392009576, 3.266473740018926541 ) ) ;
#34062 = CIRCLE ( 'NONE', #18470, 2.000000000000001776 ) ;
#34063 = VERTEX_POINT ( 'NONE', #34209 ) ;
#34064 = EDGE_CURVE ( 'NONE', #35344, #42209, #21324, .T. ) ;
#34065 = DIRECTION ( 'NONE',  ( 0.000000000000000000, 0.000000000000000000, -1.000000000000000000 ) ) ;
#34066 = EDGE_CURVE ( 'NONE', #37688, #18558, #49784, .T. ) ;
#34068 = AXIS2_PLACEMENT_3D ( 'NONE', #48517, #21615, #18254 ) ;
#34067 = CARTESIAN_POINT ( 'NONE',  ( -45.67084718096785423, 1.750000000000009548, -160.2068387089191219 ) ) ;
#34069 = DIRECTION ( 'NONE',  ( 0.000000000000000000, 1.000000000000000000, 0.000000000000000000 ) ) ;
#34070 = ADVANCED_FACE ( 'NONE', ( #14685 ), #2383, .T. ) ;
#34071 = LINE ( 'NONE', #13276, #5839 ) ;
#34072 = VECTOR ( 'NONE', #10235, 1000.000000000000000 ) ;
#34074 = AXIS2_PLACEMENT_3D ( 'NONE', #33110, #40290, #28742 ) ;
#34073 = DIRECTION ( 'NONE',  ( 0.000000000000000000, 2.537652627714642000E-15, 1.000000000000000000 ) ) ;
#34075 = VERTEX_POINT ( 'NONE', #34458 ) ;
#34076 = LINE ( 'NONE', #21748, #13047 ) ;
#34077 = CARTESIAN_POINT ( 'NONE',  ( -64.99999999999815259, 17.00000000000000000, 65.00000000000000000 ) ) ;
#34078 = VECTOR ( 'NONE', #10194, 1000.000000000000000 ) ;
#34079 = VECTOR ( 'NONE', #19624, 1000.000000000000000 ) ;
#34080 = ORIENTED_EDGE ( 'NONE', *, *, #247, .T. ) ;
#34081 = DIRECTION ( 'NONE',  ( -1.000000000000000000, 0.000000000000000000, 0.000000000000000000 ) ) ;
#34082 = EDGE_CURVE ( 'NONE', #46117, #39523, #18026, .T. ) ;
#34083 = LINE ( 'NONE', #45076, #10624 ) ;
#34084 = ORIENTED_EDGE ( 'NONE', *, *, #12993, .F. ) ;
#34085 = CARTESIAN_POINT ( 'NONE',  ( -0.4612239888288630074, 1.380789889681132365, 9.938560701278168708 ) ) ;
#34086 = DIRECTION ( 'NONE',  ( -1.122149248522496843E-16, 0.7071067811865476838, 0.7071067811865474617 ) ) ;
#34087 = CARTESIAN_POINT ( 'NONE',  ( 240.0000000000000000, -164.9999999999999716, 32.29650858650035161 ) ) ;
#34088 = DIRECTION ( 'NONE',  ( -1.000000000000000000, -0.000000000000000000, -0.000000000000000000 ) ) ;
#34089 = ORIENTED_EDGE ( 'NONE', *, *, #27707, .F. ) ;
#34090 = CARTESIAN_POINT ( 'NONE',  ( -27.31081730472607561, -41.96092862852123773, 3.199614146704519602 ) ) ;
#34091 = PRODUCT_RELATED_PRODUCT_CATEGORY ( 'part', '', ( #17099 ) ) ;
#34092 = EDGE_LOOP ( 'NONE', ( #16596, #7419, #4506, #2211 ) ) ;
#34093 = ORIENTED_EDGE ( 'NONE', *, *, #3616, .T. ) ;
#34094 = DIRECTION ( 'NONE',  ( 0.000000000000000000, 0.000000000000000000, 1.000000000000000000 ) ) ;
#34095 = VECTOR ( 'NONE', #10534, 1000.000000000000000 ) ;
#34096 = EDGE_LOOP ( 'NONE', ( #40638, #38660 ) ) ;
#34097 = LINE ( 'NONE', #45834, #5717 ) ;
#34098 = CARTESIAN_POINT ( 'NONE',  ( 343.9999999999997158, -165.0000000000001137, -90.00000000000018474 ) ) ;
#34099 = AXIS2_PLACEMENT_3D ( 'NONE', #20392, #10110, #10374 ) ;
#34100 = DIRECTION ( 'NONE',  ( 0.000000000000000000, 0.000000000000000000, -1.000000000000000000 ) ) ;
#34101 = ADVANCED_FACE ( 'NONE', ( #33698 ), #45453, .T. ) ;
#34102 = CARTESIAN_POINT ( 'NONE',  ( 3.975459390375365665, 0.2195152216756870167, 1.992221491942114397E-15 ) ) ;
#34103 = ORIENTED_EDGE ( 'NONE', *, *, #40941, .T. ) ;
#34104 = CYLINDRICAL_SURFACE ( 'NONE', #34676, 1.750000000000001554 ) ;
#34105 = CARTESIAN_POINT ( 'NONE',  ( -128.4459734468149179, 0.000000000000000000, -40.93171244307202983 ) ) ;
#34106 = DIRECTION ( 'NONE',  ( -1.000000000000000000, 0.000000000000000000, -0.000000000000000000 ) ) ;
#34107 = EDGE_LOOP ( 'NONE', ( #8274, #14039, #1366, #17341 ) ) ;
#34108 = CARTESIAN_POINT ( 'NONE',  ( 155.0540265531850537, 2.143131898507880377E-16, 165.0000000000000000 ) ) ;
#34109 = LINE ( 'NONE', #30244, #35167 ) ;
#34110 = ORIENTED_EDGE ( 'NONE', *, *, #39367, .T. ) ;
#34111 = VECTOR ( 'NONE', #18561, 1000.000000000000000 ) ;
#34112 = ORIENTED_EDGE ( 'NONE', *, *, #15418, .F. ) ;
#34113 = ORIENTED_EDGE ( 'NONE', *, *, #45832, .F. ) ;
#34114 = DIRECTION ( 'NONE',  ( -1.000000000000000000, 1.586032997072805650E-16, 4.759647537211363479E-16 ) ) ;
#34115 = FACE_OUTER_BOUND ( 'NONE', #14988, .T. ) ;
#34116 = ORIENTED_EDGE ( 'NONE', *, *, #11657, .T. ) ;
#34117 = AXIS2_PLACEMENT_3D ( 'NONE', #36509, #12878, #1345 ) ;
#34118 = CARTESIAN_POINT ( 'NONE',  ( -208.4459734468148611, 1.025126265847089213, -0.9317124430720324924 ) ) ;
#34119 = CARTESIAN_POINT ( 'NONE',  ( -64.99999999999846523, 17.00000000000000000, 60.00000000000000000 ) ) ;
#34120 =( BOUNDED_CURVE ( )  B_SPLINE_CURVE ( 3, ( #18943, #23053, #2794, #3815 ),
 .UNSPECIFIED., .F., .F. ) 
 B_SPLINE_CURVE_WITH_KNOTS ( ( 4, 4 ),
 ( 1.570796326794896558, 3.141592653589793116 ),
 .UNSPECIFIED. ) 
 CURVE ( )  GEOMETRIC_REPRESENTATION_ITEM ( )  RATIONAL_B_SPLINE_CURVE ( ( 1.000000000000000000, 0.8047378541243649375, 0.8047378541243649375, 1.000000000000000000 ) ) 
 REPRESENTATION_ITEM ( '' )  );
#34121 = CARTESIAN_POINT ( 'NONE',  ( 181.0000000000000000, -184.9999999999999716, -115.0000000000001279 ) ) ;
#34122 = ADVANCED_FACE ( 'NONE', ( #31879 ), #34721, .F. ) ;
#34123 = DIRECTION ( 'NONE',  ( 0.000000000000000000, 0.000000000000000000, 1.000000000000000000 ) ) ;
#34124 = DIRECTION ( 'NONE',  ( 1.000000000000000000, 0.000000000000000000, 0.000000000000000000 ) ) ;
#34125 = ADVANCED_FACE ( 'NONE', ( #39320 ), #23622, .T. ) ;
#34126 = ORIENTED_EDGE ( 'NONE', *, *, #39339, .F. ) ;
#34127 = CARTESIAN_POINT ( 'NONE',  ( 11.73320209285708415, -11.96063479729170886, 9.403735324607438884 ) ) ;
#34128 =( BOUNDED_CURVE ( )  B_SPLINE_CURVE ( 3, ( #6298, #10890, #13973, #21678 ),
 .UNSPECIFIED., .F., .F. ) 
 B_SPLINE_CURVE_WITH_KNOTS ( ( 4, 4 ),
 ( 1.570796326794896558, 3.141592653589793116 ),
 .UNSPECIFIED. ) 
 CURVE ( )  GEOMETRIC_REPRESENTATION_ITEM ( )  RATIONAL_B_SPLINE_CURVE ( ( 1.000000000000000000, 0.8047378541243649375, 0.8047378541243649375, 1.000000000000000000 ) ) 
 REPRESENTATION_ITEM ( '' )  );
#34129 = ADVANCED_FACE ( 'NONE', ( #326 ), #31106, .T. ) ;
#34130 = LINE ( 'NONE', #26152, #16630 ) ;
#34131 = ORIENTED_EDGE ( 'NONE', *, *, #23753, .F. ) ;
#34132 = EDGE_CURVE ( 'NONE', #21529, #5410, #8524, .T. ) ;
#34133 = ITEM_DEFINED_TRANSFORMATION ( 'NONE', 'NONE', #26669,  #45486 ) ;
#34134 = ADVANCED_FACE ( 'NONE', ( #31631 ), #47220, .T. ) ;
#34135 = CARTESIAN_POINT ( 'NONE',  ( -204.9459734468149463, 2.143131898507880377E-16, -40.93171244307202983 ) ) ;
#34136 = CARTESIAN_POINT ( 'NONE',  ( -36.62549812225767454, -8.082823558958592614, -8.600750091277035381 ) ) ;
#34137 = CIRCLE ( 'NONE', #32489, 4.000000000000003553 ) ;
#34138 = VECTOR ( 'NONE', #20832, 1000.000000000000000 ) ;
#34140 = VECTOR ( 'NONE', #9053, 1000.000000000000000 ) ;
#34139 = CARTESIAN_POINT ( 'NONE',  ( 111.5540265531850537, 1.025126265847081219, 2.568287556927973281 ) ) ;
#34141 = CARTESIAN_POINT ( 'NONE',  ( -7.822422304254325276, -2.816136035261162185, 226.0000000000000000 ) ) ;
#34142 = VERTEX_POINT ( 'NONE', #43160 ) ;
#34143 = B_SPLINE_CURVE_WITH_KNOTS ( 'NONE', 3,
 ( #10034, #5171, #1587, #25182 ),
 .UNSPECIFIED., .F., .F.,
 ( 4, 4 ),
 ( 0.0009539133080771172290, 0.009404495247862900906 ),
 .UNSPECIFIED. ) ;
#34144 = CARTESIAN_POINT ( 'NONE',  ( 168.9999999999999716, 10.00000000000006395, -350.0000000000001705 ) ) ;
#34145 = DIRECTION ( 'NONE',  ( 0.000000000000000000, 1.000000000000000000, 0.000000000000000000 ) ) ;
#34146 = EDGE_CURVE ( 'NONE', #45351, #28634, #34982, .T. ) ;
#34147 =( BOUNDED_CURVE ( )  B_SPLINE_CURVE ( 3, ( #28543, #6208, #1355, #13878 ),
 .UNSPECIFIED., .F., .F. ) 
 B_SPLINE_CURVE_WITH_KNOTS ( ( 4, 4 ),
 ( 4.712388980384689674, 6.283185307179586232 ),
 .UNSPECIFIED. ) 
 CURVE ( )  GEOMETRIC_REPRESENTATION_ITEM ( )  RATIONAL_B_SPLINE_CURVE ( ( 1.000000000000000000, 0.8047378541243649375, 0.8047378541243649375, 1.000000000000000000 ) ) 
 REPRESENTATION_ITEM ( '' )  );
#34148 = CARTESIAN_POINT ( 'NONE',  ( 47.88254548617766204, -14.43607691413525984, -3.760136334089591248 ) ) ;
#34149 = CARTESIAN_POINT ( 'NONE',  ( -0.7757854888975277419, -0.3020624223403916564, 9.985686052694763504 ) ) ;
#34150 = CARTESIAN_POINT ( 'NONE',  ( 111.5540265531850537, 1.025126265847081664, 82.56828755692798438 ) ) ;
#34151 = VECTOR ( 'NONE', #8235, 1000.000000000000000 ) ;
#34152 = ORIENTED_EDGE ( 'NONE', *, *, #48551, .F. ) ;
#34153 = CARTESIAN_POINT ( 'NONE',  ( -225.0000000000000568, -165.6999999999999602, 250.3600000000000136 ) ) ;
#34154 = EDGE_LOOP ( 'NONE', ( #38400, #36232, #42344, #3332 ) ) ;
#34155 = FACE_OUTER_BOUND ( 'NONE', #11596, .T. ) ;
#34156 = VECTOR ( 'NONE', #5635, 1000.000000000000000 ) ;
#34157 = VERTEX_POINT ( 'NONE', #11610 ) ;
#34158 = CARTESIAN_POINT ( 'NONE',  ( -14.49999999999999822, -46.01315789473684248, -5.916985404131814619 ) ) ;
#34159 = CARTESIAN_POINT ( 'NONE',  ( 34.32915281903212446, 1.750000000000010214, -80.20683870891910772 ) ) ;
#34160 = ORIENTED_EDGE ( 'NONE', *, *, #41343, .T. ) ;
#34161 =( LENGTH_UNIT ( ) NAMED_UNIT ( * ) SI_UNIT ( .MILLI., .METRE. ) );
#34162 = EDGE_LOOP ( 'NONE', ( #9523, #31963, #1546, #4038, #6417, #31720 ) ) ;
#34163 = CYLINDRICAL_SURFACE ( 'NONE', #23692, 2.000000000000001776 ) ;
#34164 = VERTEX_POINT ( 'NONE', #38818 ) ;
#34165 = LINE ( 'NONE', #14636, #27034 ) ;
#34166 = DIRECTION ( 'NONE',  ( -1.612977847700450206E-50, 0.000000000000000000, -1.000000000000000000 ) ) ;
#34167 = LINE ( 'NONE', #30298, #35241 ) ;
#34168 = CARTESIAN_POINT ( 'NONE',  ( 191.5540265531851105, 0.000000000000000000, -157.4317124430720582 ) ) ;
#34169 = VERTEX_POINT ( 'NONE', #39574 ) ;
#34170 = ORIENTED_EDGE ( 'NONE', *, *, #50642, .T. ) ;
#34171 = CARTESIAN_POINT ( 'NONE',  ( -16.99749102614300966, 1.320765928724422222, 8.953103998512858652 ) ) ;
#34172 = ADVANCED_FACE ( 'NONE', ( #43644 ), #46710, .T. ) ;
#34173 = VERTEX_POINT ( 'NONE', #19293 ) ;
#34174 = DIRECTION ( 'NONE',  ( 1.000000000000000000, 0.000000000000000000, 0.000000000000000000 ) ) ;
#34175 = VERTEX_POINT ( 'NONE', #15205 ) ;
#34176 = DIRECTION ( 'NONE',  ( -0.8411784753765545464, 0.000000000000000000, 0.5407575913134972101 ) ) ;
#34177 = B_SPLINE_CURVE_WITH_KNOTS ( 'NONE', 3,
 ( #45269, #11174, #41955, #30156 ),
 .UNSPECIFIED., .F., .F.,
 ( 4, 4 ),
 ( 2.219577935476692653E-17, 0.0003407397535652598392 ),
 .UNSPECIFIED. ) ;
#34178 = CARTESIAN_POINT ( 'NONE',  ( -5.670847180967843570, -1.750000000000023315, 81.84341382277507648 ) ) ;
#34179 = ORIENTED_EDGE ( 'NONE', *, *, #43986, .T. ) ;
#34180 = DIRECTION ( 'NONE',  ( -1.000000000000000000, -0.000000000000000000, -0.000000000000000000 ) ) ;
#34181 = CARTESIAN_POINT ( 'NONE',  ( 35.51846793572394034, -35.99772139009119343, 7.906207997025717304 ) ) ;
#34182 = LINE ( 'NONE', #46933, #28741 ) ;
#34183 = CARTESIAN_POINT ( 'NONE',  ( -4.945973446814903696, 2.143131898507912917E-16, 165.0000000000000000 ) ) ;
#34184 = EDGE_CURVE ( 'NONE', #5777, #16313, #43395, .T. ) ;
#34185 = ORIENTED_EDGE ( 'NONE', *, *, #29770, .T. ) ;
#34186 = VERTEX_POINT ( 'NONE', #4413 ) ;
#34187 = CARTESIAN_POINT ( 'NONE',  ( 1.011271242968683648, 0.7347315653655930312, 10.00000000000000000 ) ) ;
#34188 = CARTESIAN_POINT ( 'NONE',  ( 33.89193117067293315, -33.89193117067293315, 910.0000000000000000 ) ) ;
#34189 = ORIENTED_EDGE ( 'NONE', *, *, #12176, .T. ) ;
#34190 = AXIS2_PLACEMENT_3D ( 'NONE', #24384, #16664, #44349 ) ;
#34191 = VERTEX_POINT ( 'NONE', #42886 ) ;
#34192 = EDGE_CURVE ( 'NONE', #45821, #14015, #7753, .T. ) ;
#34193 = CARTESIAN_POINT ( 'NONE',  ( 0.000000000000000000, 0.000000000000000000, 0.000000000000000000 ) ) ;
#34194 = EDGE_CURVE ( 'NONE', #43155, #2713, #3900, .T. ) ;
#34195 = DIRECTION ( 'NONE',  ( 0.000000000000000000, 0.000000000000000000, 1.000000000000000000 ) ) ;
#34196 = CARTESIAN_POINT ( 'NONE',  ( 0.000000000000000000, 0.000000000000000000, 900.0000000000000000 ) ) ;
#34197 = CARTESIAN_POINT ( 'NONE',  ( 0.000000000000000000, -166.9999999999999432, -344.0000000000001705 ) ) ;
#34198 = CARTESIAN_POINT ( 'NONE',  ( 358.3431457505076310, -165.0000000000001137, 339.9999999999998863 ) ) ;
#34199 = DIRECTION ( 'NONE',  ( -2.220446049250312588E-16, -0.7071067811865475727, -0.7071067811865474617 ) ) ;
#34200 = EDGE_LOOP ( 'NONE', ( #33887, #28475, #37891, #24433 ) ) ;
#34201 = EDGE_CURVE ( 'NONE', #7115, #43423, #12603, .T. ) ;
#34202 = CARTESIAN_POINT ( 'NONE',  ( -165.6708471809677974, 1.750000000000009548, 1.843413822775065825 ) ) ;
#34203 = CARTESIAN_POINT ( 'NONE',  ( 33.89193117067290473, -21.24469349090191983, 910.0000000000000000 ) ) ;
#34204 = LINE ( 'NONE', #49778, #6943 ) ;
#34206 = EDGE_LOOP ( 'NONE', ( #13007, #13707, #1583, #17427, #19065, #15028, #15379, #12257 ) ) ;
#34205 = VECTOR ( 'NONE', #10190, 1000.000000000000000 ) ;
#34207 = CARTESIAN_POINT ( 'NONE',  ( 154.1026953830863420, 103.9380105690400597, -17.65743994998277699 ) ) ;
#34208 = ORIENTED_EDGE ( 'NONE', *, *, #39163, .F. ) ;
#34209 = CARTESIAN_POINT ( 'NONE',  ( 113.3040265531850537, -1.749999999999996891, 160.8182875569279702 ) ) ;
#34210 = DIRECTION ( 'NONE',  ( 0.000000000000000000, 0.000000000000000000, 1.000000000000000000 ) ) ;
#34211 = CARTESIAN_POINT ( 'NONE',  ( -210.0000000000000568, 0.000000000000000000, 120.8182875569279702 ) ) ;
#34212 = ORIENTED_EDGE ( 'NONE', *, *, #7513, .F. ) ;
#34213 = DIRECTION ( 'NONE',  ( -0.000000000000000000, -0.000000000000000000, -1.000000000000000000 ) ) ;
#34214 = ORIENTED_EDGE ( 'NONE', *, *, #48365, .F. ) ;
#34215 = DIRECTION ( 'NONE',  ( -0.000000000000000000, -0.000000000000000000, -1.000000000000000000 ) ) ;
#34216 =( BOUNDED_CURVE ( )  B_SPLINE_CURVE ( 3, ( #6906, #26146, #37717, #49705 ),
 .UNSPECIFIED., .F., .F. ) 
 B_SPLINE_CURVE_WITH_KNOTS ( ( 4, 4 ),
 ( 0.000000000000000000, 1.570796326794896558 ),
 .UNSPECIFIED. ) 
 CURVE ( )  GEOMETRIC_REPRESENTATION_ITEM ( )  RATIONAL_B_SPLINE_CURVE ( ( 1.000000000000000000, 0.8047378541243649375, 0.8047378541243649375, 1.000000000000000000 ) ) 
 REPRESENTATION_ITEM ( '' )  );
#34217 = CYLINDRICAL_SURFACE ( 'NONE', #17993, 1.750000000000001554 ) ;
#34218 = FACE_OUTER_BOUND ( 'NONE', #11726, .T. ) ;
#34219 = ORIENTED_EDGE ( 'NONE', *, *, #4477, .F. ) ;
#34220 = ORIENTED_EDGE ( 'NONE', *, *, #49342, .F. ) ;
#34221 = CARTESIAN_POINT ( 'NONE',  ( 181.0000000000000000, -9.999999999999953815, -350.0000000000001705 ) ) ;
#34222 = DIRECTION ( 'NONE',  ( 0.000000000000000000, 0.9749645535258953943, -0.2223603367690637489 ) ) ;
#34223 = EDGE_CURVE ( 'NONE', #42678, #50118, #36235, .T. ) ;
#34224 = ORIENTED_EDGE ( 'NONE', *, *, #16854, .T. ) ;
#34225 = ORIENTED_EDGE ( 'NONE', *, *, #37911, .T. ) ;
#34226 = DIRECTION ( 'NONE',  ( -0.000000000000000000, -1.000000000000000000, -0.000000000000000000 ) ) ;
#34227 = CYLINDRICAL_SURFACE ( 'NONE', #10353, 0.5000000000000004441 ) ;
#34228 = CARTESIAN_POINT ( 'NONE',  ( -164.9459734468149463, 2.143131898507880377E-16, -157.4317124430720582 ) ) ;
#34229 = EDGE_LOOP ( 'NONE', ( #44412, #42235, #16928, #47293 ) ) ;
#34230 = PLANE ( 'NONE',  #49686 ) ;
#34231 = ORIENTED_EDGE ( 'NONE', *, *, #32215, .F. ) ;
#34232 = CYLINDRICAL_SURFACE ( 'NONE', #30798, 0.4999999999999997224 ) ;
#34233 = DIRECTION ( 'NONE',  ( -0.000000000000000000, -1.000000000000000000, -0.000000000000000000 ) ) ;
#34234 = EDGE_LOOP ( 'NONE', ( #6177, #33481, #15159, #23024, #41385, #17089 ) ) ;
#34235 = AXIS2_PLACEMENT_3D ( 'NONE', #11212, #38928, #26850 ) ;
#34236 = ORIENTED_EDGE ( 'NONE', *, *, #39743, .T. ) ;
#34237 = ORIENTED_EDGE ( 'NONE', *, *, #24464, .T. ) ;
#34238 = CARTESIAN_POINT ( 'NONE',  ( 341.6568542494924259, 185.0000000000000284, 359.9999999999998295 ) ) ;
#34239 = DIRECTION ( 'NONE',  ( -1.586032892321652236E-16, -1.000000000000000000, -6.853681917100419162E-49 ) ) ;
#34240 = ORIENTED_EDGE ( 'NONE', *, *, #42607, .F. ) ;
#34241 = ORIENTED_EDGE ( 'NONE', *, *, #1519, .T. ) ;
#34242 = DIRECTION ( 'NONE',  ( 0.000000000000000000, 0.000000000000000000, 1.000000000000000000 ) ) ;
#34243 = SURFACE_SIDE_STYLE ('',( #18816 ) ) ;
#34244 = VERTEX_POINT ( 'NONE', #40820 ) ;
#34245 = CARTESIAN_POINT ( 'NONE',  ( 0.3370904143228947158, 0.2449105217885311492, 10.00000000000000000 ) ) ;
#34246 = CARTESIAN_POINT ( 'NONE',  ( 115.0540265531850395, -1.025126265847081664, -37.43171244307203693 ) ) ;
#34247 = CARTESIAN_POINT ( 'NONE',  ( -1.011271242968693862, 0.7347315653655780432, 10.00000000000000000 ) ) ;
#34248 = DIRECTION ( 'NONE',  ( 1.000000000000000000, 0.000000000000000000, -0.000000000000000000 ) ) ;
#34249 = DIRECTION ( 'NONE',  ( 1.000000000000000000, 0.000000000000000000, 0.000000000000000000 ) ) ;
#34250 = ORIENTED_EDGE ( 'NONE', *, *, #41596, .T. ) ;
#34251 = EDGE_CURVE ( 'NONE', #17870, #47520, #22170, .T. ) ;
#34252 = CARTESIAN_POINT ( 'NONE',  ( 152.2789002873379900, -1.750000000000009548, -158.1565861772249377 ) ) ;
#34253 = AXIS2_PLACEMENT_3D ( 'NONE', #21935, #2674, #3168 ) ;
#34254 = DIRECTION ( 'NONE',  ( -1.000000000000000000, -0.000000000000000000, -0.000000000000000000 ) ) ;
#34255 = B_SPLINE_SURFACE_WITH_KNOTS ( 'NONE', 3, 3, ( 
 ( #31307, #47647, #3570, #4601 ),
 ( #11544, #23589, #42820, #35674 ),
 ( #19215, #20244, #35159, #50484 ),
 ( #27947, #15391, #7693, #1 ) ),
 .UNSPECIFIED., .F., .F., .F.,
 ( 4, 4 ),
 ( 4, 4 ),
 ( 0.000000000000000000, 1.000000000000000000 ),
 ( 0.000000000000000000, 1.000000000000000000 ),
 .UNSPECIFIED. ) ;
#34256 = CARTESIAN_POINT ( 'NONE',  ( 71.55402655318505367, 0.000000000000000000, -117.4317124430720156 ) ) ;
#34257 = DIRECTION ( 'NONE',  ( 1.000000000000000000, 0.000000000000000000, 0.000000000000000000 ) ) ;
#34258 = CARTESIAN_POINT ( 'NONE',  ( 339.9999999999999432, 181.0000000000000568, -356.0000000000002274 ) ) ;
#34259 = CARTESIAN_POINT ( 'NONE',  ( -0.5111101921243752511, -1.175566515482119989, 9.957892297621015132 ) ) ;
#34260 = CARTESIAN_POINT ( 'NONE',  ( 154.1026953830863420, 103.9380105690400597, 22.84256005001721945 ) ) ;
#34261 = CARTESIAN_POINT ( 'NONE',  ( -556.8973046169135159, -62.56198943095993315, -64.63743994998280584 ) ) ;
#34262 = VERTEX_POINT ( 'NONE', #44148 ) ;
#34263 =( BOUNDED_CURVE ( )  B_SPLINE_CURVE ( 3, ( #20534, #47943, #31849, #12835 ),
 .UNSPECIFIED., .F., .F. ) 
 B_SPLINE_CURVE_WITH_KNOTS ( ( 4, 4 ),
 ( 4.712388980384689674, 6.283185307179586232 ),
 .UNSPECIFIED. ) 
 CURVE ( )  GEOMETRIC_REPRESENTATION_ITEM ( )  RATIONAL_B_SPLINE_CURVE ( ( 1.000000000000000000, 0.8047378541243649375, 0.8047378541243649375, 1.000000000000000000 ) ) 
 REPRESENTATION_ITEM ( '' )  );
#34264 = VECTOR ( 'NONE', #37304, 1000.000000000000000 ) ;
#34265 = CARTESIAN_POINT ( 'NONE',  ( 0.000000000000000000, 0.000000000000000000, 0.000000000000000000 ) ) ;
#34266 = CARTESIAN_POINT ( 'NONE',  ( 165.0000000000000000, -174.9999999999999716, -99.00000000000014211 ) ) ;
#34267 = CARTESIAN_POINT ( 'NONE',  ( 33.16902712922644270, -37.70469005304286725, 1.847720168420772691 ) ) ;
#34268 = DIRECTION ( 'NONE',  ( 0.000000000000000000, 0.000000000000000000, 1.000000000000000000 ) ) ;
#34269 =( BOUNDED_CURVE ( )  B_SPLINE_CURVE ( 3, ( #29894, #45759, #49594, #10897 ),
 .UNSPECIFIED., .F., .F. ) 
 B_SPLINE_CURVE_WITH_KNOTS ( ( 4, 4 ),
 ( 0.000000000000000000, 1.570796326794896780 ),
 .UNSPECIFIED. ) 
 CURVE ( )  GEOMETRIC_REPRESENTATION_ITEM ( )  RATIONAL_B_SPLINE_CURVE ( ( 1.000000000000000000, 0.8047378541243649375, 0.8047378541243649375, 1.000000000000000000 ) ) 
 REPRESENTATION_ITEM ( '' )  );
#34270 = ORIENTED_EDGE ( 'NONE', *, *, #12062, .F. ) ;
#34271 = ADVANCED_FACE ( 'NONE', ( #32629 ), #5157, .T. ) ;
#34272 = ORIENTED_EDGE ( 'NONE', *, *, #3111, .F. ) ;
#34273 = DIRECTION ( 'NONE',  ( 0.000000000000000000, 0.000000000000000000, -1.000000000000000000 ) ) ;
#34274 = CARTESIAN_POINT ( 'NONE',  ( -1.158497635116737312, 16.61944452314319420, -3.546734833711462365 ) ) ;
#34275 = EDGE_CURVE ( 'NONE', #40485, #24426, #5665, .T. ) ;
#34276 = ORIENTED_EDGE ( 'NONE', *, *, #34251, .F. ) ;
#34277 = CARTESIAN_POINT ( 'NONE',  ( 153.2026953830863647, 103.1142457376053727, -17.29493270523947501 ) ) ;
#34278 = DIRECTION ( 'NONE',  ( 0.000000000000000000, 0.000000000000000000, -1.000000000000000000 ) ) ;
#34279 = DIRECTION ( 'NONE',  ( -0.000000000000000000, -0.000000000000000000, -1.000000000000000000 ) ) ;
#34280 = ORIENTED_EDGE ( 'NONE', *, *, #7349, .F. ) ;
#34281 = ORIENTED_EDGE ( 'NONE', *, *, #6200, .F. ) ;
#34282 = ORIENTED_EDGE ( 'NONE', *, *, #48841, .T. ) ;
#34283 = DIRECTION ( 'NONE',  ( 1.132880637372608740E-16, 4.718402560806925739E-50, 1.000000000000000000 ) ) ;
#34284 = DIRECTION ( 'NONE',  ( -1.000000000000000000, 0.000000000000000000, 0.000000000000000000 ) ) ;
#34285 = CARTESIAN_POINT ( 'NONE',  ( -6.695973446814940111, 0.000000000000000000, 165.0000000000000000 ) ) ;
#34286 = ORIENTED_EDGE ( 'NONE', *, *, #27801, .T. ) ;
#34287 = FACE_OUTER_BOUND ( 'NONE', #50217, .T. ) ;
#34288 = FACE_OUTER_BOUND ( 'NONE', #24529, .T. ) ;
#34289 = CARTESIAN_POINT ( 'NONE',  ( -14.99999999999845812, 17.00000000000000000, 35.00000000000000000 ) ) ;
#34290 = VERTEX_POINT ( 'NONE', #9514 ) ;
#34291 = VERTEX_POINT ( 'NONE', #24929 ) ;
#34292 = CARTESIAN_POINT ( 'NONE',  ( 210.0000000000000568, 0.000000000000000000, -39.18171244307202983 ) ) ;
#34293 = DIRECTION ( 'NONE',  ( -1.000000000000000000, -0.000000000000000000, -0.000000000000000000 ) ) ;
#34294 = EDGE_LOOP ( 'NONE', ( #49975, #2464, #37107, #10735, #32924, #48021, #14900, #10480, #39263, #39128, #31876, #14720, #40849, #45442 ) ) ;
#34295 = ORIENTED_EDGE ( 'NONE', *, *, #176, .T. ) ;
#34296 = DIRECTION ( 'NONE',  ( -1.000000000000000000, 0.000000000000000000, -0.000000000000000000 ) ) ;
#34297 = EDGE_CURVE ( 'NONE', #45274, #29268, #37297, .T. ) ;
#34298 = CARTESIAN_POINT ( 'NONE',  ( -0.4402948852767746279, 2.015117899693936732, 9.894754715216722118 ) ) ;
#34299 = CARTESIAN_POINT ( 'NONE',  ( 33.30402655318503946, -1.750000000000010214, -39.18171244307202983 ) ) ;
#34300 = AXIS2_PLACEMENT_3D ( 'NONE', #48334, #9130, #5528 ) ;
#34301 = ADVANCED_FACE ( 'NONE', ( #21318 ), #20564, .T. ) ;
#34302 = CARTESIAN_POINT ( 'NONE',  ( 6.174150299305392053, -50.00000000000000711, 8.807470649214879543 ) ) ;
#34303 = ORIENTED_EDGE ( 'NONE', *, *, #5807, .T. ) ;
#34304 = DIRECTION ( 'NONE',  ( -1.000000000000000000, 0.000000000000000000, -2.958228394578794270E-31 ) ) ;
#34305 = ADVANCED_FACE ( 'NONE', ( #1331 ), #1826, .T. ) ;
#34306 = CARTESIAN_POINT ( 'NONE',  ( 1.011271242968694084, -0.7347315653655782652, 3.333333333333333481 ) ) ;
#34307 = CARTESIAN_POINT ( 'NONE',  ( 85.00000000000123634, 17.00000000000000000, 30.00000000000000000 ) ) ;
#34308 = CARTESIAN_POINT ( 'NONE',  ( -69.99999999999879208, 16.00000000000000000, 30.00000000000000000 ) ) ;
#34309 = CLOSED_SHELL ( 'NONE', ( #43204, #44086, #17489, #15473, #40081, #12807, #29556, #44704, #888, #7372, #25044, #45928, #45876, #36274, #212, #16926, #27861, #47758 ) ) ;
#34310 = EDGE_CURVE ( 'NONE', #39650, #31856, #20809, .T. ) ;
#34311 = DIRECTION ( 'NONE',  ( -1.000000000000000000, -0.000000000000000000, -0.000000000000000000 ) ) ;
#34312 = EDGE_CURVE ( 'NONE', #16814, #34456, #1580, .T. ) ;
#34313 = CARTESIAN_POINT ( 'NONE',  ( -125.6708471809678542, 1.749999999999996891, -120.2068387089191219 ) ) ;
#34314 = ORIENTED_EDGE ( 'NONE', *, *, #23328, .F. ) ;
#34315 = CARTESIAN_POINT ( 'NONE',  ( 10.70590866674922204, -12.76446523155706814, -3.546734833711462365 ) ) ;
#34316 = DIRECTION ( 'NONE',  ( 1.000000000000000000, 0.000000000000000000, 0.000000000000000000 ) ) ;
#34317 = CARTESIAN_POINT ( 'NONE',  ( -4.945973446814917018, -1.025126265847097207, 39.06828755692796307 ) ) ;
#34318 = ORIENTED_EDGE ( 'NONE', *, *, #15333, .F. ) ;
#34319 = LINE ( 'NONE', #14812, #24006 ) ;
#34320 = CARTESIAN_POINT ( 'NONE',  ( -164.9459734468149463, 2.143131898507880377E-16, -0.9317124430720247208 ) ) ;
#34321 = ORIENTED_EDGE ( 'NONE', *, *, #14208, .T. ) ;
#34322 = CARTESIAN_POINT ( 'NONE',  ( -114.9999999999978542, 16.00000000000000000, 115.0000000000000142 ) ) ;
#34323 = CARTESIAN_POINT ( 'NONE',  ( -48.44597344681495343, 0.000000000000000000, 122.5682875569279702 ) ) ;
#34324 = DIRECTION ( 'NONE',  ( -1.000000000000000000, 0.000000000000000000, -2.958228394578794270E-31 ) ) ;
#34325 = DIRECTION ( 'NONE',  ( 0.000000000000000000, 0.000000000000000000, -1.000000000000000000 ) ) ;
#34326 = ORIENTED_EDGE ( 'NONE', *, *, #14646, .F. ) ;
#34327 = CARTESIAN_POINT ( 'NONE',  ( 9.999999999999996447, -34.54492135858216528, 0.000000000000000000 ) ) ;
#34328 = EDGE_CURVE ( 'NONE', #49797, #15554, #39532, .T. ) ;
#34330 = ORIENTED_EDGE ( 'NONE', *, *, #25301, .T. ) ;
#34329 = EDGE_CURVE ( 'NONE', #35332, #15646, #12969, .T. ) ;
#34331 = ORIENTED_EDGE ( 'NONE', *, *, #49690, .F. ) ;
#34332 = CARTESIAN_POINT ( 'NONE',  ( -3.345242017215803276, 2.159124855890678596, -2.642742795433417058E-16 ) ) ;
#34333 = VECTOR ( 'NONE', #35588, 1000.000000000000000 ) ;
#34334 = EDGE_CURVE ( 'NONE', #13192, #6245, #41152, .T. ) ;
#34335 = ADVANCED_FACE ( 'NONE', ( #12864 ), #32888, .F. ) ;
#34336 = VECTOR ( 'NONE', #19736, 1000.000000000000000 ) ;
#34337 = ORIENTED_EDGE ( 'NONE', *, *, #14219, .F. ) ;
#34338 = DIRECTION ( 'NONE',  ( 0.000000000000000000, 0.000000000000000000, 1.000000000000000000 ) ) ;
#34339 = CARTESIAN_POINT ( 'NONE',  ( 210.0000000000000568, 0.000000000000000000, 0.8182875569279768335 ) ) ;
#34340 = CARTESIAN_POINT ( 'NONE',  ( 135.0000000000000000, 17.00000000000000000, -90.00000000000000000 ) ) ;
#34341 = VECTOR ( 'NONE', #27745, 1000.000000000000000 ) ;
#34342 = CIRCLE ( 'NONE', #29428, 2.000000000000001776 ) ;
#34343 = EDGE_CURVE ( 'NONE', #42077, #30382, #48471, .T. ) ;
#34344 = LINE ( 'NONE', #3982, #37921 ) ;
#34345 = EDGE_CURVE ( 'NONE', #24452, #19705, #32034, .T. ) ;
#34346 = LINE ( 'NONE', #7143, #18555 ) ;
#34347 = VECTOR ( 'NONE', #33367, 1000.000000000000000 ) ;
#34348 = ORIENTED_EDGE ( 'NONE', *, *, #482, .T. ) ;
#34349 = CARTESIAN_POINT ( 'NONE',  ( -166.6959734468149463, 0.000000000000000000, 165.0000000000000000 ) ) ;
#34350 = DIRECTION ( 'NONE',  ( 1.000000000000000000, 0.000000000000000000, 0.000000000000000000 ) ) ;
#34351 = CARTESIAN_POINT ( 'NONE',  ( -34.08406891383351933, 15.63733501198486309, -8.192531242611266862 ) ) ;
#34352 = LINE ( 'NONE', #14839, #12776 ) ;
#34353 = VECTOR ( 'NONE', #43482, 1000.000000000000000 ) ;
#34354 = ORIENTED_EDGE ( 'NONE', *, *, #24265, .T. ) ;
#34355 = CARTESIAN_POINT ( 'NONE',  ( -64.99999999999940314, 16.00000000000000000, -54.99999999999999289 ) ) ;
#34356 = CARTESIAN_POINT ( 'NONE',  ( 1.011271242968688311, -0.7347315653655854817, 9.972675548442463622 ) ) ;
#34357 = ORIENTED_EDGE ( 'NONE', *, *, #28495, .F. ) ;
#34358 = ORIENTED_EDGE ( 'NONE', *, *, #26014, .F. ) ;
#34359 = ORIENTED_EDGE ( 'NONE', *, *, #47236, .T. ) ;
#34360 = CARTESIAN_POINT ( 'NONE',  ( -5.670847180967843570, 1.750000000000022871, -158.1565861772249093 ) ) ;
#34361 = CARTESIAN_POINT ( 'NONE',  ( 22.69295089195473736, 45.31600496604706052, 7.455576670931136185 ) ) ;
#34362 = PRODUCT_DEFINITION_SHAPE ( 'NONE', 'NONE',  #17451 ) ;
#34363 = ORIENTED_EDGE ( 'NONE', *, *, #18779, .F. ) ;
#34364 = EDGE_CURVE ( 'NONE', #18141, #46782, #9859, .T. ) ;
#34365 = CARTESIAN_POINT ( 'NONE',  ( -207.7210997126620384, 1.750000000000009548, 81.84341382277507648 ) ) ;
#34366 = CARTESIAN_POINT ( 'NONE',  ( 155.0540265531850537, 2.143131898507880377E-16, -0.9317124430720247208 ) ) ;
#34367 = EDGE_CURVE ( 'NONE', #28808, #19177, #13852, .T. ) ;
#34368 = CARTESIAN_POINT ( 'NONE',  ( 85.00000000000213163, 17.00000000000000000, 95.00000000000000000 ) ) ;
#34369 = EDGE_CURVE ( 'NONE', #44745, #15868, #10280, .T. ) ;
#34370 = DIRECTION ( 'NONE',  ( -7.793956916774525800E-48, 0.000000000000000000, -1.000000000000000000 ) ) ;
#34371 = LINE ( 'NONE', #38728, #35778 ) ;
#34372 = LINE ( 'NONE', #11011, #277 ) ;
#34373 = ORIENTED_EDGE ( 'NONE', *, *, #12666, .F. ) ;
#34374 = AXIS2_PLACEMENT_3D ( 'NONE', #50291, #50545, #19289 ) ;
#34375 = DIRECTION ( 'NONE',  ( 0.000000000000000000, 1.580451535867971417E-48, -1.000000000000000000 ) ) ;
#34376 = DIRECTION ( 'NONE',  ( -1.000000000000000000, -0.000000000000000000, -0.000000000000000000 ) ) ;
#34377 = VECTOR ( 'NONE', #12173, 1000.000000000000000 ) ;
#34378 = CARTESIAN_POINT ( 'NONE',  ( 111.5540265531850679, 0.000000000000000000, 42.56828755692795596 ) ) ;
#34379 = CARTESIAN_POINT ( 'NONE',  ( 33.30402655318503946, 0.000000000000000000, 165.0000000000000000 ) ) ;
#34380 = EDGE_LOOP ( 'NONE', ( #3155, #16481, #13743, #13199, #406, #34126 ) ) ;
#34381 = AXIS2_PLACEMENT_3D ( 'NONE', #47620, #28173, #8678 ) ;
#34382 = CARTESIAN_POINT ( 'NONE',  ( -10.69268279052439574, -12.77266927778454964, -2.870787844569587133 ) ) ;
#34383 = EDGE_CURVE ( 'NONE', #14684, #45714, #8058, .T. ) ;
#34384 = VECTOR ( 'NONE', #14295, 1000.000000000000000 ) ;
#34385 = FACE_OUTER_BOUND ( 'NONE', #43034, .T. ) ;
#34386 = CARTESIAN_POINT ( 'NONE',  ( -1.448406091252275818, 0.9360325558308429938, 9.928159647716187308 ) ) ;
#34387 = DIRECTION ( 'NONE',  ( 1.000000000000000000, 0.000000000000000000, -0.000000000000000000 ) ) ;
#34388 = CARTESIAN_POINT ( 'NONE',  ( 130.0000000000021032, 17.00000000000000000, 95.00000000000000000 ) ) ;
#34389 = AXIS2_PLACEMENT_3D ( 'NONE', #39453, #39705, #19427 ) ;
#34390 = ORIENTED_EDGE ( 'NONE', *, *, #34329, .F. ) ;
#34391 = CARTESIAN_POINT ( 'NONE',  ( -206.6959734468149463, -1.750000000000009992, 0.8182875569279768335 ) ) ;
#34392 = EDGE_LOOP ( 'NONE', ( #3984, #321, #24312, #654 ) ) ;
#34393 = CARTESIAN_POINT ( 'NONE',  ( 75.05402655318509630, 2.143131898507880377E-16, -40.93171244307205825 ) ) ;
#34394 = EDGE_CURVE ( 'NONE', #38096, #31646, #41795, .T. ) ;
#34395 = VERTEX_POINT ( 'NONE', #29523 ) ;
#34396 = FACE_OUTER_BOUND ( 'NONE', #3607, .T. ) ;
#34397 = CARTESIAN_POINT ( 'NONE',  ( 75.05402655318509630, 2.143131898507880377E-16, -37.43171244307200141 ) ) ;
#34398 = ORIENTED_EDGE ( 'NONE', *, *, #27365, .F. ) ;
#34399 = DIRECTION ( 'NONE',  ( -0.000000000000000000, -0.000000000000000000, -1.000000000000000000 ) ) ;
#34400 = VERTEX_POINT ( 'NONE', #26424 ) ;
#34401 = EDGE_CURVE ( 'NONE', #2527, #14054, #41326, .T. ) ;
#34402 = ADVANCED_FACE ( 'NONE', ( #34396 ), #22323, .F. ) ;
#34403 = EDGE_LOOP ( 'NONE', ( #9016, #14129, #25192, #460, #42728 ) ) ;
#34404 = DIRECTION ( 'NONE',  ( 0.000000000000000000, 0.000000000000000000, 1.000000000000000000 ) ) ;
#34405 = ORIENTED_EDGE ( 'NONE', *, *, #33986, .T. ) ;
#34406 = DIRECTION ( 'NONE',  ( 1.000000000000000000, 0.000000000000000000, -1.586032892321652482E-16 ) ) ;
#34407 = PLANE ( 'NONE',  #18504 ) ;
#34408 = CARTESIAN_POINT ( 'NONE',  ( -7.721099712662037540, -1.750000000000023537, -80.20683870891910772 ) ) ;
#34409 = ORIENTED_EDGE ( 'NONE', *, *, #21983, .F. ) ;
#34410 = EDGE_CURVE ( 'NONE', #7540, #23937, #48964, .T. ) ;
#34411 = ORIENTED_EDGE ( 'NONE', *, *, #32200, .T. ) ;
#34412 = DIRECTION ( 'NONE',  ( 0.000000000000000000, 1.000000000000000000, 0.000000000000000000 ) ) ;
#34413 = EDGE_CURVE ( 'NONE', #1069, #9737, #38990, .T. ) ;
#34414 = CARTESIAN_POINT ( 'NONE',  ( 164.9999999999999716, 16.00000000000000000, 95.00000000000000000 ) ) ;
#34415 = AXIS2_PLACEMENT_3D ( 'NONE', #13292, #40761, #21253 ) ;
#34416 = EDGE_CURVE ( 'NONE', #18915, #8241, #17727, .T. ) ;
#34417 =( BOUNDED_CURVE ( )  B_SPLINE_CURVE ( 3, ( #38982, #46112, #6909, #26662 ),
 .UNSPECIFIED., .F., .F. ) 
 B_SPLINE_CURVE_WITH_KNOTS ( ( 4, 4 ),
 ( 4.712388980384689674, 6.283185307179586232 ),
 .UNSPECIFIED. ) 
 CURVE ( )  GEOMETRIC_REPRESENTATION_ITEM ( )  RATIONAL_B_SPLINE_CURVE ( ( 1.000000000000000000, 0.8047378541243649375, 0.8047378541243649375, 1.000000000000000000 ) ) 
 REPRESENTATION_ITEM ( '' )  );
#34418 = AXIS2_PLACEMENT_3D ( 'NONE', #20937, #1450, #28890 ) ;
#34419 = ORIENTED_EDGE ( 'NONE', *, *, #13078, .T. ) ;
#34420 = CARTESIAN_POINT ( 'NONE',  ( 350.0000000000001137, 165.0000000000000000, 359.9999999999997726 ) ) ;
#34421 = FACE_OUTER_BOUND ( 'NONE', #28051, .T. ) ;
#34422 = EDGE_LOOP ( 'NONE', ( #37411, #16708 ) ) ;
#34423 = CARTESIAN_POINT ( 'NONE',  ( 1.104213410210670876, 0.6509177773818231039, 9.976582533991679824 ) ) ;
#34424 = VECTOR ( 'NONE', #46104, 1000.000000000000000 ) ;
#34425 =( BOUNDED_CURVE ( )  B_SPLINE_CURVE ( 3, ( #10889, #26545, #11398, #7050 ),
 .UNSPECIFIED., .F., .F. ) 
 B_SPLINE_CURVE_WITH_KNOTS ( ( 4, 4 ),
 ( 4.712388980384689674, 6.283185307179586232 ),
 .UNSPECIFIED. ) 
 CURVE ( )  GEOMETRIC_REPRESENTATION_ITEM ( )  RATIONAL_B_SPLINE_CURVE ( ( 1.000000000000000000, 0.8047378541243649375, 0.8047378541243649375, 1.000000000000000000 ) ) 
 REPRESENTATION_ITEM ( '' )  );
#34426 = EDGE_CURVE ( 'NONE', #6173, #50118, #6178, .T. ) ;
#34427 = CARTESIAN_POINT ( 'NONE',  ( -168.4459734468149463, 0.000000000000000000, 79.06828755692797017 ) ) ;
#34428 = ORIENTED_EDGE ( 'NONE', *, *, #23054, .F. ) ;
#34429 = CARTESIAN_POINT ( 'NONE',  ( -32.57170742938676256, -18.58316106410400437, 7.697694107796192675 ) ) ;
#34430 = CARTESIAN_POINT ( 'NONE',  ( -126.6959734468149321, -1.749999999999997335, -79.18171244307201562 ) ) ;
#34431 = CARTESIAN_POINT ( 'NONE',  ( 30.00000000000062172, 16.00000000000000000, -30.00000000000000000 ) ) ;
#34432 = VECTOR ( 'NONE', #28532, 1000.000000000000000 ) ;
#34433 = DIRECTION ( 'NONE',  ( 0.000000000000000000, 1.000000000000000000, 0.000000000000000000 ) ) ;
#34434 = ORIENTED_EDGE ( 'NONE', *, *, #43166, .F. ) ;
#34435 = CARTESIAN_POINT ( 'NONE',  ( -7.749480817862350435, -14.85497772329513211, 9.403735324607438884 ) ) ;
#34436 = CARTESIAN_POINT ( 'NONE',  ( -13.59579750444763668, 10.60877755095910935, 8.727788335465566760 ) ) ;
#34437 =( BOUNDED_CURVE ( )  B_SPLINE_CURVE ( 3, ( #45565, #30451, #26603, #10945 ),
 .UNSPECIFIED., .F., .F. ) 
 B_SPLINE_CURVE_WITH_KNOTS ( ( 4, 4 ),
 ( 1.570796326794896558, 3.141592653589793116 ),
 .UNSPECIFIED. ) 
 CURVE ( )  GEOMETRIC_REPRESENTATION_ITEM ( )  RATIONAL_B_SPLINE_CURVE ( ( 1.000000000000000000, 0.8047378541243649375, 0.8047378541243649375, 1.000000000000000000 ) ) 
 REPRESENTATION_ITEM ( '' )  );
#34438 = LINE ( 'NONE', #38036, #49320 ) ;
#34439 = ORIENTED_EDGE ( 'NONE', *, *, #20329, .T. ) ;
#34440 = EDGE_LOOP ( 'NONE', ( #47692, #23367, #5056, #30353 ) ) ;
#34441 = CARTESIAN_POINT ( 'NONE',  ( 7.608425291889091113, -36.72004717559254772, 7.697694107796188234 ) ) ;
#34442 = PLANE ( 'NONE',  #6383 ) ;
#34443 = DIRECTION ( 'NONE',  ( 0.000000000000000000, 1.000000000000000000, 6.123233995736766036E-17 ) ) ;
#34444 = CARTESIAN_POINT ( 'NONE',  ( -5.000000000000000000, -165.1999999999999602, 359.7999999999997840 ) ) ;
#34445 = PLANE ( 'NONE',  #23307 ) ;
#34446 = DIRECTION ( 'NONE',  ( 0.000000000000000000, -0.000000000000000000, 1.000000000000000000 ) ) ;
#34447 = VERTEX_POINT ( 'NONE', #14377 ) ;
#34448 = CARTESIAN_POINT ( 'NONE',  ( -0.3862712429686729343, -1.188820645368946050, -10.00000000000000000 ) ) ;
#34449 = DIRECTION ( 'NONE',  ( 3.363195139050033768E-16, 0.7071067811865474617, 0.7071067811865475727 ) ) ;
#34450 = CARTESIAN_POINT ( 'NONE',  ( 181.0000000000000000, -9.999999999999953815, -340.0000000000001137 ) ) ;
#34451 = VECTOR ( 'NONE', #49115, 1000.000000000000000 ) ;
#34452 = EDGE_CURVE ( 'NONE', #36, #31581, #38262, .T. ) ;
#34453 = VECTOR ( 'NONE', #30865, 1000.000000000000000 ) ;
#34454 = ORIENTED_EDGE ( 'NONE', *, *, #34066, .T. ) ;
#34455 = CARTESIAN_POINT ( 'NONE',  ( 5.888214538810389698, 16.20866436362417673, 8.727788335465566760 ) ) ;
#34456 = VERTEX_POINT ( 'NONE', #45395 ) ;
#34457 = VECTOR ( 'NONE', #4064, 1000.000000000000000 ) ;
#34458 = CARTESIAN_POINT ( 'NONE',  ( 10.01251772323701594, 8.486842105263161073, -18.46084505325461578 ) ) ;
#34459 = DIRECTION ( 'NONE',  ( -0.7233555441435721711, -0.6904757466825004464, 0.000000000000000000 ) ) ;
#34460 = VECTOR ( 'NONE', #33359, 1000.000000000000000 ) ;
#34461 = VECTOR ( 'NONE', #27193, 1000.000000000000000 ) ;
#34462 = CARTESIAN_POINT ( 'NONE',  ( 210.0000000000000568, 0.000000000000000000, 0.8182875569279768335 ) ) ;
#34463 = ORIENTED_EDGE ( 'NONE', *, *, #6058, .F. ) ;
#34464 = EDGE_CURVE ( 'NONE', #16051, #27596, #25942, .T. ) ;
#34465 = EDGE_CURVE ( 'NONE', #2997, #21643, #6091, .T. ) ;
#34466 = VERTEX_POINT ( 'NONE', #10522 ) ;
#34467 = CARTESIAN_POINT ( 'NONE',  ( -164.9459734468149463, -1.025126265847088991, 2.568287556927986159 ) ) ;
#34468 = CARTESIAN_POINT ( 'NONE',  ( -9.999999999999998224, 8.486842105263161073, -25.00000000000000000 ) ) ;
#34469 = LINE ( 'NONE', #11356, #35727 ) ;
#34470 = ORIENTED_EDGE ( 'NONE', *, *, #49656, .F. ) ;
#34471 = EDGE_CURVE ( 'NONE', #21503, #29362, #16287, .T. ) ;
#34472 = VERTEX_POINT ( 'NONE', #45892 ) ;
#34473 = CARTESIAN_POINT ( 'NONE',  ( 344.0000000000000000, 175.0000000000000284, -108.0000000000002132 ) ) ;
#34474 = DIRECTION ( 'NONE',  ( -0.000000000000000000, -1.000000000000000000, -0.000000000000000000 ) ) ;
#34475 = EDGE_CURVE ( 'NONE', #33612, #19484, #14766, .T. ) ;
#34476 = EDGE_CURVE ( 'NONE', #34694, #39319, #23595, .T. ) ;
#34477 = ORIENTED_EDGE ( 'NONE', *, *, #49385, .F. ) ;
#34478 = VERTEX_POINT ( 'NONE', #23338 ) ;
#34479 = FACE_OUTER_BOUND ( 'NONE', #16248, .T. ) ;
#34480 = CARTESIAN_POINT ( 'NONE',  ( 210.0000000000000568, 2.143131898507881856E-16, -120.9317124430720582 ) ) ;
#34481 = CARTESIAN_POINT ( 'NONE',  ( 193.3040265531851105, 0.000000000000000000, 165.0000000000000000 ) ) ;
#34482 = ORIENTED_EDGE ( 'NONE', *, *, #50225, .T. ) ;
#34483 = DIRECTION ( 'NONE',  ( -1.000000000000000000, 0.000000000000000000, 0.000000000000000000 ) ) ;
#34484 = EDGE_CURVE ( 'NONE', #26083, #11650, #12056, .T. ) ;
#34485 = VERTEX_POINT ( 'NONE', #18973 ) ;
#34486 = CARTESIAN_POINT ( 'NONE',  ( -30.12518629743573584, -14.70074613238887551, 1.847720168420772691 ) ) ;
#34487 = CARTESIAN_POINT ( 'NONE',  ( -128.4459734468149463, -1.025126265847081886, -40.93171244307202272 ) ) ;
#34488 = VECTOR ( 'NONE', #41714, 1000.000000000000114 ) ;
#34489 = CARTESIAN_POINT ( 'NONE',  ( 4.672045878990125800, -50.00000000000000711, 1.847720168420772691 ) ) ;
#34490 = VECTOR ( 'NONE', #24242, 1000.000000000000000 ) ;
#34491 = ORIENTED_EDGE ( 'NONE', *, *, #1448, .T. ) ;
#34492 = EDGE_LOOP ( 'NONE', ( #2728, #29063, #30700, #4417 ) ) ;
#34493 = VERTEX_POINT ( 'NONE', #39010 ) ;
#34494 = FACE_OUTER_BOUND ( 'NONE', #8084, .T. ) ;
#34495 = ORIENTED_EDGE ( 'NONE', *, *, #6325, .T. ) ;
#34496 = DIRECTION ( 'NONE',  ( 0.000000000000000000, 0.000000000000000000, 1.000000000000000000 ) ) ;
#34497 = VECTOR ( 'NONE', #17218, 1000.000000000000000 ) ;
#34498 = VERTEX_POINT ( 'NONE', #11550 ) ;
#34499 = FACE_OUTER_BOUND ( 'NONE', #1936, .T. ) ;
#34500 = ORIENTED_EDGE ( 'NONE', *, *, #23478, .F. ) ;
#34501 = CARTESIAN_POINT ( 'NONE',  ( -1.011271242968683426, -0.7347315653655928092, 10.00000000000000000 ) ) ;
#34502 = DIRECTION ( 'NONE',  ( 0.000000000000000000, -2.537652627714643577E-15, -1.000000000000000000 ) ) ;
#34503 = DIRECTION ( 'NONE',  ( 1.000000000000000000, 0.000000000000000000, 0.000000000000000000 ) ) ;
#34504 = LINE ( 'NONE', #2676, #17231 ) ;
#34505 = CARTESIAN_POINT ( 'NONE',  ( -164.9459734468149463, 2.143131898507880377E-16, -120.9317124430720156 ) ) ;
#34506 = ORIENTED_EDGE ( 'NONE', *, *, #40715, .T. ) ;
#34507 = CARTESIAN_POINT ( 'NONE',  ( -27.73884755486766096, 25.23502201956265978, 7.697694107796191787 ) ) ;
#34508 = ADVANCED_FACE ( 'NONE', ( #43089 ), #30800, .T. ) ;
#34509 = CARTESIAN_POINT ( 'NONE',  ( 73.30402655318508209, -1.750000000000010214, -39.18171244307202983 ) ) ;
#34510 = CARTESIAN_POINT ( 'NONE',  ( 344.0000000000000000, -164.9999999999999432, 339.9999999999998295 ) ) ;
#34511 = CARTESIAN_POINT ( 'NONE',  ( 0.3862712429686810944, 1.188820645368943607, -10.00000000000000000 ) ) ;
#34512 = ADVANCED_FACE ( 'NONE', ( #27199 ), #27701, .F. ) ;
#34513 = B_SPLINE_CURVE_WITH_KNOTS ( 'NONE', 3,
 ( #22926, #10616, #7280, #41924 ),
 .UNSPECIFIED., .F., .F.,
 ( 4, 4 ),
 ( 0.000000000000000000, 0.001246897409371951551 ),
 .UNSPECIFIED. ) ;
#34514 = CARTESIAN_POINT ( 'NONE',  ( -5.647304616913629616, -290.4457172416107937, 144.9816133044550668 ) ) ;
#34515 =( BOUNDED_CURVE ( )  B_SPLINE_CURVE ( 3, ( #9791, #25456, #41104, #5947 ),
 .UNSPECIFIED., .F., .F. ) 
 B_SPLINE_CURVE_WITH_KNOTS ( ( 4, 4 ),
 ( 4.712388980384689674, 6.283185307179586232 ),
 .UNSPECIFIED. ) 
 CURVE ( )  GEOMETRIC_REPRESENTATION_ITEM ( )  RATIONAL_B_SPLINE_CURVE ( ( 1.000000000000000000, 0.8047378541243649375, 0.8047378541243649375, 1.000000000000000000 ) ) 
 REPRESENTATION_ITEM ( '' )  );
#34516 = CARTESIAN_POINT ( 'NONE',  ( 193.3040265531851105, -1.750000000000010658, 80.81828755692798438 ) ) ;
#34517 = B_SPLINE_CURVE_WITH_KNOTS ( 'NONE', 3,
 ( #15073, #34085, #38438, #18405 ),
 .UNSPECIFIED., .F., .F.,
 ( 4, 4 ),
 ( 0.0006664118838822479917, 0.001081796195657045356 ),
 .UNSPECIFIED. ) ;
#34518 = LINE ( 'NONE', #18330, #18823 ) ;
#34519 = FACE_OUTER_BOUND ( 'NONE', #17592, .T. ) ;
#34520 = AXIS2_PLACEMENT_3D ( 'NONE', #8307, #610, #360 ) ;
#34521 = ORIENTED_EDGE ( 'NONE', *, *, #17552, .T. ) ;
#34522 = CARTESIAN_POINT ( 'NONE',  ( 12.15085308559846844, -11.68662139125803989, 2.590526750877053086 ) ) ;
#34523 = CARTESIAN_POINT ( 'NONE',  ( -22.69295089195507487, -45.31600496604688999, 7.455576670931136185 ) ) ;
#34524 = CARTESIAN_POINT ( 'NONE',  ( 35.00000000000028422, 17.00000000000000000, -84.99999999999998579 ) ) ;
#34525 = VECTOR ( 'NONE', #37423, 1000.000000000000000 ) ;
#34526 = VERTEX_POINT ( 'NONE', #22830 ) ;
#34527 = CIRCLE ( 'NONE', #20566, 10.00000000000000000 ) ;
#34528 = ORIENTED_EDGE ( 'NONE', *, *, #27717, .T. ) ;
#34529 = CARTESIAN_POINT ( 'NONE',  ( -6.174150299305392053, 50.00000000000000711, 8.807470649214879543 ) ) ;
#34530 = CARTESIAN_POINT ( 'NONE',  ( -0.1425549192113998442, 1.238581250503548059, 9.981352469109934233 ) ) ;
#34531 = ORIENTED_EDGE ( 'NONE', *, *, #49343, .T. ) ;
#34532 = VERTEX_POINT ( 'NONE', #35168 ) ;
#34533 = DIRECTION ( 'NONE',  ( 0.000000000000000000, 0.000000000000000000, 1.000000000000000000 ) ) ;
#34534 = DIRECTION ( 'NONE',  ( -0.000000000000000000, -1.000000000000000000, -0.000000000000000000 ) ) ;
#34535 = CARTESIAN_POINT ( 'NONE',  ( 195.0540265531851105, -1.025126265847089213, -37.43171244307202272 ) ) ;
#34536 = VERTEX_POINT ( 'NONE', #16158 ) ;
#34537 = ORIENTED_EDGE ( 'NONE', *, *, #25525, .T. ) ;
#34538 = EDGE_CURVE ( 'NONE', #32124, #25314, #15643, .T. ) ;
#34539 = VERTEX_POINT ( 'NONE', #39515 ) ;
#34540 = CARTESIAN_POINT ( 'NONE',  ( 85.00000000000184741, 17.00000000000000000, 90.00000000000000000 ) ) ;
#34541 = CARTESIAN_POINT ( 'NONE',  ( 210.0000000000000568, 0.000000000000000000, 80.81828755692798438 ) ) ;
#34542 = LINE ( 'NONE', #16740, #48001 ) ;
#34543 = ORIENTED_EDGE ( 'NONE', *, *, #47410, .F. ) ;
#34544 = CARTESIAN_POINT ( 'NONE',  ( 350.0000000000000000, 183.0000000000000284, -356.0000000000002274 ) ) ;
#34545 = CARTESIAN_POINT ( 'NONE',  ( 74.32915281903215998, 1.750000000000009548, -40.20683870891912193 ) ) ;
#34546 = CARTESIAN_POINT ( 'NONE',  ( 35.00000000000186162, 16.00000000000000000, 90.00000000000000000 ) ) ;
#34547 = ORIENTED_EDGE ( 'NONE', *, *, #36560, .T. ) ;
#34548 = ORIENTED_EDGE ( 'NONE', *, *, #47578, .T. ) ;
#34549 = LINE ( 'NONE', #15041, #11525 ) ;
#34550 = CARTESIAN_POINT ( 'NONE',  ( -48.44597344681496054, 1.025126265847089213, 159.0682875569279418 ) ) ;
#34551 = VECTOR ( 'NONE', #11376, 1000.000000000000000 ) ;
#34552 = CARTESIAN_POINT ( 'NONE',  ( -177.4999999999999716, -112.5000000000000000, -10.00000000000000000 ) ) ;
#34553 = ORIENTED_EDGE ( 'NONE', *, *, #10513, .T. ) ;
#34554 = ORIENTED_EDGE ( 'NONE', *, *, #42443, .F. ) ;
#34555 = CARTESIAN_POINT ( 'NONE',  ( 7.884183412771427868, 42.26678417219198991, 893.0811050474360400 ) ) ;
#34556 = CYLINDRICAL_SURFACE ( 'NONE', #34620, 1.750000000000015543 ) ;
#34557 = CARTESIAN_POINT ( 'NONE',  ( 35.05402655318504657, 1.025126265847089879, -117.4317124430720156 ) ) ;
#34558 = DIRECTION ( 'NONE',  ( -1.000000000000000000, 0.000000000000000000, -0.000000000000000000 ) ) ;
#34559 = VECTOR ( 'NONE', #45506, 1000.000000000000000 ) ;
#34560 = DIRECTION ( 'NONE',  ( 0.000000000000000000, 0.000000000000000000, -1.000000000000000000 ) ) ;
#34561 = ORIENTED_EDGE ( 'NONE', *, *, #35958, .F. ) ;
#34562 = DIRECTION ( 'NONE',  ( 6.203854594147707562E-25, -2.067951531382569187E-25, 1.000000000000000000 ) ) ;
#34563 = LINE ( 'NONE', #19412, #11954 ) ;
#34564 = CARTESIAN_POINT ( 'NONE',  ( 359.9999999999999432, 177.9999999999999716, -353.0000000000000568 ) ) ;
#34565 = AXIS2_PLACEMENT_3D ( 'NONE', #34462, #27520, #11349 ) ;
#34566 = CARTESIAN_POINT ( 'NONE',  ( 359.9999999999999432, -181.0000000000001421, 356.0000000000000000 ) ) ;
#34567 = EDGE_CURVE ( 'NONE', #26389, #43828, #46651, .T. ) ;
#34568 = CARTESIAN_POINT ( 'NONE',  ( 30.87089393895375267, -12.69923079256617449, -9.367992836599954742 ) ) ;
#34569 =( BOUNDED_CURVE ( )  B_SPLINE_CURVE ( 3, ( #19447, #15606, #40730, #25080 ),
 .UNSPECIFIED., .F., .F. ) 
 B_SPLINE_CURVE_WITH_KNOTS ( ( 4, 4 ),
 ( 1.570796326794896558, 3.141592653589793116 ),
 .UNSPECIFIED. ) 
 CURVE ( )  GEOMETRIC_REPRESENTATION_ITEM ( )  RATIONAL_B_SPLINE_CURVE ( ( 1.000000000000000000, 0.8047378541243649375, 0.8047378541243649375, 1.000000000000000000 ) ) 
 REPRESENTATION_ITEM ( '' )  );
#34570 = CARTESIAN_POINT ( 'NONE',  ( 341.9999999999999432, -169.0000000000001705, 344.0000000000000568 ) ) ;
#34571 = ORIENTED_EDGE ( 'NONE', *, *, #31995, .F. ) ;
#34572 = FACE_OUTER_BOUND ( 'NONE', #48089, .T. ) ;
#34573 =( BOUNDED_CURVE ( )  B_SPLINE_CURVE ( 3, ( #38910, #27094, #47052, #44176 ),
 .UNSPECIFIED., .F., .F. ) 
 B_SPLINE_CURVE_WITH_KNOTS ( ( 4, 4 ),
 ( 2.784193070085688408E-13, 1.570796326794910991 ),
 .UNSPECIFIED. ) 
 CURVE ( )  GEOMETRIC_REPRESENTATION_ITEM ( )  RATIONAL_B_SPLINE_CURVE ( ( 1.000000000000000000, 0.8047378541244272210, 0.8047378541244272210, 1.000000000000000000 ) ) 
 REPRESENTATION_ITEM ( '' )  );
#34574 = FACE_OUTER_BOUND ( 'NONE', #25347, .T. ) ;
#34575 = CARTESIAN_POINT ( 'NONE',  ( 214.9999999999999432, -173.0000000000000000, 132.0000000000001137 ) ) ;
#34576 = ORIENTED_EDGE ( 'NONE', *, *, #23979, .T. ) ;
#34577 = DIRECTION ( 'NONE',  ( -0.000000000000000000, -0.000000000000000000, -1.000000000000000000 ) ) ;
#34578 = FACE_OUTER_BOUND ( 'NONE', #18000, .T. ) ;
#34579 = ORIENTED_EDGE ( 'NONE', *, *, #33729, .F. ) ;
#34580 = CARTESIAN_POINT ( 'NONE',  ( 135.0000000000021600, 17.00000000000000000, 95.00000000000000000 ) ) ;
#34581 = CARTESIAN_POINT ( 'NONE',  ( 4.641001526964561918, 50.00000000000000711, -8.016098858316205167 ) ) ;
#34582 = CARTESIAN_POINT ( 'NONE',  ( -127.7210997126620242, 1.749999999999996669, -78.15658617722492352 ) ) ;
#34583 = DIRECTION ( 'NONE',  ( 1.000000000000000000, 0.000000000000000000, 0.000000000000000000 ) ) ;
#34584 = ORIENTED_EDGE ( 'NONE', *, *, #46513, .F. ) ;
#34585 = CARTESIAN_POINT ( 'NONE',  ( -23.31729631074215092, -24.19776167542410406, -8.016098858316199838 ) ) ;
#34586 = VERTEX_POINT ( 'NONE', #518 ) ;
#34587 = ORIENTED_EDGE ( 'NONE', *, *, #10891, .F. ) ;
#34588 = CARTESIAN_POINT ( 'NONE',  ( 210.0000000000000568, 0.000000000000000000, -39.18171244307202983 ) ) ;
#34589 = VERTEX_POINT ( 'NONE', #31314 ) ;
#34590 = AXIS2_PLACEMENT_3D ( 'NONE', #5466, #32430, #16266 ) ;
#34591 = DIRECTION ( 'NONE',  ( 1.333906992743555050E-23, -1.000000000000000000, 0.000000000000000000 ) ) ;
#34592 = CARTESIAN_POINT ( 'NONE',  ( -0.3862712429686809279, -1.188820645368943163, 3.333333333333333481 ) ) ;
#34593 = LINE ( 'NONE', #46357, #42531 ) ;
#34594 = EDGE_CURVE ( 'NONE', #25029, #47864, #31817, .T. ) ;
#34595 = DIRECTION ( 'NONE',  ( 1.000000000000000000, 0.000000000000000000, 0.000000000000000000 ) ) ;
#34596 = EDGE_LOOP ( 'NONE', ( #24550, #30001, #43273, #46241 ) ) ;
#34597 = EDGE_CURVE ( 'NONE', #43608, #39344, #31193, .T. ) ;
#34598 = DIRECTION ( 'NONE',  ( 0.000000000000000000, -1.000000000000000000, 8.021842663476564905E-17 ) ) ;
#34599 = DIRECTION ( 'NONE',  ( 0.000000000000000000, 0.000000000000000000, 1.000000000000000000 ) ) ;
#34600 = EDGE_CURVE ( 'NONE', #692, #169, #265, .T. ) ;
#34601 = CARTESIAN_POINT ( 'NONE',  ( -206.6959734468149463, -1.750000000000010658, 80.81828755692798438 ) ) ;
#34602 = ORIENTED_EDGE ( 'NONE', *, *, #6119, .T. ) ;
#34603 = CARTESIAN_POINT ( 'NONE',  ( 1.011271242968688311, -0.7347315653655854817, 9.972675548442463622 ) ) ;
#34604 = CARTESIAN_POINT ( 'NONE',  ( 191.5540265531851105, 0.000000000000000000, -40.93171244307202983 ) ) ;
#34605 = ORIENTED_EDGE ( 'NONE', *, *, #46234, .T. ) ;
#34606 = VERTEX_POINT ( 'NONE', #23080 ) ;
#34607 = ORIENTED_EDGE ( 'NONE', *, *, #11772, .F. ) ;
#34608 = LINE ( 'NONE', #26899, #36934 ) ;
#34609 = ADVANCED_FACE ( 'NONE', ( #35424 ), #27451, .T. ) ;
#34610 = AXIS2_PLACEMENT_3D ( 'NONE', #20138, #24259, #16552 ) ;
#34611 = EDGE_CURVE ( 'NONE', #40582, #37522, #18213, .T. ) ;
#34612 = DIRECTION ( 'NONE',  ( 0.000000000000000000, -1.000000000000000000, 0.000000000000000000 ) ) ;
#34613 = ORIENTED_EDGE ( 'NONE', *, *, #1102, .F. ) ;
#34614 = CARTESIAN_POINT ( 'NONE',  ( 31.55402655318503236, -1.025126265847089213, 162.5682875569279133 ) ) ;
#34615 = PRESENTATION_STYLE_ASSIGNMENT (( #38481 ) ) ;
#34616 = ADVANCED_FACE ( 'NONE', ( #4101 ), #8210, .F. ) ;
#34617 = FACE_BOUND ( 'NONE', #47841, .T. ) ;
#34618 = CARTESIAN_POINT ( 'NONE',  ( -2.462075149652696027, 16.57295996686994499, 9.403735324607438884 ) ) ;
#34619 = LINE ( 'NONE', #13655, #18922 ) ;
#34620 = AXIS2_PLACEMENT_3D ( 'NONE', #50139, #39431, #32228 ) ;
#34621 = CYLINDRICAL_SURFACE ( 'NONE', #38053, 1.749999999999987566 ) ;
#34622 = CARTESIAN_POINT ( 'NONE',  ( 224.9999999999999716, -164.9999999999999716, 32.29650858650035161 ) ) ;
#34623 = AXIS2_PLACEMENT_3D ( 'NONE', #29313, #5956, #49264 ) ;
#34624 = CARTESIAN_POINT ( 'NONE',  ( -168.4459734468149463, 0.000000000000000000, -40.93171244307202983 ) ) ;
#34625 = DIRECTION ( 'NONE',  ( 0.000000000000000000, -0.000000000000000000, 1.000000000000000000 ) ) ;
#34626 = EDGE_CURVE ( 'NONE', #6992, #36853, #23486, .T. ) ;
#34627 = ADVANCED_FACE ( 'NONE', ( #7191 ), #19933, .T. ) ;
#34628 = AXIS2_PLACEMENT_3D ( 'NONE', #35738, #16705, #11857 ) ;
#34629 = VERTEX_POINT ( 'NONE', #9199 ) ;
#34630 = CARTESIAN_POINT ( 'NONE',  ( 0.000000000000000000, 57.49999999999999289, 0.000000000000000000 ) ) ;
#34631 = DIRECTION ( 'NONE',  ( -0.000000000000000000, -0.000000000000000000, -1.000000000000000000 ) ) ;
#34632 = EDGE_CURVE ( 'NONE', #18292, #39878, #16647, .T. ) ;
#34633 = ADVANCED_FACE ( 'NONE', ( #35920 ), #20252, .F. ) ;
#34634 = VECTOR ( 'NONE', #36829, 1000.000000000000000 ) ;
#34635 = CARTESIAN_POINT ( 'NONE',  ( -2.242409830259191494, 37.46921084408874947, 3.209567239418970708 ) ) ;
#34636 = FACE_OUTER_BOUND ( 'NONE', #26126, .T. ) ;
#34637 = ORIENTED_EDGE ( 'NONE', *, *, #27958, .T. ) ;
#34638 = EDGE_CURVE ( 'NONE', #5571, #17054, #36428, .T. ) ;
#34639 = LINE ( 'NONE', #34144, #31261 ) ;
#34640 = CARTESIAN_POINT ( 'NONE',  ( -7.200076171898729172, 0.000000000000000000, 0.000000000000000000 ) ) ;
#34641 = EDGE_CURVE ( 'NONE', #25320, #42631, #44567, .T. ) ;
#34642 = CARTESIAN_POINT ( 'NONE',  ( 50.11058929355270664, -7.578863168071591438, 7.455576670931136185 ) ) ;
#34643 = CARTESIAN_POINT ( 'NONE',  ( 0.000000000000000000, -168.9999999999999432, -358.0000000000002274 ) ) ;
#34644 = SURFACE_SIDE_STYLE ('',( #18963 ) ) ;
#34645 = ORIENTED_EDGE ( 'NONE', *, *, #3267, .T. ) ;
#34646 = DIRECTION ( 'NONE',  ( -1.000000000000000000, 0.000000000000000000, 0.000000000000000000 ) ) ;
#34647 = ORIENTED_EDGE ( 'NONE', *, *, #37547, .F. ) ;
#34648 = CARTESIAN_POINT ( 'NONE',  ( 194.3291528190321742, -1.750000000000009548, 39.79316129108089228 ) ) ;
#34649 = ORIENTED_EDGE ( 'NONE', *, *, #35914, .F. ) ;
#34650 = CARTESIAN_POINT ( 'NONE',  ( 350.0000000000001137, 169.0000000000000000, 343.9999999999997726 ) ) ;
#34651 = PLANE ( 'NONE',  #19996 ) ;
#34652 = ORIENTED_EDGE ( 'NONE', *, *, #45443, .T. ) ;
#34653 = CARTESIAN_POINT ( 'NONE',  ( 153.3040265531850537, 1.750000000000009992, 160.8182875569279702 ) ) ;
#34654 = ADVANCED_FACE ( 'NONE', ( #1270 ), #12167, .T. ) ;
#34655 = ORIENTED_EDGE ( 'NONE', *, *, #24754, .F. ) ;
#34656 = EDGE_CURVE ( 'NONE', #50236, #50559, #47653, .T. ) ;
#34657 = EDGE_CURVE ( 'NONE', #50425, #24051, #37182, .T. ) ;
#34658 = VERTEX_POINT ( 'NONE', #32575 ) ;
#34659 = DIRECTION ( 'NONE',  ( 0.000000000000000000, 0.000000000000000000, 1.000000000000000000 ) ) ;
#34660 = LINE ( 'NONE', #30809, #31436 ) ;
#34661 = SHAPE_REPRESENTATION ( 'fann', ( #45486 ), #46291 ) ;
#34662 = MECHANICAL_DESIGN_GEOMETRIC_PRESENTATION_REPRESENTATION (  '', ( #33013 ), #8439 ) ;
#34663 = ORIENTED_EDGE ( 'NONE', *, *, #25508, .T. ) ;
#34664 = DIRECTION ( 'NONE',  ( -0.000000000000000000, -0.000000000000000000, 1.000000000000000000 ) ) ;
#34665 = DIRECTION ( 'NONE',  ( -1.000000000000000000, -0.000000000000000000, -0.000000000000000000 ) ) ;
#34666 = EDGE_CURVE ( 'NONE', #16118, #21503, #13044, .T. ) ;
#34667 = VECTOR ( 'NONE', #2241, 1000.000000000000000 ) ;
#34668 = CARTESIAN_POINT ( 'NONE',  ( -6.619412807845042046, 7.495556955913086128, 9.646707543097347681 ) ) ;
#34669 = ORIENTED_EDGE ( 'NONE', *, *, #44613, .T. ) ;
#34670 = ORIENTED_EDGE ( 'NONE', *, *, #41343, .F. ) ;
#34671 = DIRECTION ( 'NONE',  ( 0.000000000000000000, 0.000000000000000000, -1.000000000000000000 ) ) ;
#34672 = AXIS2_PLACEMENT_3D ( 'NONE', #12230, #7895, #23538 ) ;
#34673 = ADVANCED_FACE ( 'NONE', ( #13295 ), #14557, .T. ) ;
#34674 = DIRECTION ( 'NONE',  ( -1.000000000000000000, -0.000000000000000000, -0.000000000000000000 ) ) ;
#34675 = ORIENTED_EDGE ( 'NONE', *, *, #30361, .F. ) ;
#34676 = AXIS2_PLACEMENT_3D ( 'NONE', #34349, #45841, #10727 ) ;
#34677 = DIRECTION ( 'NONE',  ( -0.5877852522924802425, 0.8090169943749422332, 0.000000000000000000 ) ) ;
#34678 = CYLINDRICAL_SURFACE ( 'NONE', #10556, 2.000000000000001776 ) ;
#34679 = ORIENTED_EDGE ( 'NONE', *, *, #17032, .F. ) ;
#34680 = DIRECTION ( 'NONE',  ( 1.000000000000000000, 0.000000000000000000, 0.000000000000000000 ) ) ;
#34681 = LINE ( 'NONE', #6446, #30037 ) ;
#34682 = B_SPLINE_SURFACE_WITH_KNOTS ( 'NONE', 3, 3, ( 
 ( #45543, #17862, #25573, #37148 ),
 ( #6829, #18360, #5817, #14263 ),
 ( #10423, #10672, #22475, #2962 ),
 ( #49623, #13756, #18116, #34042 ) ),
 .UNSPECIFIED., .F., .F., .F.,
 ( 4, 4 ),
 ( 4, 4 ),
 ( 0.000000000000000000, 1.000000000000000000 ),
 ( 0.000000000000000000, 1.000000000000000000 ),
 .UNSPECIFIED. ) ;
#34683 = ORIENTED_EDGE ( 'NONE', *, *, #39052, .T. ) ;
#34684 = EDGE_CURVE ( 'NONE', #10553, #37470, #6613, .T. ) ;
#34685 = DIRECTION ( 'NONE',  ( 0.000000000000000000, 0.000000000000000000, 1.000000000000000000 ) ) ;
#34686 = CARTESIAN_POINT ( 'NONE',  ( 113.3040265531850537, 1.749999999999996891, 160.8182875569279702 ) ) ;
#34687 = DIRECTION ( 'NONE',  ( 1.000000000000000000, 0.000000000000000000, 0.000000000000000000 ) ) ;
#34688 = CARTESIAN_POINT ( 'NONE',  ( -215.0000000000000568, 164.9999999999999716, 231.9999999999999716 ) ) ;
#34689 = VERTEX_POINT ( 'NONE', #18653 ) ;
#34690 = EDGE_CURVE ( 'NONE', #41862, #30294, #41515, .T. ) ;
#34691 = FACE_OUTER_BOUND ( 'NONE', #23462, .T. ) ;
#34692 = CARTESIAN_POINT ( 'NONE',  ( 111.5540265531850679, 0.000000000000000000, 2.568287556927950632 ) ) ;
#34693 = CARTESIAN_POINT ( 'NONE',  ( 29.61572577327002520, 16.11461842845735859, 8.807470649214879543 ) ) ;
#34694 = VERTEX_POINT ( 'NONE', #22005 ) ;
#34695 = ORIENTED_EDGE ( 'NONE', *, *, #32277, .F. ) ;
#34696 = CARTESIAN_POINT ( 'NONE',  ( 1036.499533818970804, 815.9163949454632530, 1335.986414963427706 ) ) ;
#34697 = CARTESIAN_POINT ( 'NONE',  ( 31.55402655318503236, 0.000000000000000000, -120.9317124430720725 ) ) ;
#34698 = CARTESIAN_POINT ( 'NONE',  ( -9.999999999999994671, -1.598124844265358068E-11, 9.303249460319950259 ) ) ;
#34699 = CARTESIAN_POINT ( 'NONE',  ( 7.499999999999944045, -224.9999999999999716, -224.9999999999999716 ) ) ;
#34700 = EDGE_CURVE ( 'NONE', #30887, #24424, #20176, .T. ) ;
#34701 = EDGE_CURVE ( 'NONE', #44745, #35393, #25426, .T. ) ;
#34702 = PRESENTATION_STYLE_ASSIGNMENT (( #38555 ) ) ;
#34703 = VECTOR ( 'NONE', #1954, 1000.000000000000000 ) ;
#34704 = DIRECTION ( 'NONE',  ( 0.000000000000000000, -0.000000000000000000, -1.000000000000000000 ) ) ;
#34705 = CARTESIAN_POINT ( 'NONE',  ( 181.0000000000000000, -164.9999999999999432, -358.0000000000001705 ) ) ;
#34706 = ORIENTED_EDGE ( 'NONE', *, *, #16121, .T. ) ;
#34707 = ADVANCED_FACE ( 'NONE', ( #6359, #29973 ), #2512, .T. ) ;
#34708 = CARTESIAN_POINT ( 'NONE',  ( 15.45175104485250728, -6.222373774239001065, -2.870787844569587133 ) ) ;
#34709 = AXIS2_PLACEMENT_3D ( 'NONE', #18828, #29887, #10395 ) ;
#34710 = ADVANCED_FACE ( 'NONE', ( #25868 ), #22265, .T. ) ;
#34711 = CYLINDRICAL_SURFACE ( 'NONE', #22859, 1.750000000000001554 ) ;
#34712 = DIRECTION ( 'NONE',  ( 1.333906992743555050E-23, -1.000000000000000000, 0.000000000000000000 ) ) ;
#34713 = PRESENTATION_LAYER_ASSIGNMENT (  '', '', ( #24084 ) ) ;
#34714 = ADVANCED_FACE ( 'NONE', ( #37940 ), #18406, .F. ) ;
#34715 = SURFACE_STYLE_FILL_AREA ( #31102 ) ;
#34716 = VERTEX_POINT ( 'NONE', #34323 ) ;
#34717 = VECTOR ( 'NONE', #38495, 1000.000000000000000 ) ;
#34718 = CARTESIAN_POINT ( 'NONE',  ( -6.695973446814940111, 0.000000000000000000, -165.0000000000000000 ) ) ;
#34719 = LINE ( 'NONE', #30345, #10590 ) ;
#34720 = ORIENTED_EDGE ( 'NONE', *, *, #32908, .T. ) ;
#34721 = CYLINDRICAL_SURFACE ( 'NONE', #874, 2.000000000000001776 ) ;
#34722 = CARTESIAN_POINT ( 'NONE',  ( 355.9999999999998863, -183.0000000000002274, -358.0000000000003411 ) ) ;
#34723 = DIRECTION ( 'NONE',  ( -1.000000000000000000, -0.000000000000000000, -0.000000000000000000 ) ) ;
#34724 = ORIENTED_EDGE ( 'NONE', *, *, #31296, .T. ) ;
#34725 =( BOUNDED_CURVE ( )  B_SPLINE_CURVE ( 3, ( #18717, #32014, #28155, #31764 ),
 .UNSPECIFIED., .F., .F. ) 
 B_SPLINE_CURVE_WITH_KNOTS ( ( 4, 4 ),
 ( 3.141592653589793116, 4.712388980384689674 ),
 .UNSPECIFIED. ) 
 CURVE ( )  GEOMETRIC_REPRESENTATION_ITEM ( )  RATIONAL_B_SPLINE_CURVE ( ( 1.000000000000000000, 0.8047378541243649375, 0.8047378541243649375, 1.000000000000000000 ) ) 
 REPRESENTATION_ITEM ( '' )  );
#34726 = VECTOR ( 'NONE', #17061, 1000.000000000000000 ) ;
#34727 = CARTESIAN_POINT ( 'NONE',  ( 0.8065422446123827749, -0.2117385185661261604, 9.985671801905168010 ) ) ;
#34728 = EDGE_CURVE ( 'NONE', #37995, #8296, #44829, .T. ) ;
#34729 = CARTESIAN_POINT ( 'NONE',  ( -194.9999999999999432, 164.9999999999999716, 111.9999999999999858 ) ) ;
#34730 = ORIENTED_EDGE ( 'NONE', *, *, #48979, .F. ) ;
#34731 = CARTESIAN_POINT ( 'NONE',  ( 16.02661358026014327, 4.530191650547718218, -9.683996418299976483 ) ) ;
#34732 = CARTESIAN_POINT ( 'NONE',  ( -206.6959734468149463, -1.750000000000009992, 0.8182875569279768335 ) ) ;
#34733 = DIRECTION ( 'NONE',  ( -0.000000000000000000, -0.000000000000000000, -1.000000000000000000 ) ) ;
#34734 =( BOUNDED_CURVE ( )  B_SPLINE_CURVE ( 3, ( #1566, #10270, #21305, #37734 ),
 .UNSPECIFIED., .F., .F. ) 
 B_SPLINE_CURVE_WITH_KNOTS ( ( 4, 4 ),
 ( 3.141592653589793116, 4.712388980384689674 ),
 .UNSPECIFIED. ) 
 CURVE ( )  GEOMETRIC_REPRESENTATION_ITEM ( )  RATIONAL_B_SPLINE_CURVE ( ( 1.000000000000000000, 0.8047378541243649375, 0.8047378541243649375, 1.000000000000000000 ) ) 
 REPRESENTATION_ITEM ( '' )  );
#34735 = ORIENTED_EDGE ( 'NONE', *, *, #19553, .F. ) ;
#34736 = ORIENTED_EDGE ( 'NONE', *, *, #17964, .T. ) ;
#34737 = CARTESIAN_POINT ( 'NONE',  ( 167.0000000000000000, -174.9999999999999716, -99.00000000000014211 ) ) ;
#34738 = CARTESIAN_POINT ( 'NONE',  ( 168.9999999999999716, -272.5000000000000000, -98.99999999999990052 ) ) ;
#34739 = ORIENTED_EDGE ( 'NONE', *, *, #45443, .F. ) ;
#34740 = EDGE_LOOP ( 'NONE', ( #45839, #33750, #33027 ) ) ;
#34741 = CARTESIAN_POINT ( 'NONE',  ( 30.00000000000029132, 17.00000000000000000, -60.00000000000000000 ) ) ;
#34742 = DIRECTION ( 'NONE',  ( -0.000000000000000000, -0.000000000000000000, -1.000000000000000000 ) ) ;
#34743 = VECTOR ( 'NONE', #6189, 1000.000000000000000 ) ;
#34744 = CARTESIAN_POINT ( 'NONE',  ( 2.499999999999952927, -204.9999999999999716, -230.2499999999999716 ) ) ;
#34745 = VERTEX_POINT ( 'NONE', #13791 ) ;
#34746 = CARTESIAN_POINT ( 'NONE',  ( 344.0000000000000000, 175.0000000000000284, -110.0000000000002132 ) ) ;
#34747 = VECTOR ( 'NONE', #251, 1000.000000000000000 ) ;
#34748 = VERTEX_POINT ( 'NONE', #30213 ) ;
#34749 = EDGE_CURVE ( 'NONE', #34922, #25186, #45822, .T. ) ;
#34750 =( BOUNDED_CURVE ( )  B_SPLINE_CURVE ( 3, ( #7591, #46792, #38907, #45787 ),
 .UNSPECIFIED., .F., .F. ) 
 B_SPLINE_CURVE_WITH_KNOTS ( ( 4, 4 ),
 ( 1.570796326794896558, 3.141592653589793116 ),
 .UNSPECIFIED. ) 
 CURVE ( )  GEOMETRIC_REPRESENTATION_ITEM ( )  RATIONAL_B_SPLINE_CURVE ( ( 1.000000000000000000, 0.8047378541243649375, 0.8047378541243649375, 1.000000000000000000 ) ) 
 REPRESENTATION_ITEM ( '' )  );
#34751 = CYLINDRICAL_SURFACE ( 'NONE', #32889, 1.880036658038868103 ) ;
#34752 = CARTESIAN_POINT ( 'NONE',  ( -23.13346437080424778, 39.73622551878982989, -8.016098858316205167 ) ) ;
#34753 = CARTESIAN_POINT ( 'NONE',  ( 168.9999999999999716, -180.9999999999999716, -350.0000000000001705 ) ) ;
#34754 = ORIENTED_EDGE ( 'NONE', *, *, #17032, .T. ) ;
#34755 = VERTEX_POINT ( 'NONE', #25360 ) ;
#34756 = ORIENTED_EDGE ( 'NONE', *, *, #27985, .T. ) ;
#34757 = CARTESIAN_POINT ( 'NONE',  ( -8.445973446814914354, 0.000000000000000000, 162.5682875569279702 ) ) ;
#34758 = SURFACE_STYLE_USAGE ( .BOTH. , #46490 ) ;
#34759 = CARTESIAN_POINT ( 'NONE',  ( 0.09523839817332763191, 1.466467394239034050, 9.958264684458713489 ) ) ;
#34760 = ORIENTED_EDGE ( 'NONE', *, *, #27735, .F. ) ;
#34761 = ORIENTED_EDGE ( 'NONE', *, *, #8038, .F. ) ;
#34762 = LINE ( 'NONE', #38353, #16821 ) ;
#34763 = VERTEX_POINT ( 'NONE', #37190 ) ;
#34764 = LINE ( 'NONE', #16011, #3729 ) ;
#34765 = CARTESIAN_POINT ( 'NONE',  ( 71.55402655318505367, 0.000000000000000000, 122.5682875569279844 ) ) ;
#34766 = CARTESIAN_POINT ( 'NONE',  ( 73.30402655318508209, -1.750000000000010658, -119.1817124430720440 ) ) ;
#34767 = CARTESIAN_POINT ( 'NONE',  ( -88.44597344681497475, 0.000000000000000000, -37.43171244307200141 ) ) ;
#34768 = ADVANCED_FACE ( 'NONE', ( #41013 ), #5857, .F. ) ;
#34769 = AXIS2_PLACEMENT_3D ( 'NONE', #21990, #26089, #34560 ) ;
#34770 = ADVANCED_FACE ( 'NONE', ( #9958 ), #6109, .T. ) ;
#34771 = CARTESIAN_POINT ( 'NONE',  ( 8.277096487746778308, -50.00000000000000711, 7.455576670931136185 ) ) ;
#34772 = VERTEX_POINT ( 'NONE', #37681 ) ;
#34773 = ORIENTED_EDGE ( 'NONE', *, *, #4909, .F. ) ;
#34774 = LINE ( 'NONE', #121, #27196 ) ;
#34775 = DIRECTION ( 'NONE',  ( 0.000000000000000000, 0.000000000000000000, 1.000000000000000000 ) ) ;
#34776 = ADVANCED_FACE ( 'NONE', ( #18152 ), #33830, .F. ) ;
#34777 = DIRECTION ( 'NONE',  ( 1.000000000000000000, 0.000000000000000000, -0.000000000000000000 ) ) ;
#34778 = CARTESIAN_POINT ( 'NONE',  ( 113.3040265531850537, 0.000000000000000000, 165.0000000000000000 ) ) ;
#34779 = EDGE_CURVE ( 'NONE', #10187, #32574, #48102, .T. ) ;
#34780 = ADVANCED_FACE ( 'NONE', ( #20373 ), #11479, .F. ) ;
#34781 = CARTESIAN_POINT ( 'NONE',  ( -1.540526284687967706, 1.371707213411501147, 9.886433018048069954 ) ) ;
#34782 = AXIS2_PLACEMENT_3D ( 'NONE', #775, #278, #27466 ) ;
#34783 = AXIS2_PLACEMENT_3D ( 'NONE', #15026, #38141, #49854 ) ;
#34784 = FACE_OUTER_BOUND ( 'NONE', #15289, .T. ) ;
#34785 = ORIENTED_EDGE ( 'NONE', *, *, #14919, .F. ) ;
#34786 = AXIS2_PLACEMENT_3D ( 'NONE', #43090, #4610, #31053 ) ;
#34787 = CARTESIAN_POINT ( 'NONE',  ( 85.00000000000056843, 17.00000000000000000, -54.99999999999999289 ) ) ;
#34788 = EDGE_CURVE ( 'NONE', #29488, #25367, #15339, .T. ) ;
#34789 = CYLINDRICAL_SURFACE ( 'NONE', #46746, 1.750000000000015543 ) ;
#34790 = AXIS2_PLACEMENT_3D ( 'NONE', #3354, #18743, #33918 ) ;
#34791 = ORIENTED_EDGE ( 'NONE', *, *, #16684, .F. ) ;
#34792 = CARTESIAN_POINT ( 'NONE',  ( 113.3040265531850537, -1.749999999999996891, -159.1817124430720298 ) ) ;
#34793 = CARTESIAN_POINT ( 'NONE',  ( -28.52604530808686079, -41.07801380285659576, -3.760136334089591248 ) ) ;
#34794 = DIRECTION ( 'NONE',  ( -1.000000000000000000, -0.000000000000000000, -0.000000000000000000 ) ) ;
#34795 = ORIENTED_EDGE ( 'NONE', *, *, #11097, .F. ) ;
#34796 = ORIENTED_EDGE ( 'NONE', *, *, #39324, .F. ) ;
#34797 = CYLINDRICAL_SURFACE ( 'NONE', #46336, 1.750000000000001554 ) ;
#34798 = CARTESIAN_POINT ( 'NONE',  ( 73.30402655318508209, -1.750000000000010658, 120.8182875569279702 ) ) ;
#34799 = AXIS2_PLACEMENT_3D ( 'NONE', #40124, #44694, #5215 ) ;
#34800 = VERTEX_POINT ( 'NONE', #43967 ) ;
#34801 = ORIENTED_EDGE ( 'NONE', *, *, #1438, .T. ) ;
#34802 = DIRECTION ( 'NONE',  ( 0.000000000000000000, 1.000000000000000000, 7.004339610132985974E-48 ) ) ;
#34803 = LINE ( 'NONE', #27080, #29849 ) ;
#34804 = CARTESIAN_POINT ( 'NONE',  ( 340.0000000000000000, 175.0000000000000284, -94.00000000000019895 ) ) ;
#34805 = ORIENTED_EDGE ( 'NONE', *, *, #34728, .F. ) ;
#34806 = AXIS2_PLACEMENT_3D ( 'NONE', #23717, #27576, #43703 ) ;
#34807 = ORIENTED_EDGE ( 'NONE', *, *, #10461, .T. ) ;
#34808 = ORIENTED_EDGE ( 'NONE', *, *, #17840, .F. ) ;
#34809 = EDGE_CURVE ( 'NONE', #9595, #36017, #568, .T. ) ;
#34810 = CARTESIAN_POINT ( 'NONE',  ( 340.0000000000000568, 169.0000000000000000, 339.9999999999997726 ) ) ;
#34811 = CARTESIAN_POINT ( 'NONE',  ( -46.69597344681494633, -1.750000000000009992, -159.1817124430720298 ) ) ;
#34812 = VERTEX_POINT ( 'NONE', #26874 ) ;
#34813 = DIRECTION ( 'NONE',  ( -1.000000000000000000, -0.000000000000000000, -0.000000000000000000 ) ) ;
#34814 = DIRECTION ( 'NONE',  ( -1.000000000000000000, 0.000000000000000000, 0.000000000000000000 ) ) ;
#34815 = CARTESIAN_POINT ( 'NONE',  ( 1.080340181645069064, -0.5751155560365959207, 9.966990753365129407 ) ) ;
#34816 = AXIS2_PLACEMENT_3D ( 'NONE', #28793, #41274, #31898 ) ;
#34817 = ORIENTED_EDGE ( 'NONE', *, *, #24668, .T. ) ;
#34818 = VERTEX_POINT ( 'NONE', #42269 ) ;
#34819 = CARTESIAN_POINT ( 'NONE',  ( 210.0000000000000568, 0.000000000000000000, 160.8182875569279702 ) ) ;
#34820 = CARTESIAN_POINT ( 'NONE',  ( -128.4459734468149463, -1.025126265847081442, 162.5682875569279133 ) ) ;
#34821 = FACE_OUTER_BOUND ( 'NONE', #27212, .T. ) ;
#34822 = ORIENTED_EDGE ( 'NONE', *, *, #6840, .T. ) ;
#34823 = ORIENTED_EDGE ( 'NONE', *, *, #852, .T. ) ;
#34824 = VECTOR ( 'NONE', #20155, 1000.000000000000000 ) ;
#34825 = CARTESIAN_POINT ( 'NONE',  ( 192.2789002873380184, 1.750000000000010436, 119.7931612910808781 ) ) ;
#34826 = LINE ( 'NONE', #26085, #32981 ) ;
#34827 = DIRECTION ( 'NONE',  ( 0.000000000000000000, 0.000000000000000000, 1.000000000000000000 ) ) ;
#34828 = DIRECTION ( 'NONE',  ( 0.000000000000000000, -1.000000000000000000, 0.000000000000000000 ) ) ;
#34829 = LINE ( 'NONE', #15048, #22855 ) ;
#34830 = CARTESIAN_POINT ( 'NONE',  ( -69.99999999999972999, 16.00000000000000000, -84.99999999999998579 ) ) ;
#34831 = ORIENTED_EDGE ( 'NONE', *, *, #34932, .T. ) ;
#34832 = SURFACE_STYLE_USAGE ( .BOTH. , #4459 ) ;
#34833 = CARTESIAN_POINT ( 'NONE',  ( 181.0000000000000000, 6.000000000000060396, 339.9999999999998295 ) ) ;
#34834 = CARTESIAN_POINT ( 'NONE',  ( 210.0000000000000568, 0.000000000000000000, 0.8182875569279768335 ) ) ;
#34835 = DIRECTION ( 'NONE',  ( 0.000000000000000000, 0.000000000000000000, 1.000000000000000000 ) ) ;
#34836 = DIRECTION ( 'NONE',  ( -1.000000000000000000, 0.000000000000000000, 0.000000000000000000 ) ) ;
#34837 = EDGE_CURVE ( 'NONE', #4803, #38537, #4151, .T. ) ;
#34838 = AXIS2_PLACEMENT_3D ( 'NONE', #41124, #32677, #1135 ) ;
#34839 = EDGE_LOOP ( 'NONE', ( #35043, #48306, #6072, #19878, #4250, #43279 ) ) ;
#34840 = EDGE_CURVE ( 'NONE', #37272, #42411, #49943, .T. ) ;
#34841 = CARTESIAN_POINT ( 'NONE',  ( 8.277096487746778308, -50.00000000000000711, 7.455576670931136185 ) ) ;
#34842 = CARTESIAN_POINT ( 'NONE',  ( 33.30402655318503946, -1.750000000000010658, 80.81828755692798438 ) ) ;
#34843 = CARTESIAN_POINT ( 'NONE',  ( 153.3040265531850537, 1.750000000000010214, 40.81828755692798438 ) ) ;
#34844 = EDGE_LOOP ( 'NONE', ( #4249, #40770, #4557, #7292, #49275 ) ) ;
#34845 = SURFACE_STYLE_FILL_AREA ( #14552 ) ;
#34846 = LINE ( 'NONE', #50427, #1634 ) ;
#34847 = CIRCLE ( 'NONE', #46254, 4.000000000000003553 ) ;
#34848 = ORIENTED_EDGE ( 'NONE', *, *, #15788, .F. ) ;
#34849 = DIRECTION ( 'NONE',  ( 1.000000000000000000, 0.000000000000000000, 0.000000000000000000 ) ) ;
#34850 = DIRECTION ( 'NONE',  ( -1.000000000000000000, 0.000000000000000000, 0.000000000000000000 ) ) ;
#34851 = CYLINDRICAL_SURFACE ( 'NONE', #43675, 0.5000000000000004441 ) ;
#34852 = DIRECTION ( 'NONE',  ( -1.000000000000000000, 0.000000000000000000, 0.000000000000000000 ) ) ;
#34853 = ORIENTED_EDGE ( 'NONE', *, *, #7992, .F. ) ;
#34854 = CARTESIAN_POINT ( 'NONE',  ( 185.0000000000000000, -5.999999999999950262, -340.0000000000001137 ) ) ;
#34855 = VERTEX_POINT ( 'NONE', #4977 ) ;
#34856 = ORIENTED_EDGE ( 'NONE', *, *, #24300, .T. ) ;
#34857 = AXIS2_PLACEMENT_3D ( 'NONE', #35024, #50595, #22931 ) ;
#34858 = PLANE ( 'NONE',  #12345 ) ;
#34859 = VERTEX_POINT ( 'NONE', #10968 ) ;
#34860 = FACE_OUTER_BOUND ( 'NONE', #37887, .T. ) ;
#34861 = CARTESIAN_POINT ( 'NONE',  ( 210.0000000000000568, 0.000000000000000000, -79.18171244307201562 ) ) ;
#34862 = CARTESIAN_POINT ( 'NONE',  ( 0.2455008416098105606, 1.553107091521340966, 9.945241992664895392 ) ) ;
#34863 = DIRECTION ( 'NONE',  ( 0.000000000000000000, 0.000000000000000000, -1.000000000000000000 ) ) ;
#34864 = ORIENTED_EDGE ( 'NONE', *, *, #16278, .T. ) ;
#34865 = ADVANCED_FACE ( 'NONE', ( #50680 ), #20634, .T. ) ;
#34866 = PLANE ( 'NONE',  #29085 ) ;
#34867 = DIRECTION ( 'NONE',  ( -1.000000000000000000, 0.000000000000000000, -1.612977847700450206E-50 ) ) ;
#34868 = SURFACE_SIDE_STYLE ('',( #27917 ) ) ;
#34869 = VECTOR ( 'NONE', #23984, 1000.000000000000000 ) ;
#34870 = ORIENTED_EDGE ( 'NONE', *, *, #28012, .F. ) ;
#34871 = CARTESIAN_POINT ( 'NONE',  ( 75.05402655318509630, 1.025126265847089657, -37.43171244307202272 ) ) ;
#34872 = DIRECTION ( 'NONE',  ( -0.000000000000000000, -0.000000000000000000, -1.000000000000000000 ) ) ;
#34873 = ORIENTED_EDGE ( 'NONE', *, *, #25535, .F. ) ;
#34874 = VERTEX_POINT ( 'NONE', #49910 ) ;
#34875 = EDGE_LOOP ( 'NONE', ( #12045, #20251, #19612, #32454 ) ) ;
#34876 = LINE ( 'NONE', #46865, #22968 ) ;
#34877 = AXIS2_PLACEMENT_3D ( 'NONE', #27043, #42681, #38866 ) ;
#34878 = PLANE ( 'NONE',  #2866 ) ;
#34879 = ORIENTED_EDGE ( 'NONE', *, *, #36859, .T. ) ;
#34880 = DIRECTION ( 'NONE',  ( 1.000000000000000000, 0.000000000000000000, 0.000000000000000000 ) ) ;
#34881 = CARTESIAN_POINT ( 'NONE',  ( -8.445973446814964092, 1.025126265847097429, -120.9317124430720440 ) ) ;
#34882 = FACE_OUTER_BOUND ( 'NONE', #17925, .T. ) ;
#34883 = DIRECTION ( 'NONE',  ( 0.000000000000000000, 1.000000000000000000, -0.000000000000000000 ) ) ;
#34884 = CARTESIAN_POINT ( 'NONE',  ( -48.44597344681496054, 1.025126265847089213, 42.56828755692799149 ) ) ;
#34885 = CARTESIAN_POINT ( 'NONE',  ( 151.5540265531850537, -1.025126265847089879, 82.56828755692798438 ) ) ;
#34886 = CIRCLE ( 'NONE', #12738, 4.999999999999997335 ) ;
#34887 = FACE_OUTER_BOUND ( 'NONE', #25866, .T. ) ;
#34888 = SURFACE_SIDE_STYLE ('',( #19200 ) ) ;
#34889 = CARTESIAN_POINT ( 'NONE',  ( -9.999999999999994671, -1.598124844265358068E-11, 9.303249460319950259 ) ) ;
#34890 =( BOUNDED_CURVE ( )  B_SPLINE_CURVE ( 3, ( #18175, #46098, #34871, #45352 ),
 .UNSPECIFIED., .F., .F. ) 
 B_SPLINE_CURVE_WITH_KNOTS ( ( 4, 4 ),
 ( 1.570796326794896558, 3.141592653589793116 ),
 .UNSPECIFIED. ) 
 CURVE ( )  GEOMETRIC_REPRESENTATION_ITEM ( )  RATIONAL_B_SPLINE_CURVE ( ( 1.000000000000000000, 0.8047378541243649375, 0.8047378541243649375, 1.000000000000000000 ) ) 
 REPRESENTATION_ITEM ( '' )  );
#34891 = CARTESIAN_POINT ( 'NONE',  ( -31.44259251615275019, -38.95901822126145220, -9.367992836599954742 ) ) ;
#34892 = B_SPLINE_CURVE_WITH_KNOTS ( 'NONE', 3,
 ( #21150, #36832, #1660, #13451 ),
 .UNSPECIFIED., .F., .F.,
 ( 4, 4 ),
 ( 0.9811748202683396869, 0.9878904167554125593 ),
 .UNSPECIFIED. ) ;
#34893 = VECTOR ( 'NONE', #5456, 1000.000000000000000 ) ;
#34894 = ORIENTED_EDGE ( 'NONE', *, *, #41074, .T. ) ;
#34895 = CARTESIAN_POINT ( 'NONE',  ( 344.0000000000000000, 165.0000000000000000, -94.00000000000019895 ) ) ;
#34896 = CARTESIAN_POINT ( 'NONE',  ( -44.94597344681493922, 2.143131898507880377E-16, 82.56828755692798438 ) ) ;
#34897 = CARTESIAN_POINT ( 'NONE',  ( -125.6708471809678542, -1.749999999999996669, 121.8434138227750481 ) ) ;
#34898 = CARTESIAN_POINT ( 'NONE',  ( 79.99999999999997158, 17.00000000000000000, -90.00000000000000000 ) ) ;
#34899 = ORIENTED_EDGE ( 'NONE', *, *, #48551, .T. ) ;
#34900 = CARTESIAN_POINT ( 'NONE',  ( 214.9999999999999432, 164.9999999999999716, 497.2965085865001811 ) ) ;
#34901 = EDGE_CURVE ( 'NONE', #21950, #3623, #19159, .T. ) ;
#34902 = CARTESIAN_POINT ( 'NONE',  ( -86.69597344681496054, 0.000000000000000000, 165.0000000000000000 ) ) ;
#34903 = CARTESIAN_POINT ( 'NONE',  ( -45.64490844644706868, -21.32281559348764333, 8.807470649214879543 ) ) ;
#34904 = LINE ( 'NONE', #15634, #45476 ) ;
#34905 = CARTESIAN_POINT ( 'NONE',  ( 168.9999999999999716, -164.9999999999999432, -340.0000000000001137 ) ) ;
#34906 = ORIENTED_EDGE ( 'NONE', *, *, #22992, .F. ) ;
#34907 = CARTESIAN_POINT ( 'NONE',  ( 168.9999999999999716, -174.9999999999999716, -358.0000000000001705 ) ) ;
#34908 = ORIENTED_EDGE ( 'NONE', *, *, #35568, .T. ) ;
#34909 = LINE ( 'NONE', #39007, #11436 ) ;
#34910 = VECTOR ( 'NONE', #42466, 1000.000000000000000 ) ;
#34911 = EDGE_LOOP ( 'NONE', ( #19054, #4236, #44779, #26651 ) ) ;
#34912 = CARTESIAN_POINT ( 'NONE',  ( 343.9999999999998863, -165.0000000000001137, -92.00000000000019895 ) ) ;
#34914 = EDGE_CURVE ( 'NONE', #22581, #46047, #31248, .T. ) ;
#34913 = DIRECTION ( 'NONE',  ( 0.000000000000000000, -1.000000000000000000, 0.000000000000000000 ) ) ;
#34915 = VECTOR ( 'NONE', #43071, 1000.000000000000000 ) ;
#34916 = EDGE_LOOP ( 'NONE', ( #5001, #15431, #50052, #46755, #48969, #37379 ) ) ;
#34917 = CYLINDRICAL_SURFACE ( 'NONE', #39645, 1.750000000000001554 ) ;
#34918 = ORIENTED_EDGE ( 'NONE', *, *, #21171, .F. ) ;
#34919 = EDGE_CURVE ( 'NONE', #907, #20271, #4731, .T. ) ;
#34920 = ADVANCED_FACE ( 'NONE', ( #14816 ), #42854, .T. ) ;
#34921 = MECHANICAL_DESIGN_GEOMETRIC_PRESENTATION_REPRESENTATION (  '', ( #29957 ), #7846 ) ;
#34922 = VERTEX_POINT ( 'NONE', #13434 ) ;
#34923 = CARTESIAN_POINT ( 'NONE',  ( 339.9999999999999432, -168.9999999999999432, -344.0000000000001705 ) ) ;
#34924 = CARTESIAN_POINT ( 'NONE',  ( 210.0000000000000568, 0.000000000000000000, -39.18171244307202983 ) ) ;
#34925 = AXIS2_PLACEMENT_3D ( 'NONE', #21351, #2117, #17763 ) ;
#34926 = ORIENTED_EDGE ( 'NONE', *, *, #5314, .T. ) ;
#34927 = CARTESIAN_POINT ( 'NONE',  ( -23.29043492822808759, 24.10797434788186067, 1.847720168420772691 ) ) ;
#34928 = CARTESIAN_POINT ( 'NONE',  ( 34.91952936320839740, -13.67027684621004546, -9.422646554964178023 ) ) ;
#34929 = DIRECTION ( 'NONE',  ( 0.000000000000000000, 0.000000000000000000, 1.000000000000000000 ) ) ;
#34930 = ORIENTED_EDGE ( 'NONE', *, *, #1979, .F. ) ;
#34931 = CARTESIAN_POINT ( 'NONE',  ( -167.7210997126620384, -1.750000000000010214, 119.7931612910808781 ) ) ;
#34932 = EDGE_CURVE ( 'NONE', #18558, #21591, #29096, .T. ) ;
#34933 = CARTESIAN_POINT ( 'NONE',  ( 193.3040265531851105, -1.750000000000009992, -159.1817124430720298 ) ) ;
#34934 = EDGE_CURVE ( 'NONE', #3137, #50500, #15065, .T. ) ;
#34935 = AXIS2_PLACEMENT_3D ( 'NONE', #10851, #7007, #30110 ) ;
#34936 = CARTESIAN_POINT ( 'NONE',  ( 130.0000000000008811, 17.00000000000000000, -24.99999999999999289 ) ) ;
#34937 = EDGE_CURVE ( 'NONE', #44965, #32324, #9590, .T. ) ;
#34938 = EDGE_CURVE ( 'NONE', #25767, #13303, #25240, .T. ) ;
#34939 = ORIENTED_EDGE ( 'NONE', *, *, #19663, .T. ) ;
#34940 = DIRECTION ( 'NONE',  ( 0.000000000000000000, -1.000000000000000000, 1.604368532695312981E-16 ) ) ;
#34941 = CARTESIAN_POINT ( 'NONE',  ( 181.0000000000000000, -97.49999999999997158, -115.0000000000001563 ) ) ;
#34942 = ORIENTED_EDGE ( 'NONE', *, *, #5509, .T. ) ;
#34943 = FACE_OUTER_BOUND ( 'NONE', #20888, .T. ) ;
#34944 = DIRECTION ( 'NONE',  ( 0.000000000000000000, 1.000000000000000000, 6.123233995736766036E-17 ) ) ;
#34945 = ORIENTED_EDGE ( 'NONE', *, *, #19577, .F. ) ;
#34946 = FACE_BOUND ( 'NONE', #19578, .T. ) ;
#34947 = PLANE ( 'NONE',  #43797 ) ;
#34948 = LINE ( 'NONE', #2842, #19725 ) ;
#34949 = CARTESIAN_POINT ( 'NONE',  ( -84.94597344681493212, -1.025126265847088991, 2.568287556927986159 ) ) ;
#34950 = VECTOR ( 'NONE', #39274, 1000.000000000000000 ) ;
#34951 = VECTOR ( 'NONE', #4691, 1000.000000000000000 ) ;
#34952 = ORIENTED_EDGE ( 'NONE', *, *, #36038, .T. ) ;
#34953 = CARTESIAN_POINT ( 'NONE',  ( 47.88254548617766204, -14.43607691413525984, -3.760136334089591248 ) ) ;
#34954 =( LENGTH_UNIT ( ) NAMED_UNIT ( * ) SI_UNIT ( .MILLI., .METRE. ) );
#34955 = CARTESIAN_POINT ( 'NONE',  ( -127.7210997126620242, -1.749999999999996669, -160.2068387089191219 ) ) ;
#34956 = ORIENTED_EDGE ( 'NONE', *, *, #15224, .T. ) ;
#34957 = ADVANCED_FACE ( 'NONE', ( #21134 ), #8076, .T. ) ;
#34958 = EDGE_LOOP ( 'NONE', ( #6102, #4633, #7660, #21404, #45181, #40823, #17257, #32764 ) ) ;
#34959 = DIRECTION ( 'NONE',  ( 1.000000000000000000, -1.047444401652940007E-14, -1.745740669421566678E-14 ) ) ;
#34960 = DIRECTION ( 'NONE',  ( 0.000000000000000000, -1.000000000000000000, 2.537652627714643577E-15 ) ) ;
#34961 = VECTOR ( 'NONE', #3209, 1000.000000000000000 ) ;
#34962 = DIRECTION ( 'NONE',  ( 0.000000000000000000, -0.000000000000000000, -1.000000000000000000 ) ) ;
#34963 = EDGE_CURVE ( 'NONE', #35915, #37221, #44464, .T. ) ;
#34964 = EDGE_CURVE ( 'NONE', #32976, #28202, #17542, .T. ) ;
#34965 =( NAMED_UNIT ( * ) PLANE_ANGLE_UNIT ( ) SI_UNIT ( $, .RADIAN. ) );
#34966 = CARTESIAN_POINT ( 'NONE',  ( -48.44597344681495343, 0.000000000000000000, 165.0000000000000000 ) ) ;
#34967 = AXIS2_PLACEMENT_3D ( 'NONE', #50144, #22496, #3233 ) ;
#34968 = CYLINDRICAL_SURFACE ( 'NONE', #40390, 1.749999999999987566 ) ;
#34969 = VERTEX_POINT ( 'NONE', #40648 ) ;
#34970 = LINE ( 'NONE', #50535, #48457 ) ;
#34971 = EDGE_CURVE ( 'NONE', #16197, #40485, #21518, .T. ) ;
#34972 = CARTESIAN_POINT ( 'NONE',  ( -114.9999999999994031, 17.00000000000000000, -54.99999999999999289 ) ) ;
#34973 = CARTESIAN_POINT ( 'NONE',  ( 210.0000000000000568, 0.000000000000000000, -159.1817124430720298 ) ) ;
#34974 = EDGE_CURVE ( 'NONE', #4263, #30568, #48799, .T. ) ;
#34975 = DIRECTION ( 'NONE',  ( 0.000000000000000000, 1.000000000000000000, 0.000000000000000000 ) ) ;
#34976 = CIRCLE ( 'NONE', #34117, 4.000000000000003553 ) ;
#34977 = FILL_AREA_STYLE_COLOUR ( '', #49406 ) ;
#34978 = EDGE_LOOP ( 'NONE', ( #2065, #49469 ) ) ;
#34979 = PLANE ( 'NONE',  #34374 ) ;
#34980 = CARTESIAN_POINT ( 'NONE',  ( 13.92102703536701114, 30.85732372859822803, 8.356839323120299312 ) ) ;
#34981 = ORIENTED_EDGE ( 'NONE', *, *, #41736, .F. ) ;
#34982 = LINE ( 'NONE', #42636, #8226 ) ;
#34983 = CARTESIAN_POINT ( 'NONE',  ( 1.250000000000000222, 0.000000000000000000, 10.00000000000000000 ) ) ;
#34984 = CARTESIAN_POINT ( 'NONE',  ( 168.9999999999999716, 6.000000000000060396, -340.0000000000001137 ) ) ;
#34985 = ORIENTED_EDGE ( 'NONE', *, *, #45180, .T. ) ;
#34986 = PLANE ( 'NONE',  #8138 ) ;
#34987 = AXIS2_PLACEMENT_3D ( 'NONE', #24334, #43039, #24073 ) ;
#34988 = LINE ( 'NONE', #18275, #13114 ) ;
#34989 = ORIENTED_EDGE ( 'NONE', *, *, #9665, .T. ) ;
#34990 = CYLINDRICAL_SURFACE ( 'NONE', #43478, 4.000000000000003553 ) ;
#34991 = EDGE_CURVE ( 'NONE', #38289, #29160, #32689, .T. ) ;
#34992 = CARTESIAN_POINT ( 'NONE',  ( 155.0540265531850537, -1.025126265847089435, -77.43171244307200141 ) ) ;
#34993 = CARTESIAN_POINT ( 'NONE',  ( 210.0000000000000568, 0.000000000000000000, -39.18171244307202983 ) ) ;
#34994 = ORIENTED_EDGE ( 'NONE', *, *, #50578, .T. ) ;
#34995 = VERTEX_POINT ( 'NONE', #1146 ) ;
#34996 = DIRECTION ( 'NONE',  ( 0.000000000000000000, 1.000000000000000000, 0.000000000000000000 ) ) ;
#34997 = ADVANCED_FACE ( 'NONE', ( #9835 ), #20883, .F. ) ;
#34998 = CARTESIAN_POINT ( 'NONE',  ( 15.42815683172628738, 34.17926237904582365, 7.697694107796191787 ) ) ;
#34999 = EDGE_CURVE ( 'NONE', #22621, #30282, #2152, .T. ) ;
#35000 = ADVANCED_FACE ( 'NONE', ( #29590 ), #32449, .F. ) ;
#35001 = EDGE_LOOP ( 'NONE', ( #28429, #41026 ) ) ;
#35002 = ORIENTED_EDGE ( 'NONE', *, *, #31964, .T. ) ;
#35003 = CARTESIAN_POINT ( 'NONE',  ( 195.0540265531851105, 1.025126265847089657, -120.9317124430720440 ) ) ;
#35004 = LINE ( 'NONE', #3922, #7090 ) ;
#35005 = CARTESIAN_POINT ( 'NONE',  ( 0.000000000000000000, -180.9999999999999716, -340.0000000000001705 ) ) ;
#35006 = ORIENTED_EDGE ( 'NONE', *, *, #25509, .F. ) ;
#35007 = CARTESIAN_POINT ( 'NONE',  ( 339.9999999999999432, 169.0000000000000000, -356.0000000000002274 ) ) ;
#35008 = EDGE_CURVE ( 'NONE', #8469, #42421, #40854, .T. ) ;
#35009 = VERTEX_POINT ( 'NONE', #14447 ) ;
#35010 = EDGE_CURVE ( 'NONE', #38333, #10859, #46057, .T. ) ;
#35011 = DIRECTION ( 'NONE',  ( 1.000000000000000000, 0.000000000000000000, 0.000000000000000000 ) ) ;
#35012 = VECTOR ( 'NONE', #7402, 1000.000000000000000 ) ;
#35013 = CARTESIAN_POINT ( 'NONE',  ( -167.7210997126620384, 1.750000000000010436, -80.20683870891910772 ) ) ;
#35014 = CARTESIAN_POINT ( 'NONE',  ( 1.066995270233474624, -50.00000000000000711, -3.760136334089591248 ) ) ;
#35015 = ORIENTED_EDGE ( 'NONE', *, *, #26413, .F. ) ;
#35016 = ORIENTED_EDGE ( 'NONE', *, *, #33394, .T. ) ;
#35017 = ORIENTED_EDGE ( 'NONE', *, *, #12340, .F. ) ;
#35018 = LINE ( 'NONE', #7804, #29598 ) ;
#35019 =( NAMED_UNIT ( * ) PLANE_ANGLE_UNIT ( ) SI_UNIT ( $, .RADIAN. ) );
#35020 = LINE ( 'NONE', #15487, #37186 ) ;
#35021 = ORIENTED_EDGE ( 'NONE', *, *, #18868, .T. ) ;
#35022 = CARTESIAN_POINT ( 'NONE',  ( 194.3291528190321742, 1.750000000000009548, 39.79316129108089228 ) ) ;
#35023 = EDGE_LOOP ( 'NONE', ( #7785, #18494, #3476, #35551, #20015 ) ) ;
#35024 = CARTESIAN_POINT ( 'NONE',  ( 35.00000000000028422, 17.00000000000000000, -60.00000000000000000 ) ) ;
#35025 = ORIENTED_EDGE ( 'NONE', *, *, #19952, .T. ) ;
#35026 = DIRECTION ( 'NONE',  ( 1.000000000000000000, 0.000000000000000000, 0.000000000000000000 ) ) ;
#35027 = FACE_BOUND ( 'NONE', #286, .T. ) ;
#35028 = CARTESIAN_POINT ( 'NONE',  ( -0.3370904143228978245, 0.2449105217885259589, 10.00000000000000000 ) ) ;
#35029 = DIRECTION ( 'NONE',  ( 1.000000000000000000, 0.000000000000000000, -1.586032892321651989E-16 ) ) ;
#35030 = EDGE_CURVE ( 'NONE', #39708, #43597, #22150, .T. ) ;
#35031 = EDGE_CURVE ( 'NONE', #23937, #13514, #1702, .T. ) ;
#35032 = DIRECTION ( 'NONE',  ( -1.000000000000000000, -0.000000000000000000, -0.000000000000000000 ) ) ;
#35033 = ORIENTED_EDGE ( 'NONE', *, *, #6400, .F. ) ;
#35034 = ORIENTED_EDGE ( 'NONE', *, *, #49025, .F. ) ;
#35035 = B_SPLINE_CURVE_WITH_KNOTS ( 'NONE', 3,
 ( #9837, #5734, #21640, #44716 ),
 .UNSPECIFIED., .F., .F.,
 ( 4, 4 ),
 ( 0.000000000000000000, 0.2637263876330695478 ),
 .UNSPECIFIED. ) ;
#35036 = CARTESIAN_POINT ( 'NONE',  ( -26.42016489236612387, -32.24895757977012067, -9.387872844313825738 ) ) ;
#35037 = CARTESIAN_POINT ( 'NONE',  ( 192.2789002873380184, -1.750000000000009548, 41.84341382277508359 ) ) ;
#35038 = FACE_OUTER_BOUND ( 'NONE', #47577, .T. ) ;
#35039 = CYLINDRICAL_SURFACE ( 'NONE', #34806, 1.750000000000008438 ) ;
#35040 =( BOUNDED_CURVE ( )  B_SPLINE_CURVE ( 3, ( #32742, #2446, #37115, #18085 ),
 .UNSPECIFIED., .F., .F. ) 
 B_SPLINE_CURVE_WITH_KNOTS ( ( 4, 4 ),
 ( 4.712388980384689674, 6.283185307179586232 ),
 .UNSPECIFIED. ) 
 CURVE ( )  GEOMETRIC_REPRESENTATION_ITEM ( )  RATIONAL_B_SPLINE_CURVE ( ( 1.000000000000000000, 0.8047378541243649375, 0.8047378541243649375, 1.000000000000000000 ) ) 
 REPRESENTATION_ITEM ( '' )  );
#35041 = DIRECTION ( 'NONE',  ( 1.000000000000000000, 0.000000000000000000, 0.000000000000000000 ) ) ;
#35042 = CARTESIAN_POINT ( 'NONE',  ( 10.00000000000000178, -46.01315789473684248, -25.00000000000000000 ) ) ;
#35043 = ORIENTED_EDGE ( 'NONE', *, *, #20620, .F. ) ;
#35044 = EDGE_CURVE ( 'NONE', #913, #32935, #22393, .T. ) ;
#35045 = DIRECTION ( 'NONE',  ( 0.000000000000000000, -1.000000000000000000, 0.000000000000000000 ) ) ;
#35046 =( BOUNDED_CURVE ( )  B_SPLINE_CURVE ( 3, ( #27391, #19688, #19932, #8660 ),
 .UNSPECIFIED., .F., .F. ) 
 B_SPLINE_CURVE_WITH_KNOTS ( ( 4, 4 ),
 ( 0.000000000000000000, 1.570796326794896558 ),
 .UNSPECIFIED. ) 
 CURVE ( )  GEOMETRIC_REPRESENTATION_ITEM ( )  RATIONAL_B_SPLINE_CURVE ( ( 1.000000000000000000, 0.8047378541243649375, 0.8047378541243649375, 1.000000000000000000 ) ) 
 REPRESENTATION_ITEM ( '' )  );
#35047 = CARTESIAN_POINT ( 'NONE',  ( -166.6959734468149463, 1.750000000000009992, -159.1817124430720298 ) ) ;
#35048 = ORIENTED_EDGE ( 'NONE', *, *, #12770, .T. ) ;
#35049 = CARTESIAN_POINT ( 'NONE',  ( 340.0000000000000568, 169.0000000000000000, 341.9999999999997726 ) ) ;
#35050 = ADVANCED_FACE ( 'NONE', ( #18536 ), #49294, .T. ) ;
#35051 = CARTESIAN_POINT ( 'NONE',  ( 356.0000000000001137, 183.0000000000000284, 357.9999999999998295 ) ) ;
#35052 = DIRECTION ( 'NONE',  ( 0.000000000000000000, -0.000000000000000000, -1.000000000000000000 ) ) ;
#35053 =( BOUNDED_CURVE ( )  B_SPLINE_CURVE ( 3, ( #42819, #12287, #46640, #46893 ),
 .UNSPECIFIED., .F., .F. ) 
 B_SPLINE_CURVE_WITH_KNOTS ( ( 4, 4 ),
 ( 3.141592653589793116, 4.712388980384689674 ),
 .UNSPECIFIED. ) 
 CURVE ( )  GEOMETRIC_REPRESENTATION_ITEM ( )  RATIONAL_B_SPLINE_CURVE ( ( 1.000000000000000000, 0.8047378541243649375, 0.8047378541243649375, 1.000000000000000000 ) ) 
 REPRESENTATION_ITEM ( '' )  );
#35054 = ORIENTED_EDGE ( 'NONE', *, *, #11810, .F. ) ;
#35055 = VERTEX_POINT ( 'NONE', #33709 ) ;
#35056 = CARTESIAN_POINT ( 'NONE',  ( 4.763548243873389154, -16.57409059453848599, 8.727788335465566760 ) ) ;
#35057 = EDGE_CURVE ( 'NONE', #16051, #36968, #26260, .T. ) ;
#35058 = EDGE_CURVE ( 'NONE', #45646, #41656, #25446, .T. ) ;
#35059 = VECTOR ( 'NONE', #46315, 1000.000000000000000 ) ;
#35060 = ORIENTED_EDGE ( 'NONE', *, *, #20555, .F. ) ;
#35061 = VERTEX_POINT ( 'NONE', #42645 ) ;
#35062 = CARTESIAN_POINT ( 'NONE',  ( -10.50000000000003375, 8.875661936878630698, 18.94832733001756253 ) ) ;
#35063 = FACE_OUTER_BOUND ( 'NONE', #20804, .T. ) ;
#35064 = CARTESIAN_POINT ( 'NONE',  ( 111.5540265531850679, 0.000000000000000000, 39.06828755692798438 ) ) ;
#35065 = EDGE_LOOP ( 'NONE', ( #22905, #39184, #8335, #28617 ) ) ;
#35066 = ORIENTED_EDGE ( 'NONE', *, *, #43521, .T. ) ;
#35067 = ORIENTED_EDGE ( 'NONE', *, *, #22515, .F. ) ;
#35068 = EDGE_CURVE ( 'NONE', #16975, #21335, #44734, .T. ) ;
#35069 = EDGE_CURVE ( 'NONE', #16655, #32283, #41896, .T. ) ;
#35070 = DIRECTION ( 'NONE',  ( 0.000000000000000000, 0.000000000000000000, 1.000000000000000000 ) ) ;
#35071 = ADVANCED_FACE ( 'NONE', ( #6744 ), #23198, .T. ) ;
#35072 = CARTESIAN_POINT ( 'NONE',  ( 15.00000000000000000, -46.51315789473684248, -5.916985404131818171 ) ) ;
#35073 = ORIENTED_EDGE ( 'NONE', *, *, #2670, .F. ) ;
#35074 = FACE_OUTER_BOUND ( 'NONE', #27341, .T. ) ;
#35075 = CARTESIAN_POINT ( 'NONE',  ( 344.0000000000000000, 175.0000000000000284, -106.0000000000001990 ) ) ;
#35076 = EDGE_LOOP ( 'NONE', ( #9792, #40416, #20917, #39657, #2971, #45417 ) ) ;
#35077 = VERTEX_POINT ( 'NONE', #30610 ) ;
#35078 = DIRECTION ( 'NONE',  ( -1.000000000000000000, -0.000000000000000000, -0.000000000000000000 ) ) ;
#35079 = DIRECTION ( 'NONE',  ( -1.000000000000000000, 0.000000000000000000, 0.000000000000000000 ) ) ;
#35080 = EDGE_CURVE ( 'NONE', #20716, #45083, #48028, .T. ) ;
#35081 = DIRECTION ( 'NONE',  ( 1.333906992743555050E-23, -1.000000000000000000, 0.000000000000000000 ) ) ;
#35082 = ORIENTED_EDGE ( 'NONE', *, *, #37740, .F. ) ;
#35083 = EDGE_LOOP ( 'NONE', ( #41205, #19749, #24136, #9265 ) ) ;
#35084 = CARTESIAN_POINT ( 'NONE',  ( -21.24469349090191983, 33.89193117067290473, 910.0000000000000000 ) ) ;
#35085 = DIRECTION ( 'NONE',  ( -0.000000000000000000, -0.000000000000000000, -1.000000000000000000 ) ) ;
#35086 = ORIENTED_EDGE ( 'NONE', *, *, #31746, .F. ) ;
#35087 = CARTESIAN_POINT ( 'NONE',  ( 115.0540265531850395, 2.143131898507847836E-16, 39.06828755692798438 ) ) ;
#35088 = DIRECTION ( 'NONE',  ( -1.000000000000000000, -0.000000000000000000, -0.000000000000000000 ) ) ;
#35089 = CARTESIAN_POINT ( 'NONE',  ( 0.9390173899407876501, 1.130417317737878458, 9.958264684458711713 ) ) ;
#35090 = CARTESIAN_POINT ( 'NONE',  ( -225.0000000000000568, -153.6999999999999602, 250.3600000000000136 ) ) ;
#35091 = ORIENTED_EDGE ( 'NONE', *, *, #16494, .F. ) ;
#35092 = CARTESIAN_POINT ( 'NONE',  ( 192.2789002873380184, -1.750000000000009548, -160.2068387089191219 ) ) ;
#35093 = FACE_OUTER_BOUND ( 'NONE', #24893, .T. ) ;
#35094 = CARTESIAN_POINT ( 'NONE',  ( 115.0540265531850395, 1.025126265847082108, 42.56828755692797017 ) ) ;
#35095 = CARTESIAN_POINT ( 'NONE',  ( -126.6959734468149321, 0.000000000000000000, 165.0000000000000000 ) ) ;
#35096 = VERTEX_POINT ( 'NONE', #46210 ) ;
#35097 = CARTESIAN_POINT ( 'NONE',  ( 8.813458710706171928, 4.724716452304571490, 0.000000000000000000 ) ) ;
#35098 = LINE ( 'NONE', #31238, #19275 ) ;
#35099 = DIRECTION ( 'NONE',  ( 0.000000000000000000, 0.000000000000000000, -1.000000000000000000 ) ) ;
#35100 = EDGE_CURVE ( 'NONE', #30729, #34658, #38282, .T. ) ;
#35101 = ORIENTED_EDGE ( 'NONE', *, *, #49014, .T. ) ;
#35102 = DIRECTION ( 'NONE',  ( -1.000000000000000000, -0.000000000000000000, -0.000000000000000000 ) ) ;
#35103 = CARTESIAN_POINT ( 'NONE',  ( 350.0000000000000000, -164.9999999999999432, -356.0000000000002274 ) ) ;
#35104 = ORIENTED_EDGE ( 'NONE', *, *, #18204, .T. ) ;
#35105 = DIRECTION ( 'NONE',  ( 1.000000000000000000, 0.000000000000000000, -0.000000000000000000 ) ) ;
#35106 = CARTESIAN_POINT ( 'NONE',  ( 5.951573025415589413, -0.3107723916541159093, 1.992221491942114397E-15 ) ) ;
#35107 = CARTESIAN_POINT ( 'NONE',  ( 224.9999999999999716, -164.9999999999999716, 32.29650858650035161 ) ) ;
#35108 = LINE ( 'NONE', #11237, #11077 ) ;
#35109 = VERTEX_POINT ( 'NONE', #32128 ) ;
#35110 = FACE_OUTER_BOUND ( 'NONE', #44359, .T. ) ;
#35111 = B_SPLINE_SURFACE_WITH_KNOTS ( 'NONE', 3, 3, ( 
 ( #36579, #4483, #904, #16546 ),
 ( #20130, #35821, #32199, #47798 ),
 ( #12683, #28344, #16796, #32458 ),
 ( #24499, #43975, #8843, #40148 ) ),
 .UNSPECIFIED., .F., .F., .F.,
 ( 4, 4 ),
 ( 4, 4 ),
 ( 0.000000000000000000, 1.000000000000000000 ),
 ( 0.000000000000000000, 1.000000000000000000 ),
 .UNSPECIFIED. ) ;
#35112 = B_SPLINE_CURVE_WITH_KNOTS ( 'NONE', 3,
 ( #2111, #17758, #33424, #48997 ),
 .UNSPECIFIED., .F., .F.,
 ( 4, 4 ),
 ( 0.0001535465953326577474, 0.0005837444810855837779 ),
 .UNSPECIFIED. ) ;
#35113 = ORIENTED_EDGE ( 'NONE', *, *, #25661, .F. ) ;
#35114 = ORIENTED_EDGE ( 'NONE', *, *, #42205, .T. ) ;
#35115 = CARTESIAN_POINT ( 'NONE',  ( -124.9459734468149463, 2.143131898507847836E-16, 42.56828755692795596 ) ) ;
#35116 = CARTESIAN_POINT ( 'NONE',  ( 194.3291528190321742, -1.750000000000009548, 121.8434138227750623 ) ) ;
#35117 = ADVANCED_FACE ( 'NONE', ( #4680 ), #47731, .F. ) ;
#35118 = ADVANCED_FACE ( 'NONE', ( #39585 ), #34990, .T. ) ;
#35119 = ORIENTED_EDGE ( 'NONE', *, *, #1775, .T. ) ;
#35120 = LINE ( 'NONE', #50172, #5751 ) ;
#35121 = CARTESIAN_POINT ( 'NONE',  ( -88.44597344681497475, 0.000000000000000000, 159.0682875569279418 ) ) ;
#35122 = CARTESIAN_POINT ( 'NONE',  ( 75.05402655318509630, -1.025126265847089657, 79.06828755692797017 ) ) ;
#35123 = VERTEX_POINT ( 'NONE', #39088 ) ;
#35125 = EDGE_CURVE ( 'NONE', #22517, #12712, #42494, .T. ) ;
#35124 = DIRECTION ( 'NONE',  ( -0.000000000000000000, -0.000000000000000000, -1.000000000000000000 ) ) ;
#35126 = CARTESIAN_POINT ( 'NONE',  ( 210.0000000000000568, 0.000000000000000000, 40.81828755692798438 ) ) ;
#35127 = EDGE_CURVE ( 'NONE', #47029, #7547, #77, .T. ) ;
#35128 = CARTESIAN_POINT ( 'NONE',  ( 114.3291528190321173, 1.749999999999996669, 159.7931612910809065 ) ) ;
#35129 = ORIENTED_EDGE ( 'NONE', *, *, #37535, .F. ) ;
#35130 = VECTOR ( 'NONE', #42437, 1000.000000000000000 ) ;
#35131 = CARTESIAN_POINT ( 'NONE',  ( 25.61277432017878297, -22.36370378792834757, 7.906207997025717304 ) ) ;
#35132 = CARTESIAN_POINT ( 'NONE',  ( 344.0000000000000568, 165.0000000000000000, 349.9999999999998295 ) ) ;
#35133 = ORIENTED_EDGE ( 'NONE', *, *, #34343, .T. ) ;
#35134 = ORIENTED_EDGE ( 'NONE', *, *, #45528, .T. ) ;
#35135 = ORIENTED_EDGE ( 'NONE', *, *, #43048, .T. ) ;
#35136 = CARTESIAN_POINT ( 'NONE',  ( 0.000000000000000000, -168.9999999999999432, -356.0000000000002274 ) ) ;
#35137 = EDGE_CURVE ( 'NONE', #14362, #38591, #8280, .T. ) ;
#35138 = CARTESIAN_POINT ( 'NONE',  ( 10.00000000000000000, -250.0000000000000000, -224.9999999999999716 ) ) ;
#35139 = EDGE_LOOP ( 'NONE', ( #31685, #3511, #31221, #30346 ) ) ;
#35140 = CLOSED_SHELL ( 'NONE', ( #42473, #4755, #30659, #40083, #4478, #34305, #3230, #33369, #32233, #29417, #24396, #6713, #41240, #168, #34060, #14773, #18463, #29047, #32437, #24969, #44815, #5357, #17551, #9374, #31181, #47314, #35853, #4811, #28684, #8650, #6, #38169, #7179, #739, #42452, #35242, #36909, #26807, #20205, #1579, #41007, #35892, #34865, #17837, #2325, #8401, #6828, #18640, #509, #42544, #27443, #5636, #47777, #629, #8965, #4412, #24106, #16573, #2628, #3652, #1158, #42276, #30234, #9259, #38133, #31159, #24101, #31503, #33101, #27998, #47782, #16157, #17376, #41639, #6761, #31304, #30575, #31479, #45563, #17884, #7183, #48991, #9655, #8067, #31770, #11073, #20198, #41505, #10455, #24448, #50032, #41701, #48784, #14746, #16702, #22153, #15645, #37749, #14093, #13585, #3559, #42589, #14041, #893, #13897, #42792, #35579 ) ) ;
#35141 = CARTESIAN_POINT ( 'NONE',  ( -177.4999999999999716, 74.83106485270648989, -130.5992382549688955 ) ) ;
#35142 = FACE_OUTER_BOUND ( 'NONE', #48625, .T. ) ;
#35143 = DIRECTION ( 'NONE',  ( 0.000000000000000000, 1.000000000000000000, 1.544785076050074834E-48 ) ) ;
#35144 = DIRECTION ( 'NONE',  ( -0.000000000000000000, -0.000000000000000000, -1.000000000000000000 ) ) ;
#35145 = CARTESIAN_POINT ( 'NONE',  ( 31.55402655318503236, -1.025126265847089657, -37.43171244307202272 ) ) ;
#35146 = LINE ( 'NONE', #11523, #11823 ) ;
#35147 = DIRECTION ( 'NONE',  ( 1.000000000000000000, 0.000000000000000000, 0.000000000000000000 ) ) ;
#35148 = CARTESIAN_POINT ( 'NONE',  ( -5.670847180967843570, 1.750000000000023315, -0.2068387089191201234 ) ) ;
#35149 = CARTESIAN_POINT ( 'NONE',  ( -168.4459734468149747, -1.025126265847089657, 119.0682875569279560 ) ) ;
#35150 = EDGE_LOOP ( 'NONE', ( #45725, #18340, #10742, #39932, #2312, #31398 ) ) ;
#35151 = DIRECTION ( 'NONE',  ( -1.000000000000000000, 0.000000000000000000, -2.958228394578794270E-31 ) ) ;
#35152 = CARTESIAN_POINT ( 'NONE',  ( -0.5113015165352315927, -1.175527691268679398, 9.948547179989621014 ) ) ;
#35153 = CARTESIAN_POINT ( 'NONE',  ( -126.6959734468149321, -1.749999999999997335, 120.8182875569279702 ) ) ;
#35154 = CARTESIAN_POINT ( 'NONE',  ( -0.9460392030597363222, -0.7922402054911648062, 9.969907203203806745 ) ) ;
#35155 = VERTEX_POINT ( 'NONE', #38829 ) ;
#35156 = CARTESIAN_POINT ( 'NONE',  ( -0.1469336902871204442, -1.496274467947957376, 9.953784399990622589 ) ) ;
#35157 = LINE ( 'NONE', #35910, #8127 ) ;
#35158 = DIRECTION ( 'NONE',  ( 0.000000000000000000, 0.000000000000000000, 1.000000000000000000 ) ) ;
#35159 = CARTESIAN_POINT ( 'NONE',  ( 15.44803555374680393, 6.237487519713364570, -3.546734833711462365 ) ) ;
#35160 = EDGE_CURVE ( 'NONE', #29819, #17812, #32822, .T. ) ;
#35161 = ORIENTED_EDGE ( 'NONE', *, *, #35044, .T. ) ;
#35162 = DIRECTION ( 'NONE',  ( 0.000000000000000000, 1.000000000000000000, 0.000000000000000000 ) ) ;
#35164 = ORIENTED_EDGE ( 'NONE', *, *, #20827, .F. ) ;
#35163 = CIRCLE ( 'NONE', #24526, 0.5000000000000004441 ) ;
#35165 = CARTESIAN_POINT ( 'NONE',  ( 0.1471466405374506625, 1.496299042407936319, 9.944962737436833677 ) ) ;
#35166 = ORIENTED_EDGE ( 'NONE', *, *, #49394, .F. ) ;
#35167 = VECTOR ( 'NONE', #49443, 1000.000000000000000 ) ;
#35168 = CARTESIAN_POINT ( 'NONE',  ( 358.0000000000000000, -168.9999999999999432, 343.9999999999998295 ) ) ;
#35169 = FACE_OUTER_BOUND ( 'NONE', #4238, .T. ) ;
#35170 = ORIENTED_EDGE ( 'NONE', *, *, #48539, .T. ) ;
#35171 = DIRECTION ( 'NONE',  ( 1.000000000000000000, 0.000000000000000000, 0.000000000000000000 ) ) ;
#35172 = CLOSED_SHELL ( 'NONE', ( #46829, #50030, #25242, #19088, #14224, #23466, #15357, #30019 ) ) ;
#35173 = ORIENTED_EDGE ( 'NONE', *, *, #22506, .F. ) ;
#35174 = AXIS2_PLACEMENT_3D ( 'NONE', #41691, #45513, #14493 ) ;
#35175 = ORIENTED_EDGE ( 'NONE', *, *, #48664, .T. ) ;
#35176 = CARTESIAN_POINT ( 'NONE',  ( 192.2789002873380184, 1.750000000000009548, 81.84341382277507648 ) ) ;
#35177 = DIRECTION ( 'NONE',  ( 8.673617379884028076E-17, -1.000000000000000000, -0.000000000000000000 ) ) ;
#35178 = EDGE_LOOP ( 'NONE', ( #32118, #42784, #25052, #39573 ) ) ;
#35179 = DIRECTION ( 'NONE',  ( -1.000000000000000000, 0.000000000000000000, 0.000000000000000000 ) ) ;
#35180 = CARTESIAN_POINT ( 'NONE',  ( -6.174150299305392053, 50.00000000000000000, 8.807470649214879543 ) ) ;
#35181 = CARTESIAN_POINT ( 'NONE',  ( -215.0000000000000568, -175.0000000000000000, 497.2965085865002379 ) ) ;
#35182 = ORIENTED_EDGE ( 'NONE', *, *, #4341, .T. ) ;
#35183 = DIRECTION ( 'NONE',  ( -0.000000000000000000, -1.000000000000000000, -0.000000000000000000 ) ) ;
#35184 = CARTESIAN_POINT ( 'NONE',  ( -225.0000000000000568, 164.9999999999999716, 231.9999999999999716 ) ) ;
#35185 = ORIENTED_EDGE ( 'NONE', *, *, #12452, .T. ) ;
#35186 = CARTESIAN_POINT ( 'NONE',  ( -1.142975459103954705, -16.61830776097024653, -2.870787844569587133 ) ) ;
#35187 = CARTESIAN_POINT ( 'NONE',  ( 85.00000000000090949, 17.00000000000000000, 0.000000000000000000 ) ) ;
#35188 = ORIENTED_EDGE ( 'NONE', *, *, #49601, .F. ) ;
#35189 = DIRECTION ( 'NONE',  ( 1.000000000000000000, 0.000000000000000000, -0.000000000000000000 ) ) ;
#35190 = EDGE_CURVE ( 'NONE', #40604, #46387, #5790, .T. ) ;
#35191 =( BOUNDED_CURVE ( )  B_SPLINE_CURVE ( 3, ( #18984, #46149, #25953, #30054 ),
 .UNSPECIFIED., .F., .F. ) 
 B_SPLINE_CURVE_WITH_KNOTS ( ( 4, 4 ),
 ( 0.000000000000000000, 1.570796326794896558 ),
 .UNSPECIFIED. ) 
 CURVE ( )  GEOMETRIC_REPRESENTATION_ITEM ( )  RATIONAL_B_SPLINE_CURVE ( ( 1.000000000000000000, 0.8047378541243649375, 0.8047378541243649375, 1.000000000000000000 ) ) 
 REPRESENTATION_ITEM ( '' )  );
#35192 = CARTESIAN_POINT ( 'NONE',  ( -69.99999999999783995, 17.00000000000000000, 115.0000000000000142 ) ) ;
#35193 = ORIENTED_EDGE ( 'NONE', *, *, #27163, .T. ) ;
#35194 = DIRECTION ( 'NONE',  ( -1.586032892321652236E-16, -1.000000000000000000, -2.288264760618012091E-48 ) ) ;
#35195 = CARTESIAN_POINT ( 'NONE',  ( -48.55374341718683695, -12.37034209168234256, -8.917361510505369182 ) ) ;
#35196 = PLANE ( 'NONE',  #4164 ) ;
#35197 = CARTESIAN_POINT ( 'NONE',  ( 75.05402655318509630, 2.143131898507880377E-16, -77.43171244307198720 ) ) ;
#35198 = AXIS2_PLACEMENT_3D ( 'NONE', #48532, #28326, #13174 ) ;
#35199 = ORIENTED_EDGE ( 'NONE', *, *, #45305, .F. ) ;
#35200 = CARTESIAN_POINT ( 'NONE',  ( -86.69597344681494633, 1.750000000000009992, -159.1817124430720298 ) ) ;
#35201 = AXIS2_PLACEMENT_3D ( 'NONE', #46425, #50002, #42849 ) ;
#35202 = CARTESIAN_POINT ( 'NONE',  ( -50.00000000000000000, 0.000000000000000000, 900.0000000000000000 ) ) ;
#35203 = AXIS2_PLACEMENT_3D ( 'NONE', #18142, #6603, #33817 ) ;
#35204 = DIRECTION ( 'NONE',  ( 0.000000000000000000, -0.9749645535258953943, -0.2223603367690637489 ) ) ;
#35205 = ORIENTED_EDGE ( 'NONE', *, *, #813, .T. ) ;
#35206 = EDGE_LOOP ( 'NONE', ( #15490, #21268, #6364, #31002 ) ) ;
#35208 = CARTESIAN_POINT ( 'NONE',  ( 33.30402655318503946, 1.750000000000010658, -119.1817124430720440 ) ) ;
#35207 = CIRCLE ( 'NONE', #13054, 4.000000000000003553 ) ;
#35209 = CYLINDRICAL_SURFACE ( 'NONE', #31621, 4.000000000000003553 ) ;
#35210 = SURFACE_SIDE_STYLE ('',( #7234 ) ) ;
#35211 = CARTESIAN_POINT ( 'NONE',  ( 4.999999999999999112, 175.0000000000000284, -346.2500000000002274 ) ) ;
#35212 = CARTESIAN_POINT ( 'NONE',  ( -1.011271242968693862, 0.7347315653655780432, -10.00000000000000000 ) ) ;
#35213 = ORIENTED_EDGE ( 'NONE', *, *, #7740, .T. ) ;
#35214 = CARTESIAN_POINT ( 'NONE',  ( 16.52264463346132572, -2.779753662172757878, 9.403735324607438884 ) ) ;
#35215 = DIRECTION ( 'NONE',  ( 0.000000000000000000, 0.000000000000000000, 1.000000000000000000 ) ) ;
#35216 = LINE ( 'NONE', #11854, #7803 ) ;
#35217 = VERTEX_POINT ( 'NONE', #3655 ) ;
#35218 =( NAMED_UNIT ( * ) PLANE_ANGLE_UNIT ( ) SI_UNIT ( $, .RADIAN. ) );
#35219 = ORIENTED_EDGE ( 'NONE', *, *, #17977, .F. ) ;
#35220 = CARTESIAN_POINT ( 'NONE',  ( 115.0540265531850395, 2.143131898507847836E-16, -160.9317124430720014 ) ) ;
#35221 = CARTESIAN_POINT ( 'NONE',  ( 7.749480817862238524, 14.85497772329518895, 9.403735324607438884 ) ) ;
#35222 = ORIENTED_EDGE ( 'NONE', *, *, #32557, .T. ) ;
#35223 = CARTESIAN_POINT ( 'NONE',  ( -5.670847180967843570, 1.750000000000023315, 41.84341382277508359 ) ) ;
#35224 = CARTESIAN_POINT ( 'NONE',  ( 7.359817328027030925, 15.16751262232805431, 2.590526750877053086 ) ) ;
#35225 = CARTESIAN_POINT ( 'NONE',  ( 1.011271242968694084, -0.7347315653655782652, -10.00000000000000000 ) ) ;
#35226 = CYLINDRICAL_SURFACE ( 'NONE', #34565, 1.750000000000010214 ) ;
#35227 = AXIS2_PLACEMENT_3D ( 'NONE', #17232, #21327, #32898 ) ;
#35228 = ORIENTED_EDGE ( 'NONE', *, *, #7694, .T. ) ;
#35229 = CIRCLE ( 'NONE', #49901, 4.000000000000003553 ) ;
#35230 = AXIS2_PLACEMENT_3D ( 'NONE', #128, #47537, #12417 ) ;
#35231 = CARTESIAN_POINT ( 'NONE',  ( 31.55402655318503236, 0.000000000000000000, 159.0682875569279702 ) ) ;
#35232 = CARTESIAN_POINT ( 'NONE',  ( -14.49999999999999822, 12.98684210526315930, -19.37312575500899570 ) ) ;
#35233 = ORIENTED_EDGE ( 'NONE', *, *, #31869, .T. ) ;
#35234 = DIRECTION ( 'NONE',  ( -1.000000000000000000, 0.000000000000000000, 0.000000000000000000 ) ) ;
#35235 = UNCERTAINTY_MEASURE_WITH_UNIT (LENGTH_MEASURE( 1.000000000000000082E-05 ), #32936, 'distance_accuracy_value', 'NONE');
#35236 = SPHERICAL_SURFACE ( 'NONE', #29944, 0.5000000000000000000 ) ;
#35237 = AXIS2_PLACEMENT_3D ( 'NONE', #25146, #48436, #39793 ) ;
#35238 = VERTEX_POINT ( 'NONE', #23665 ) ;
#35239 = ORIENTED_EDGE ( 'NONE', *, *, #36343, .T. ) ;
#35240 = CARTESIAN_POINT ( 'NONE',  ( -206.6959734468149463, -1.750000000000009992, 160.8182875569279702 ) ) ;
#35241 = VECTOR ( 'NONE', #25952, 1000.000000000000000 ) ;
#35242 = ADVANCED_FACE ( 'NONE', ( #27271 ), #3907, .T. ) ;
#35243 = EDGE_LOOP ( 'NONE', ( #50472, #25697, #45618, #45915 ) ) ;
#35244 = FACE_OUTER_BOUND ( 'NONE', #24675, .T. ) ;
#35245 = DIRECTION ( 'NONE',  ( 0.000000000000000000, 0.000000000000000000, 1.000000000000000000 ) ) ;
#35246 = VERTEX_POINT ( 'NONE', #8533 ) ;
#35247 = DIRECTION ( 'NONE',  ( 1.000000000000000000, 0.000000000000000000, 0.000000000000000000 ) ) ;
#35248 = EDGE_CURVE ( 'NONE', #36749, #39770, #8031, .T. ) ;
#35249 = ORIENTED_EDGE ( 'NONE', *, *, #15004, .F. ) ;
#35250 = CARTESIAN_POINT ( 'NONE',  ( -31.28234235046239320, -11.28615439405757392, -3.760136334089591248 ) ) ;
#35251 = EDGE_CURVE ( 'NONE', #50485, #34472, #42897, .T. ) ;
#35252 = DIRECTION ( 'NONE',  ( -1.000000000000000000, -0.000000000000000000, -0.000000000000000000 ) ) ;
#35253 = EDGE_CURVE ( 'NONE', #32679, #14457, #4172, .T. ) ;
#35254 = CARTESIAN_POINT ( 'NONE',  ( 342.0000000000000568, 169.0000000000000000, 343.9999999999998863 ) ) ;
#35255 = B_SPLINE_CURVE_WITH_KNOTS ( 'NONE', 3,
 ( #27468, #38771, #3597, #19241 ),
 .UNSPECIFIED., .F., .F.,
 ( 4, 4 ),
 ( 4.906538933386796626E-18, 0.002458791966311094177 ),
 .UNSPECIFIED. ) ;
#35256 = VERTEX_POINT ( 'NONE', #31117 ) ;
#35257 = VERTEX_POINT ( 'NONE', #27772 ) ;
#35258 = ORIENTED_EDGE ( 'NONE', *, *, #3941, .F. ) ;
#35259 = CARTESIAN_POINT ( 'NONE',  ( 153.3040265531850537, -1.750000000000010658, -79.18171244307201562 ) ) ;
#35260 = PRESENTATION_STYLE_ASSIGNMENT (( #34758 ) ) ;
#35261 = B_SPLINE_CURVE_WITH_KNOTS ( 'NONE', 3,
 ( #37931, #29966, #17887, #46069 ),
 .UNSPECIFIED., .F., .F.,
 ( 4, 4 ),
 ( 1.735570302229820823E-18, 2.804146970186932944E-05 ),
 .UNSPECIFIED. ) ;
#35262 = DIRECTION ( 'NONE',  ( 0.000000000000000000, -1.000000000000000000, -1.544785076050074834E-48 ) ) ;
#35263 = EDGE_CURVE ( 'NONE', #6656, #24412, #11035, .T. ) ;
#35264 = ORIENTED_EDGE ( 'NONE', *, *, #22690, .T. ) ;
#35265 = DIRECTION ( 'NONE',  ( 1.000000000000000000, -1.586032892321652236E-16, -9.711650524620651178E-33 ) ) ;
#35267 = ORIENTED_EDGE ( 'NONE', *, *, #17701, .T. ) ;
#35266 = VECTOR ( 'NONE', #5810, 1000.000000000000000 ) ;
#35268 = CARTESIAN_POINT ( 'NONE',  ( -177.4999999999999716, -112.5000000000000000, 0.000000000000000000 ) ) ;
#35270 = EDGE_LOOP ( 'NONE', ( #44255, #42515, #37261, #18525, #18498, #25615 ) ) ;
#35269 = VECTOR ( 'NONE', #15453, 1000.000000000000000 ) ;
#35271 = PLANE ( 'NONE',  #48210 ) ;
#35272 = DIRECTION ( 'NONE',  ( -1.110223024625156171E-16, 0.7071067811865474617, -0.7071067811865474617 ) ) ;
#35273 = DIRECTION ( 'NONE',  ( -0.000000000000000000, -0.000000000000000000, -1.000000000000000000 ) ) ;
#35274 = AXIS2_PLACEMENT_3D ( 'NONE', #24676, #5411, #9765 ) ;
#35275 = SHAPE_REPRESENTATION ( 'tire holder', ( #45486 ), #13533 ) ;
#35276 = FACE_OUTER_BOUND ( 'NONE', #50060, .T. ) ;
#35277 = EDGE_LOOP ( 'NONE', ( #48033, #39630, #43639, #42712 ) ) ;
#35278 = ORIENTED_EDGE ( 'NONE', *, *, #29294, .F. ) ;
#35280 = CIRCLE ( 'NONE', #4128, 2.000000000000001776 ) ;
#35279 = CARTESIAN_POINT ( 'NONE',  ( -36.08557433729204433, 35.58569447144795106, 7.455576670931136185 ) ) ;
#35281 = CIRCLE ( 'NONE', #40377, 4.000000000000003553 ) ;
#35282 = DIRECTION ( 'NONE',  ( 0.000000000000000000, 0.000000000000000000, -1.000000000000000000 ) ) ;
#35283 = CARTESIAN_POINT ( 'NONE',  ( -47.87295225382221275, -14.46560184742400423, -2.408242355805840784 ) ) ;
#35284 = EDGE_CURVE ( 'NONE', #30177, #41895, #50560, .T. ) ;
#35285 = ADVANCED_FACE ( 'NONE', ( #2090 ), #32636, .T. ) ;
#35286 = VECTOR ( 'NONE', #9716, 1000.000000000000000 ) ;
#35287 = EDGE_CURVE ( 'NONE', #26079, #27650, #32381, .T. ) ;
#35288 = EDGE_CURVE ( 'NONE', #26701, #11387, #8788, .T. ) ;
#35289 = LINE ( 'NONE', #50354, #40342 ) ;
#35290 = DIRECTION ( 'NONE',  ( 0.000000000000000000, 0.000000000000000000, 1.000000000000000000 ) ) ;
#35291 = EDGE_CURVE ( 'NONE', #48865, #37507, #26777, .T. ) ;
#35292 = ORIENTED_EDGE ( 'NONE', *, *, #1487, .F. ) ;
#35293 = CARTESIAN_POINT ( 'NONE',  ( -0.1469336902871204442, -1.496274467947957376, 9.953784399990622589 ) ) ;
#35294 = EDGE_CURVE ( 'NONE', #30988, #32259, #15650, .T. ) ;
#35295 = CYLINDRICAL_SURFACE ( 'NONE', #38608, 2.000000000000001776 ) ;
#35296 = ORIENTED_EDGE ( 'NONE', *, *, #36928, .F. ) ;
#35297 = DIRECTION ( 'NONE',  ( -1.000000000000000000, 0.000000000000000000, 0.000000000000000000 ) ) ;
#35298 = CARTESIAN_POINT ( 'NONE',  ( -126.6959734468149321, 1.749999999999997113, 40.81828755692798438 ) ) ;
#35299 = CYLINDRICAL_SURFACE ( 'NONE', #27496, 1.750000000000015543 ) ;
#35300 = ORIENTED_EDGE ( 'NONE', *, *, #10867, .F. ) ;
#35301 = VERTEX_POINT ( 'NONE', #5671 ) ;
#35302 = EDGE_CURVE ( 'NONE', #39140, #34485, #37880, .T. ) ;
#35303 = FACE_OUTER_BOUND ( 'NONE', #22146, .T. ) ;
#35304 = CARTESIAN_POINT ( 'NONE',  ( 0.000000000000000000, 181.0000000000000284, 343.9999999999997726 ) ) ;
#35305 = CIRCLE ( 'NONE', #32845, 0.5000000000000004441 ) ;
#35306 = VECTOR ( 'NONE', #49979, 1000.000000000000000 ) ;
#35307 = EDGE_CURVE ( 'NONE', #40207, #24013, #7375, .T. ) ;
#35308 = ORIENTED_EDGE ( 'NONE', *, *, #2321, .F. ) ;
#35309 = ADVANCED_FACE ( 'NONE', ( #1082 ), #16980, .F. ) ;
#35310 = ORIENTED_EDGE ( 'NONE', *, *, #44466, .F. ) ;
#35311 = CARTESIAN_POINT ( 'NONE',  ( 195.0540265531851105, -1.025126265847088991, -157.4317124430720582 ) ) ;
#35312 = DIRECTION ( 'NONE',  ( -1.000000000000000000, -0.000000000000000000, -0.000000000000000000 ) ) ;
#35313 = CARTESIAN_POINT ( 'NONE',  ( -7.576114424932982594, 50.00000000000000711, 7.906207997025717304 ) ) ;
#35314 = CARTESIAN_POINT ( 'NONE',  ( -164.9459734468149463, 1.025126265847089879, 82.56828755692798438 ) ) ;
#35315 = VERTEX_POINT ( 'NONE', #16722 ) ;
#35316 = EDGE_LOOP ( 'NONE', ( #7412, #48467, #30545, #31806 ) ) ;
#35317 = ORIENTED_EDGE ( 'NONE', *, *, #29133, .F. ) ;
#35318 = AXIS2_PLACEMENT_3D ( 'NONE', #28109, #23508, #39663 ) ;
#35319 = AXIS2_PLACEMENT_3D ( 'NONE', #37001, #9262, #16701 ) ;
#35320 = EDGE_CURVE ( 'NONE', #16290, #50318, #9280, .T. ) ;
#35321 = CARTESIAN_POINT ( 'NONE',  ( -7.721099712662037540, -1.750000000000023537, 121.8434138227750623 ) ) ;
#35322 = DIRECTION ( 'NONE',  ( -1.000000000000000000, -0.000000000000000000, -0.000000000000000000 ) ) ;
#35323 = ORIENTED_EDGE ( 'NONE', *, *, #33711, .T. ) ;
#35324 = CARTESIAN_POINT ( 'NONE',  ( 1.080000014128428498, 0.7606467978644730898, 9.943883492372853183 ) ) ;
#35325 = PLANE ( 'NONE',  #30708 ) ;
#35326 = VERTEX_POINT ( 'NONE', #25181 ) ;
#35327 = ORIENTED_EDGE ( 'NONE', *, *, #1502, .T. ) ;
#35328 = DIRECTION ( 'NONE',  ( 0.000000000000000000, 0.000000000000000000, 1.000000000000000000 ) ) ;
#35329 = CARTESIAN_POINT ( 'NONE',  ( -47.72109971266203132, 1.750000000000009548, 159.7931612910809065 ) ) ;
#35330 = CARTESIAN_POINT ( 'NONE',  ( 194.9999999999999432, 173.0000000000000000, 252.0000000000000000 ) ) ;
#35331 = UNCERTAINTY_MEASURE_WITH_UNIT (LENGTH_MEASURE( 1.000000000000000082E-05 ), #46966, 'distance_accuracy_value', 'NONE');
#35332 = VERTEX_POINT ( 'NONE', #37015 ) ;
#35333 = ORIENTED_EDGE ( 'NONE', *, *, #43824, .F. ) ;
#35334 = EDGE_CURVE ( 'NONE', #23855, #40582, #47705, .T. ) ;
#35335 = CARTESIAN_POINT ( 'NONE',  ( -0.3862712429686809279, -1.188820645368943163, 10.00000000000000000 ) ) ;
#35336 = DIRECTION ( 'NONE',  ( 1.000000000000000000, 0.000000000000000000, 0.000000000000000000 ) ) ;
#35337 = VERTEX_POINT ( 'NONE', #5170 ) ;
#35338 =( BOUNDED_CURVE ( )  B_SPLINE_CURVE ( 3, ( #48648, #48901, #5081, #44561 ),
 .UNSPECIFIED., .F., .F. ) 
 B_SPLINE_CURVE_WITH_KNOTS ( ( 4, 4 ),
 ( 0.000000000000000000, 1.570796326794896780 ),
 .UNSPECIFIED. ) 
 CURVE ( )  GEOMETRIC_REPRESENTATION_ITEM ( )  RATIONAL_B_SPLINE_CURVE ( ( 1.000000000000000000, 0.8047378541243649375, 0.8047378541243649375, 1.000000000000000000 ) ) 
 REPRESENTATION_ITEM ( '' )  );
#35339 = DIRECTION ( 'NONE',  ( 1.000000000000000000, 0.000000000000000000, -0.000000000000000000 ) ) ;
#35340 = DIRECTION ( 'NONE',  ( 1.000000000000000000, 0.000000000000000000, 0.000000000000000000 ) ) ;
#35341 = CARTESIAN_POINT ( 'NONE',  ( 2.500000000000000444, 224.9999999999999716, -240.0000000000000000 ) ) ;
#35342 = EDGE_CURVE ( 'NONE', #9162, #47457, #5420, .T. ) ;
#35343 = LINE ( 'NONE', #15813, #8529 ) ;
#35344 = VERTEX_POINT ( 'NONE', #1338 ) ;
#35345 = DIRECTION ( 'NONE',  ( 1.000000000000000000, 0.000000000000000000, 0.000000000000000000 ) ) ;
#35346 =( BOUNDED_CURVE ( )  B_SPLINE_CURVE ( 3, ( #32515, #41188, #40192, #6043 ),
 .UNSPECIFIED., .F., .F. ) 
 B_SPLINE_CURVE_WITH_KNOTS ( ( 4, 4 ),
 ( 3.141592653589793116, 4.712388980384689674 ),
 .UNSPECIFIED. ) 
 CURVE ( )  GEOMETRIC_REPRESENTATION_ITEM ( )  RATIONAL_B_SPLINE_CURVE ( ( 1.000000000000000000, 0.8047378541243649375, 0.8047378541243649375, 1.000000000000000000 ) ) 
 REPRESENTATION_ITEM ( '' )  );
#35347 = CARTESIAN_POINT ( 'NONE',  ( 210.0000000000000568, 0.000000000000000000, 160.8182875569279702 ) ) ;
#35348 = CARTESIAN_POINT ( 'NONE',  ( -325.0507910275983932, -325.0507910275983932, 321.8002831173224649 ) ) ;
#35349 = AXIS2_PLACEMENT_3D ( 'NONE', #41905, #30886, #6751 ) ;
#35350 = LINE ( 'NONE', #43767, #47591 ) ;
#35351 = EDGE_CURVE ( 'NONE', #3258, #41868, #24938, .T. ) ;
#35352 = ADVANCED_FACE ( 'NONE', ( #13626 ), #1586, .T. ) ;
#35353 = ORIENTED_EDGE ( 'NONE', *, *, #43560, .T. ) ;
#35354 = CARTESIAN_POINT ( 'NONE',  ( 194.3291528190321742, -1.750000000000009548, -0.2068387089191121020 ) ) ;
#35355 = EDGE_CURVE ( 'NONE', #26029, #22310, #48478, .T. ) ;
#35356 = DIRECTION ( 'NONE',  ( -0.000000000000000000, -0.000000000000000000, -1.000000000000000000 ) ) ;
#35357 = CIRCLE ( 'NONE', #26319, 50.00000000000000000 ) ;
#35358 = CARTESIAN_POINT ( 'NONE',  ( 193.3040265531851105, 1.750000000000009992, -159.1817124430720298 ) ) ;
#35359 = EDGE_CURVE ( 'NONE', #9213, #9513, #44647, .T. ) ;
#35360 = ADVANCED_FACE ( 'NONE', ( #42336 ), #26434, .F. ) ;
#35361 = ORIENTED_EDGE ( 'NONE', *, *, #9924, .T. ) ;
#35362 = PLANE ( 'NONE',  #5975 ) ;
#35363 = DIRECTION ( 'NONE',  ( 0.000000000000000000, 0.000000000000000000, 1.000000000000000000 ) ) ;
#35364 = ORIENTED_EDGE ( 'NONE', *, *, #35984, .T. ) ;
#35365 = CARTESIAN_POINT ( 'NONE',  ( 181.0000000000000000, -5.999999999999950262, -340.0000000000001137 ) ) ;
#35366 = FACE_OUTER_BOUND ( 'NONE', #12132, .T. ) ;
#35367 = DIRECTION ( 'NONE',  ( 1.000000000000000000, 0.000000000000000000, 0.000000000000000000 ) ) ;
#35368 = ORIENTED_EDGE ( 'NONE', *, *, #46516, .T. ) ;
#35369 = PLANE ( 'NONE',  #33927 ) ;
#35370 = ORIENTED_EDGE ( 'NONE', *, *, #22353, .T. ) ;
#35371 = EDGE_LOOP ( 'NONE', ( #43978, #11186, #2573, #16923 ) ) ;
#35372 = LINE ( 'NONE', #16345, #15251 ) ;
#35373 = CARTESIAN_POINT ( 'NONE',  ( 195.9526953830863079, -153.9383703589661820, 472.5992458228020610 ) ) ;
#35374 = EDGE_LOOP ( 'NONE', ( #43197, #44535, #38575, #30081 ) ) ;
#35375 = EDGE_CURVE ( 'NONE', #418, #13598, #30546, .T. ) ;
#35376 = DIRECTION ( 'NONE',  ( 1.000000000000000000, 0.000000000000000000, 0.000000000000000000 ) ) ;
#35377 = LINE ( 'NONE', #24065, #31476 ) ;
#35378 = B_SPLINE_CURVE_WITH_KNOTS ( 'NONE', 3,
 ( #40069, #13101, #12853, #25417 ),
 .UNSPECIFIED., .F., .F.,
 ( 4, 4 ),
 ( 0.9895749839358300992, 1.000000000000000000 ),
 .UNSPECIFIED. ) ;
#35379 = CARTESIAN_POINT ( 'NONE',  ( 151.5540265531850537, 0.000000000000000000, 165.0000000000000000 ) ) ;
#35380 = ORIENTED_EDGE ( 'NONE', *, *, #12101, .T. ) ;
#35381 = LINE ( 'NONE', #27916, #29916 ) ;
#35382 = FACE_OUTER_BOUND ( 'NONE', #11987, .T. ) ;
#35383 = DIRECTION ( 'NONE',  ( -0.000000000000000000, -0.000000000000000000, 1.000000000000000000 ) ) ;
#35384 = ORIENTED_EDGE ( 'NONE', *, *, #583, .T. ) ;
#35385 = CARTESIAN_POINT ( 'NONE',  ( 210.0000000000000568, 0.000000000000000000, 120.8182875569279702 ) ) ;
#35386 = DIRECTION ( 'NONE',  ( -1.000000000000000000, 0.000000000000000000, 0.000000000000000000 ) ) ;
#35387 = EDGE_LOOP ( 'NONE', ( #44462, #3203, #9356, #8960, #2174, #8807 ) ) ;
#35388 = VERTEX_POINT ( 'NONE', #29530 ) ;
#35389 = ORIENTED_EDGE ( 'NONE', *, *, #15214, .T. ) ;
#35390 = CARTESIAN_POINT ( 'NONE',  ( 12.16428377685533135, 11.73151505502934988, -9.008049429158100807 ) ) ;
#35391 = CARTESIAN_POINT ( 'NONE',  ( 35.05402655318504657, -1.025126265847089657, 119.0682875569279560 ) ) ;
#35392 = VECTOR ( 'NONE', #50039, 1000.000000000000000 ) ;
#35393 = VERTEX_POINT ( 'NONE', #29789 ) ;
#35394 = CARTESIAN_POINT ( 'NONE',  ( -12.15085308559838317, 11.68662139125813226, 2.590526750877053086 ) ) ;
#35395 = DIRECTION ( 'NONE',  ( 0.000000000000000000, -1.000000000000000000, 0.000000000000000000 ) ) ;
#35396 = DIRECTION ( 'NONE',  ( -1.000000000000000000, 0.000000000000000000, 0.000000000000000000 ) ) ;
#35397 = CARTESIAN_POINT ( 'NONE',  ( 33.30402655318503946, -1.750000000000010658, -79.18171244307201562 ) ) ;
#35398 = CARTESIAN_POINT ( 'NONE',  ( 35.05402655318504657, 1.025126265847089213, -160.9317124430720014 ) ) ;
#35399 = CARTESIAN_POINT ( 'NONE',  ( 153.3040265531850537, -1.750000000000010658, 80.81828755692798438 ) ) ;
#35400 = CARTESIAN_POINT ( 'NONE',  ( -166.6959734468149463, 1.750000000000010658, -79.18171244307201562 ) ) ;
#35401 = CARTESIAN_POINT ( 'NONE',  ( 1.760168014277346593, 0.8403809255487892926, 9.896382706792421047 ) ) ;
#35402 = CYLINDRICAL_SURFACE ( 'NONE', #40415, 1.750000000000015543 ) ;
#35403 = CARTESIAN_POINT ( 'NONE',  ( 0.9602803029231544718, -0.8490247040095941777, 9.976582533991681601 ) ) ;
#35404 = CARTESIAN_POINT ( 'NONE',  ( -126.6959734468149321, 1.749999999999997113, 40.81828755692798438 ) ) ;
#35405 = EDGE_CURVE ( 'NONE', #36298, #5197, #22836, .T. ) ;
#35406 = EDGE_CURVE ( 'NONE', #44300, #42814, #2574, .T. ) ;
#35407 = DIRECTION ( 'NONE',  ( -0.000000000000000000, 1.000000000000000000, 0.000000000000000000 ) ) ;
#35408 = DIRECTION ( 'NONE',  ( 1.000000000000000000, 0.000000000000000000, 0.000000000000000000 ) ) ;
#35409 = EDGE_LOOP ( 'NONE', ( #391, #40203, #12082, #43159 ) ) ;
#35410 = CARTESIAN_POINT ( 'NONE',  ( -127.7210997126620242, 1.749999999999997113, -80.20683870891909351 ) ) ;
#35411 = AXIS2_PLACEMENT_3D ( 'NONE', #35716, #11579, #1043 ) ;
#35412 = ADVANCED_FACE ( 'NONE', ( #49737 ), #46145, .T. ) ;
#35413 = DIRECTION ( 'NONE',  ( 0.000000000000000000, 0.000000000000000000, -1.000000000000000000 ) ) ;
#35414 = CARTESIAN_POINT ( 'NONE',  ( 194.3291528190321742, -1.750000000000010436, -120.2068387089191219 ) ) ;
#35415 = CARTESIAN_POINT ( 'NONE',  ( 210.0000000000000568, 2.143131898507881116E-16, 39.06828755692797728 ) ) ;
#35416 = EDGE_CURVE ( 'NONE', #6557, #49797, #48307, .T. ) ;
#35417 = EDGE_CURVE ( 'NONE', #8857, #35947, #28727, .T. ) ;
#35418 = EDGE_LOOP ( 'NONE', ( #41591, #5111, #21830, #24756 ) ) ;
#35419 = CARTESIAN_POINT ( 'NONE',  ( 35.05402655318504657, 2.143131898507880377E-16, 165.0000000000000000 ) ) ;
#35420 = EDGE_LOOP ( 'NONE', ( #12600, #38094, #38238, #35327, #41378, #26437 ) ) ;
#35421 = VECTOR ( 'NONE', #40632, 1000.000000000000000 ) ;
#35422 = CARTESIAN_POINT ( 'NONE',  ( 0.1473596192803392213, 1.496323530725627515, 9.936141075511205401 ) ) ;
#35423 = ORIENTED_EDGE ( 'NONE', *, *, #33426, .T. ) ;
#35424 = FACE_OUTER_BOUND ( 'NONE', #17420, .T. ) ;
#35425 = DIRECTION ( 'NONE',  ( -0.000000000000000000, -0.000000000000000000, -1.000000000000000000 ) ) ;
#35426 = EDGE_CURVE ( 'NONE', #3803, #30626, #3078, .T. ) ;
#35427 = VERTEX_POINT ( 'NONE', #45903 ) ;
#35428 = CARTESIAN_POINT ( 'NONE',  ( 32.92553608936638199, 17.96298651181805894, 8.100132398494515940 ) ) ;
#35429 = ORIENTED_EDGE ( 'NONE', *, *, #26014, .T. ) ;
#35430 = ORIENTED_EDGE ( 'NONE', *, *, #7601, .T. ) ;
#35431 = DIRECTION ( 'NONE',  ( 0.000000000000000000, 0.000000000000000000, 1.000000000000000000 ) ) ;
#35432 = DIRECTION ( 'NONE',  ( -0.000000000000000000, -0.000000000000000000, -1.000000000000000000 ) ) ;
#35433 = ORIENTED_EDGE ( 'NONE', *, *, #36676, .F. ) ;
#35434 = CARTESIAN_POINT ( 'NONE',  ( 181.0000000000000000, -272.5000000000000000, -114.9999999999999147 ) ) ;
#35435 = CARTESIAN_POINT ( 'NONE',  ( 111.5540265531850679, 0.000000000000000000, -0.9317124430719969652 ) ) ;
#35436 = CARTESIAN_POINT ( 'NONE',  ( -50.00000000000000000, -50.00000000000000000, 900.0000000000000000 ) ) ;
#35437 = ORIENTED_EDGE ( 'NONE', *, *, #50333, .F. ) ;
#35438 = DIRECTION ( 'NONE',  ( -1.000000000000000000, -0.000000000000000000, -0.000000000000000000 ) ) ;
#35439 = DIRECTION ( 'NONE',  ( 1.000000000000000000, 0.000000000000000000, 0.000000000000000000 ) ) ;
#35440 = ORIENTED_EDGE ( 'NONE', *, *, #19340, .T. ) ;
#35441 = CARTESIAN_POINT ( 'NONE',  ( 2.569099690548740877, -50.00000000000000711, 3.199614146704519602 ) ) ;
#35442 = PLANE ( 'NONE',  #31904 ) ;
#35443=STYLED_ITEM('',(#50761),#5361);
#35444 = ORIENTED_EDGE ( 'NONE', *, *, #22115, .F. ) ;
#35445 = LINE ( 'NONE', #4377, #14741 ) ;
#35446 = AXIS2_PLACEMENT_3D ( 'NONE', #41615, #24970, #1619 ) ;
#35447 = CARTESIAN_POINT ( 'NONE',  ( 0.000000000000000000, -166.9999999999999432, -356.0000000000002274 ) ) ;
#35448 = ORIENTED_EDGE ( 'NONE', *, *, #39743, .F. ) ;
#35450 = EDGE_CURVE ( 'NONE', #13304, #43357, #34165, .T. ) ;
#35449 = VECTOR ( 'NONE', #15508, 1000.000000000000000 ) ;
#35451 = DIRECTION ( 'NONE',  ( 0.000000000000000000, 1.000000000000000000, 0.000000000000000000 ) ) ;
#35452 = LINE ( 'NONE', #15423, #48662 ) ;
#35453 = CARTESIAN_POINT ( 'NONE',  ( 5.551115123125782702E-14, -182.9999999999999716, 355.9999999999997726 ) ) ;
#35454 = CARTESIAN_POINT ( 'NONE',  ( 73.30402655318508209, -1.750000000000010658, -119.1817124430720440 ) ) ;
#35455 = AXIS2_PLACEMENT_3D ( 'NONE', #9721, #40283, #25139 ) ;
#35456 = ORIENTED_EDGE ( 'NONE', *, *, #40853, .T. ) ;
#35457 = CARTESIAN_POINT ( 'NONE',  ( 30.87089393895375267, -12.69923079256617449, -9.367992836599954742 ) ) ;
#35458 = DIRECTION ( 'NONE',  ( 0.7233555441435721711, 0.6904757466825004464, 0.000000000000000000 ) ) ;
#35459 = DIRECTION ( 'NONE',  ( -1.000000000000000000, -0.000000000000000000, -0.000000000000000000 ) ) ;
#35460 = EDGE_LOOP ( 'NONE', ( #13932, #7064 ) ) ;
#35461 = ORIENTED_EDGE ( 'NONE', *, *, #4340, .T. ) ;
#35462 = APPLICATION_PROTOCOL_DEFINITION ( 'draft international standard', 'automotive_design', 1998, #13525 ) ;
#35463 = DIRECTION ( 'NONE',  ( 1.000000000000000000, 0.000000000000000000, 0.000000000000000000 ) ) ;
#35464 = CARTESIAN_POINT ( 'NONE',  ( -1.249999999999999778, 0.000000000000000000, 10.00000000000000000 ) ) ;
#35465 = CARTESIAN_POINT ( 'NONE',  ( 210.0000000000000568, 0.000000000000000000, 42.56828755692799149 ) ) ;
#35466 = ORIENTED_EDGE ( 'NONE', *, *, #32419, .T. ) ;
#35467 = CARTESIAN_POINT ( 'NONE',  ( 341.6568542494921417, -185.0000000000000568, 359.9999999999998295 ) ) ;
#35468 = VECTOR ( 'NONE', #9606, 1000.000000000000000 ) ;
#35469 = LINE ( 'NONE', #35734, #4833 ) ;
#35470 = DIRECTION ( 'NONE',  ( 0.000000000000000000, 0.000000000000000000, 1.000000000000000000 ) ) ;
#35471 = DIRECTION ( 'NONE',  ( -0.000000000000000000, -0.000000000000000000, -1.000000000000000000 ) ) ;
#35472 = VERTEX_POINT ( 'NONE', #14893 ) ;
#35473 = CARTESIAN_POINT ( 'NONE',  ( 113.3040265531850537, 1.749999999999997335, -119.1817124430720440 ) ) ;
#35474 = ORIENTED_EDGE ( 'NONE', *, *, #15577, .F. ) ;
#35475 = PLANE ( 'NONE',  #6487 ) ;
#35476 = ORIENTED_EDGE ( 'NONE', *, *, #44717, .T. ) ;
#35477 = EDGE_CURVE ( 'NONE', #44889, #8314, #2200, .T. ) ;
#35478 = CARTESIAN_POINT ( 'NONE',  ( -7.129058724845069861, -15.30620660340479766, 9.178419661560148768 ) ) ;
#35479 = VECTOR ( 'NONE', #35459, 1000.000000000000000 ) ;
#35480 = FACE_OUTER_BOUND ( 'NONE', #45737, .T. ) ;
#35481 = LINE ( 'NONE', #22892, #14886 ) ;
#35482 = ORIENTED_EDGE ( 'NONE', *, *, #7810, .F. ) ;
#35483=STYLED_ITEM('',(#50747),#38632);
#35484 = DIRECTION ( 'NONE',  ( 0.000000000000000000, -1.822804496942679766E-16, -1.000000000000000000 ) ) ;
#35485 = AXIS2_PLACEMENT_3D ( 'NONE', #6470, #41626, #17521 ) ;
#35486 = CARTESIAN_POINT ( 'NONE',  ( 358.3431457505075741, 185.0000000000001990, -360.0000000000003411 ) ) ;
#35487 = ORIENTED_EDGE ( 'NONE', *, *, #13316, .T. ) ;
#35488 = CARTESIAN_POINT ( 'NONE',  ( 181.0000000000000000, -168.9999999999999432, -350.0000000000001705 ) ) ;
#35489 = DIRECTION ( 'NONE',  ( 0.000000000000000000, 0.000000000000000000, 1.000000000000000000 ) ) ;
#35490 = DIRECTION ( 'NONE',  ( 0.000000000000000000, 0.9230769230769231282, 0.3846153846153844702 ) ) ;
#35491 = LINE ( 'NONE', #24441, #40608 ) ;
#35492 =( BOUNDED_CURVE ( )  B_SPLINE_CURVE ( 3, ( #44228, #911, #40154, #39411 ),
 .UNSPECIFIED., .F., .F. ) 
 B_SPLINE_CURVE_WITH_KNOTS ( ( 4, 4 ),
 ( 0.000000000000000000, 1.570796326794896780 ),
 .UNSPECIFIED. ) 
 CURVE ( )  GEOMETRIC_REPRESENTATION_ITEM ( )  RATIONAL_B_SPLINE_CURVE ( ( 1.000000000000000000, 0.8047378541243649375, 0.8047378541243649375, 1.000000000000000000 ) ) 
 REPRESENTATION_ITEM ( '' )  );
#35493 = VERTEX_POINT ( 'NONE', #25691 ) ;
#35494 = VERTEX_POINT ( 'NONE', #10784 ) ;
#35495 = CARTESIAN_POINT ( 'NONE',  ( 154.3291528190321458, 1.750000000000009548, -40.20683870891912193 ) ) ;
#35496 = ORIENTED_EDGE ( 'NONE', *, *, #9545, .F. ) ;
#35497 = DIRECTION ( 'NONE',  ( -1.000000000000000000, -0.000000000000000000, -0.000000000000000000 ) ) ;
#35498 = CARTESIAN_POINT ( 'NONE',  ( -165.6708471809677974, -1.750000000000009548, 39.79316129108089228 ) ) ;
#35499 = AXIS2_PLACEMENT_3D ( 'NONE', #12459, #50406, #16319 ) ;
#35500 = LINE ( 'NONE', #47991, #42827 ) ;
#35501 = VERTEX_POINT ( 'NONE', #26698 ) ;
#35502 = LINE ( 'NONE', #8045, #44806 ) ;
#35503 = ORIENTED_EDGE ( 'NONE', *, *, #13180, .F. ) ;
#35504 = CARTESIAN_POINT ( 'NONE',  ( -119.9999999999978400, 17.00000000000000000, 95.00000000000000000 ) ) ;
#35505 = EDGE_CURVE ( 'NONE', #32969, #19150, #7198, .T. ) ;
#35506 = LINE ( 'NONE', #27790, #7059 ) ;
#35507 = CARTESIAN_POINT ( 'NONE',  ( -1.249999999999999778, 0.000000000000000000, 3.333333333333333481 ) ) ;
#35508 = VERTEX_POINT ( 'NONE', #14385 ) ;
#35509 = EDGE_LOOP ( 'NONE', ( #29539, #32911 ) ) ;
#35510 = AXIS2_PLACEMENT_3D ( 'NONE', #5292, #42898, #26059 ) ;
#35511 = APPLICATION_CONTEXT ( 'automotive_design' ) ;
#35512 = ORIENTED_EDGE ( 'NONE', *, *, #7105, .T. ) ;
#35513 = CARTESIAN_POINT ( 'NONE',  ( 164.9999999999999716, 17.00000000000000000, -1.387778780781445676E-14 ) ) ;
#35514 =( NAMED_UNIT ( * ) PLANE_ANGLE_UNIT ( ) SI_UNIT ( $, .RADIAN. ) );
#35515 = CIRCLE ( 'NONE', #15016, 2.000000000000001776 ) ;
#35516 = CARTESIAN_POINT ( 'NONE',  ( 0.1287570809895630941, -0.3962735484563133515, 10.00000000000000000 ) ) ;
#35517 = UNCERTAINTY_MEASURE_WITH_UNIT (LENGTH_MEASURE( 1.000000000000000082E-05 ), #15432, 'distance_accuracy_value', 'NONE');
#35518 = ORIENTED_EDGE ( 'NONE', *, *, #1092, .T. ) ;
#35519 = DIRECTION ( 'NONE',  ( -0.000000000000000000, -0.000000000000000000, -1.000000000000000000 ) ) ;
#35520 = ORIENTED_EDGE ( 'NONE', *, *, #32507, .T. ) ;
#35521 =( GEOMETRIC_REPRESENTATION_CONTEXT ( 3 ) GLOBAL_UNCERTAINTY_ASSIGNED_CONTEXT ( ( #50650 ) ) GLOBAL_UNIT_ASSIGNED_CONTEXT ( ( #27696, #39763, #44826 ) ) REPRESENTATION_CONTEXT ( 'NONE', 'WORKASPACE' ) );
#35522 = DIRECTION ( 'NONE',  ( 0.000000000000000000, 0.000000000000000000, -1.000000000000000000 ) ) ;
#35523 = VERTEX_POINT ( 'NONE', #30295 ) ;
#35524 = DIRECTION ( 'NONE',  ( -1.000000000000000000, 0.000000000000000000, 0.000000000000000000 ) ) ;
#35525 = CARTESIAN_POINT ( 'NONE',  ( 164.9999999999999716, 17.00000000000000000, 115.0000000000000142 ) ) ;
#35526 = CARTESIAN_POINT ( 'NONE',  ( -167.7210997126620384, 1.750000000000009548, -118.1565861772249519 ) ) ;
#35527 = PLANE ( 'NONE',  #47844 ) ;
#35528 = CARTESIAN_POINT ( 'NONE',  ( 1.066995270233474624, -50.00000000000000711, -3.760136334089591248 ) ) ;
#35529 = ORIENTED_EDGE ( 'NONE', *, *, #33711, .F. ) ;
#35530 = EDGE_LOOP ( 'NONE', ( #9103, #36576, #46393, #4996 ) ) ;
#35531 = CARTESIAN_POINT ( 'NONE',  ( -6.695973446814940111, -1.750000000000024203, 80.81828755692798438 ) ) ;
#35532 = B_SPLINE_SURFACE_WITH_KNOTS ( 'NONE', 3, 3, ( 
 ( #8509, #39815, #31617, #4656 ),
 ( #40062, #47203, #39560, #565 ),
 ( #12102, #8250, #36218, #4396 ),
 ( #44133, #20045, #16200, #31864 ) ),
 .UNSPECIFIED., .F., .F., .F.,
 ( 4, 4 ),
 ( 4, 4 ),
 ( 0.000000000000000000, 1.000000000000000000 ),
 ( 0.000000000000000000, 1.000000000000000000 ),
 .UNSPECIFIED. ) ;
#35533 = DIRECTION ( 'NONE',  ( -0.000000000000000000, -0.000000000000000000, -1.000000000000000000 ) ) ;
#35534 = CARTESIAN_POINT ( 'NONE',  ( 33.30402655318503946, 0.000000000000000000, 165.0000000000000000 ) ) ;
#35536 =( NAMED_UNIT ( * ) PLANE_ANGLE_UNIT ( ) SI_UNIT ( $, .RADIAN. ) );
#35535 = B_SPLINE_CURVE_WITH_KNOTS ( 'NONE', 3,
 ( #37004, #48468, #9264, #5660 ),
 .UNSPECIFIED., .F., .F.,
 ( 4, 4 ),
 ( 0.0001535465953326810848, 0.0005837444810856193397 ),
 .UNSPECIFIED. ) ;
#35537 = CARTESIAN_POINT ( 'NONE',  ( 0.1287570809895630941, -0.3962735484563133515, 10.00000000000000000 ) ) ;
#35538 = VERTEX_POINT ( 'NONE', #26191 ) ;
#35539 = EDGE_CURVE ( 'NONE', #21654, #3325, #27376, .T. ) ;
#35540 = CARTESIAN_POINT ( 'NONE',  ( 355.9999999999999432, 185.0000000000002274, -360.0000000000003411 ) ) ;
#35541 = FACE_OUTER_BOUND ( 'NONE', #313, .T. ) ;
#35542 = EDGE_LOOP ( 'NONE', ( #36135, #39083, #13063, #9581 ) ) ;
#35543 = CARTESIAN_POINT ( 'NONE',  ( 111.5540265531850679, 0.000000000000000000, 82.56828755692797017 ) ) ;
#35544 = CIRCLE ( 'NONE', #42911, 4.000000000000003553 ) ;
#35545 = CARTESIAN_POINT ( 'NONE',  ( 30.00000000000029132, 16.00000000000000000, -60.00000000000000000 ) ) ;
#35546 = CYLINDRICAL_SURFACE ( 'NONE', #31616, 1.750000000000015543 ) ;
#35547 = AXIS2_PLACEMENT_3D ( 'NONE', #45002, #48079, #12959 ) ;
#35548 = EDGE_CURVE ( 'NONE', #45538, #14054, #17967, .T. ) ;
#35549 = EDGE_CURVE ( 'NONE', #14126, #30097, #14118, .T. ) ;
#35550 = ORIENTED_EDGE ( 'NONE', *, *, #44364, .F. ) ;
#35551 = ORIENTED_EDGE ( 'NONE', *, *, #1667, .F. ) ;
#35552 = CARTESIAN_POINT ( 'NONE',  ( 210.0000000000000568, 0.000000000000000000, -157.4317124430720298 ) ) ;
#35553 =( GEOMETRIC_REPRESENTATION_CONTEXT ( 3 ) GLOBAL_UNCERTAINTY_ASSIGNED_CONTEXT ( ( #23514 ) ) GLOBAL_UNIT_ASSIGNED_CONTEXT ( ( #13364, #17962, #41079 ) ) REPRESENTATION_CONTEXT ( 'NONE', 'WORKASPACE' ) );
#35554 = CARTESIAN_POINT ( 'NONE',  ( 14.48769039275578407, 30.44468701195595983, 8.807470649214879543 ) ) ;
#35555 = EDGE_CURVE ( 'NONE', #46181, #11387, #16167, .T. ) ;
#35556 = ORIENTED_EDGE ( 'NONE', *, *, #44962, .T. ) ;
#35557 = ORIENTED_EDGE ( 'NONE', *, *, #39462, .F. ) ;
#35558 = CARTESIAN_POINT ( 'NONE',  ( -84.94597344681494633, 2.143131898507880377E-16, 165.0000000000000000 ) ) ;
#35559 = CARTESIAN_POINT ( 'NONE',  ( 340.0000000000000568, 183.0000000000000284, 343.9999999999997726 ) ) ;
#35560 = CARTESIAN_POINT ( 'NONE',  ( 224.9999999999999716, -175.0000000000000000, 444.9999999999998295 ) ) ;
#35561 = CARTESIAN_POINT ( 'NONE',  ( 340.0000000000000568, 169.0000000000000000, 349.9999999999998295 ) ) ;
#35562 = ORIENTED_EDGE ( 'NONE', *, *, #45374, .T. ) ;
#35563 = ORIENTED_EDGE ( 'NONE', *, *, #34656, .F. ) ;
#35564 = ORIENTED_EDGE ( 'NONE', *, *, #31490, .F. ) ;
#35565 = EDGE_CURVE ( 'NONE', #12438, #7169, #17976, .T. ) ;
#35566 = EDGE_CURVE ( 'NONE', #17256, #11190, #32631, .T. ) ;
#35567 = CARTESIAN_POINT ( 'NONE',  ( 224.9999999999999432, -175.0000000000000000, 500.0000000000000000 ) ) ;
#35568 = EDGE_CURVE ( 'NONE', #41244, #22918, #15404, .T. ) ;
#35569 = EDGE_LOOP ( 'NONE', ( #8969, #47163, #34894, #13181 ) ) ;
#35570 = EDGE_CURVE ( 'NONE', #16395, #2436, #23602, .T. ) ;
#35571 = VECTOR ( 'NONE', #17005, 1000.000000000000000 ) ;
#35572 = CARTESIAN_POINT ( 'NONE',  ( 35.00000000000186162, 16.00000000000000000, 90.00000000000000000 ) ) ;
#35573 = LINE ( 'NONE', #15548, #10700 ) ;
#35574 = ORIENTED_EDGE ( 'NONE', *, *, #32920, .T. ) ;
#35575 =( BOUNDED_CURVE ( )  B_SPLINE_CURVE ( 3, ( #25762, #10855, #33721, #26018 ),
 .UNSPECIFIED., .F., .F. ) 
 B_SPLINE_CURVE_WITH_KNOTS ( ( 4, 4 ),
 ( 1.570796326794896558, 3.141592653589793116 ),
 .UNSPECIFIED. ) 
 CURVE ( )  GEOMETRIC_REPRESENTATION_ITEM ( )  RATIONAL_B_SPLINE_CURVE ( ( 1.000000000000000000, 0.8047378541243649375, 0.8047378541243649375, 1.000000000000000000 ) ) 
 REPRESENTATION_ITEM ( '' )  );
#35576 = VERTEX_POINT ( 'NONE', #39524 ) ;
#35577 = FACE_OUTER_BOUND ( 'NONE', #26263, .T. ) ;
#35578 = CARTESIAN_POINT ( 'NONE',  ( -1.250000000000000222, 0.000000000000000000, -3.333333333333333481 ) ) ;
#35579 = ADVANCED_FACE ( 'NONE', ( #3588 ), #38762, .T. ) ;
#35580 = DIRECTION ( 'NONE',  ( 0.000000000000000000, -1.604368532695312981E-16, -1.000000000000000000 ) ) ;
#35581 = ORIENTED_EDGE ( 'NONE', *, *, #44603, .F. ) ;
#35582 = ORIENTED_EDGE ( 'NONE', *, *, #8880, .F. ) ;
#35583 = CARTESIAN_POINT ( 'NONE',  ( -114.9999999999981526, 17.00000000000000000, 65.00000000000000000 ) ) ;
#35584 = DIRECTION ( 'NONE',  ( -0.000000000000000000, -0.000000000000000000, -1.000000000000000000 ) ) ;
#35585 = ORIENTED_EDGE ( 'NONE', *, *, #1700, .T. ) ;
#35586 = DIRECTION ( 'NONE',  ( 1.000000000000000000, 0.000000000000000000, 0.000000000000000000 ) ) ;
#35587 = CARTESIAN_POINT ( 'NONE',  ( 30.00000000000092726, 17.00000000000000000, -24.99999999999999289 ) ) ;
#35588 = DIRECTION ( 'NONE',  ( -1.000000000000000000, -0.000000000000000000, -0.000000000000000000 ) ) ;
#35589 = AXIS2_PLACEMENT_3D ( 'NONE', #15409, #22841, #18485 ) ;
#35590 = AXIS2_PLACEMENT_3D ( 'NONE', #45835, #10227, #14062 ) ;
#35591 = CARTESIAN_POINT ( 'NONE',  ( 4.339432828817248122, 37.24807810779213213, -8.192531242611266862 ) ) ;
#35592 = ORIENTED_EDGE ( 'NONE', *, *, #12669, .T. ) ;
#35593 = VECTOR ( 'NONE', #46888, 1000.000000000000000 ) ;
#35594 = FACE_OUTER_BOUND ( 'NONE', #35243, .T. ) ;
#35595 = CARTESIAN_POINT ( 'NONE',  ( -48.44597344681495343, 0.000000000000000000, -80.93171244307204404 ) ) ;
#35596 = PLANE ( 'NONE',  #44064 ) ;
#35597 = EDGE_CURVE ( 'NONE', #35621, #12549, #2786, .T. ) ;
#35598 = VECTOR ( 'NONE', #44520, 1000.000000000000000 ) ;
#35599 = CARTESIAN_POINT ( 'NONE',  ( 155.0540265531850537, 2.143131898507880377E-16, -77.43171244307204404 ) ) ;
#35600 = EDGE_CURVE ( 'NONE', #29055, #2997, #29024, .T. ) ;
#35601 = ADVANCED_FACE ( 'NONE', ( #3849 ), #31829, .T. ) ;
#35602 = CARTESIAN_POINT ( 'NONE',  ( -194.9999999999999432, 173.0000000000000000, 231.9999999999999716 ) ) ;
#35603 = EDGE_CURVE ( 'NONE', #28634, #11806, #12302, .T. ) ;
#35604 = CARTESIAN_POINT ( 'NONE',  ( -0.6595498452743703277, 16.59563386392009576, 3.266473740018926541 ) ) ;
#35605 = LINE ( 'NONE', #4026, #33692 ) ;
#35606 = EDGE_CURVE ( 'NONE', #3991, #25566, #26199, .T. ) ;
#35607 = ORIENTED_EDGE ( 'NONE', *, *, #18452, .F. ) ;
#35608 = LINE ( 'NONE', #8646, #28104 ) ;
#35609 = AXIS2_PLACEMENT_3D ( 'NONE', #23576, #12033, #12520 ) ;
#35610 = DIRECTION ( 'NONE',  ( -0.000000000000000000, -0.000000000000000000, -1.000000000000000000 ) ) ;
#35611 = ORIENTED_EDGE ( 'NONE', *, *, #36226, .T. ) ;
#35612 = CARTESIAN_POINT ( 'NONE',  ( 34.32915281903212446, -1.750000000000009548, 41.84341382277508359 ) ) ;
#35613 = DIRECTION ( 'NONE',  ( 0.000000000000000000, 0.000000000000000000, -1.000000000000000000 ) ) ;
#35614 = CARTESIAN_POINT ( 'NONE',  ( -3.808200756227646089, -0.8261963378076270237, 9.741991644047246268 ) ) ;
#35615 = ORIENTED_EDGE ( 'NONE', *, *, #32781, .F. ) ;
#35616 = CARTESIAN_POINT ( 'NONE',  ( -164.9459734468149463, 2.143131898507880377E-16, -40.93171244307202983 ) ) ;
#35617 = ORIENTED_EDGE ( 'NONE', *, *, #21202, .T. ) ;
#35618 = EDGE_LOOP ( 'NONE', ( #27583, #14246, #31519, #21018 ) ) ;
#35619 = CARTESIAN_POINT ( 'NONE',  ( 181.0000000000000000, -164.9999999999999432, 343.9999999999998863 ) ) ;
#35620 = DIRECTION ( 'NONE',  ( -1.000000000000000000, 0.000000000000000000, 0.000000000000000000 ) ) ;
#35621 = VERTEX_POINT ( 'NONE', #46659 ) ;
#35622 = DIRECTION ( 'NONE',  ( -0.000000000000000000, 0.9749645535258956164, 0.2223603367690631105 ) ) ;
#35623 = CYLINDRICAL_SURFACE ( 'NONE', #7736, 1.750000000000015543 ) ;
#35624 = VECTOR ( 'NONE', #3921, 1000.000000000000000 ) ;
#35625 = EDGE_CURVE ( 'NONE', #48047, #18735, #31578, .T. ) ;
#35626 = EDGE_LOOP ( 'NONE', ( #8035, #46455, #1962, #14650, #21933, #38895 ) ) ;
#35627 = VECTOR ( 'NONE', #17728, 1000.000000000000000 ) ;
#35628 = DIRECTION ( 'NONE',  ( -1.000000000000000000, -0.000000000000000000, -0.000000000000000000 ) ) ;
#35629 = ORIENTED_EDGE ( 'NONE', *, *, #3841, .T. ) ;
#35630 = AXIS2_PLACEMENT_3D ( 'NONE', #1609, #1358, #20590 ) ;
#35631 = CARTESIAN_POINT ( 'NONE',  ( 164.9999999999999716, 165.0000000000000000, -344.0000000000001137 ) ) ;
#35632 = CARTESIAN_POINT ( 'NONE',  ( 344.0000000000000000, 174.9999999999996874, -342.0000000000002842 ) ) ;
#35633 = LINE ( 'NONE', #24071, #17681 ) ;
#35634 =( BOUNDED_CURVE ( )  B_SPLINE_CURVE ( 3, ( #532, #47417, #33338, #29727 ),
 .UNSPECIFIED., .F., .F. ) 
 B_SPLINE_CURVE_WITH_KNOTS ( ( 4, 4 ),
 ( 4.712388980384689674, 6.283185307179586232 ),
 .UNSPECIFIED. ) 
 CURVE ( )  GEOMETRIC_REPRESENTATION_ITEM ( )  RATIONAL_B_SPLINE_CURVE ( ( 1.000000000000000000, 0.8047378541243649375, 0.8047378541243649375, 1.000000000000000000 ) ) 
 REPRESENTATION_ITEM ( '' )  );
#35635 = ADVANCED_FACE ( 'NONE', ( #50498 ), #15652, .T. ) ;
#35636 = EDGE_LOOP ( 'NONE', ( #2463, #2830, #13849 ) ) ;
#35637 = EDGE_CURVE ( 'NONE', #2259, #45927, #18521, .T. ) ;
#35638 = DIRECTION ( 'NONE',  ( -0.000000000000000000, -1.000000000000000000, -0.000000000000000000 ) ) ;
#35639 = DIRECTION ( 'NONE',  ( 0.000000000000000000, -1.000000000000000000, 1.604368532695312981E-16 ) ) ;
#35640 = VERTEX_POINT ( 'NONE', #23348 ) ;
#35641 = ORIENTED_EDGE ( 'NONE', *, *, #28761, .T. ) ;
#35642 = ORIENTED_EDGE ( 'NONE', *, *, #20801, .T. ) ;
#35643 = CARTESIAN_POINT ( 'NONE',  ( 135.0000000000003411, 17.00000000000000000, -60.00000000000000000 ) ) ;
#35644 = EDGE_CURVE ( 'NONE', #42413, #22765, #43101, .T. ) ;
#35645 =( BOUNDED_CURVE ( )  B_SPLINE_CURVE ( 3, ( #8833, #21127, #36805, #13423 ),
 .UNSPECIFIED., .F., .F. ) 
 B_SPLINE_CURVE_WITH_KNOTS ( ( 4, 4 ),
 ( 1.570796326794896558, 3.141592653589793116 ),
 .UNSPECIFIED. ) 
 CURVE ( )  GEOMETRIC_REPRESENTATION_ITEM ( )  RATIONAL_B_SPLINE_CURVE ( ( 1.000000000000000000, 0.8047378541243649375, 0.8047378541243649375, 1.000000000000000000 ) ) 
 REPRESENTATION_ITEM ( '' )  );
#35646 = ADVANCED_FACE ( 'NONE', ( #23863 ), #4365, .T. ) ;
#35647 = CARTESIAN_POINT ( 'NONE',  ( 154.3291528190321458, -1.750000000000009326, 1.843413822775066269 ) ) ;
#35648 = PRODUCT_DEFINITION_SHAPE ( 'NONE', 'NONE',  #50728 ) ;
#35649 = ORIENTED_EDGE ( 'NONE', *, *, #49062, .T. ) ;
#35650 = ADVANCED_FACE ( 'NONE', ( #12814 ), #9211, .T. ) ;
#35651 = LINE ( 'NONE', #27419, #48699 ) ;
#35652 = FACE_OUTER_BOUND ( 'NONE', #49640, .T. ) ;
#35653 = CARTESIAN_POINT ( 'NONE',  ( -47.72109971266203132, -1.750000000000009548, 159.7931612910809065 ) ) ;
#35654 = VECTOR ( 'NONE', #26041, 1000.000000000000000 ) ;
#35655 = LINE ( 'NONE', #46332, #19782 ) ;
#35656 = CARTESIAN_POINT ( 'NONE',  ( -0.09523839817533703844, -1.466467394240187350, 9.958264684458541183 ) ) ;
#35657 = CARTESIAN_POINT ( 'NONE',  ( -7.372990760266265653, 0.000000000000000000, 22.00000000000000000 ) ) ;
#35658 = SURFACE_STYLE_FILL_AREA ( #24094 ) ;
#35659 = LINE ( 'NONE', #8443, #20113 ) ;
#35660 = CARTESIAN_POINT ( 'NONE',  ( -114.9999999999997158, 17.00000000000000000, -60.00000000000000000 ) ) ;
#35661 = B_SPLINE_CURVE_WITH_KNOTS ( 'NONE', 3,
 ( #42543, #41549, #45860, #18941 ),
 .UNSPECIFIED., .F., .F.,
 ( 4, 4 ),
 ( 0.0009679537044785101619, 0.001281751046851273322 ),
 .UNSPECIFIED. ) ;
#35662 = DIRECTION ( 'NONE',  ( 0.000000000000000000, 0.000000000000000000, -1.000000000000000000 ) ) ;
#35663 = CARTESIAN_POINT ( 'NONE',  ( 1.365263087672787590, -0.5437404457008400138, 9.958264684458717042 ) ) ;
#35664 = LINE ( 'NONE', #31552, #11860 ) ;
#35665 = EDGE_CURVE ( 'NONE', #23383, #34290, #23781, .T. ) ;
#35666 = VECTOR ( 'NONE', #14005, 1000.000000000000000 ) ;
#35667 = CARTESIAN_POINT ( 'NONE',  ( -64.99999999999877787, 17.00000000000000000, 5.000000000000004441 ) ) ;
#35668 = DIRECTION ( 'NONE',  ( -0.000000000000000000, -0.000000000000000000, -1.000000000000000000 ) ) ;
#35669 = ORIENTED_EDGE ( 'NONE', *, *, #17830, .T. ) ;
#35670 = CARTESIAN_POINT ( 'NONE',  ( 210.0000000000000568, 0.000000000000000000, -159.1817124430720298 ) ) ;
#35671 = DIRECTION ( 'NONE',  ( -0.000000000000000000, -1.000000000000000000, -0.000000000000000000 ) ) ;
#35672 = CARTESIAN_POINT ( 'NONE',  ( -10.49999999999999467, -46.51315789473684248, 5.916985404131814619 ) ) ;
#35673 = VECTOR ( 'NONE', #15369, 1000.000000000000000 ) ;
#35674 = CARTESIAN_POINT ( 'NONE',  ( -0.3862712429686977478, 1.188820645368937390, 3.333333333333333481 ) ) ;
#35675 = ORIENTED_EDGE ( 'NONE', *, *, #30598, .T. ) ;
#35676 = VERTEX_POINT ( 'NONE', #43852 ) ;
#35677 = CARTESIAN_POINT ( 'NONE',  ( 50.11058929355270664, -7.578863168071591438, 7.455576670931136185 ) ) ;
#35678 = ORIENTED_EDGE ( 'NONE', *, *, #33729, .T. ) ;
#35680 = EDGE_CURVE ( 'NONE', #44903, #23347, #40271, .T. ) ;
#35679 = DIRECTION ( 'NONE',  ( -1.000000000000000000, -0.000000000000000000, -0.000000000000000000 ) ) ;
#35681 = LINE ( 'NONE', #32320, #11268 ) ;
#35682 = ORIENTED_EDGE ( 'NONE', *, *, #45727, .T. ) ;
#35683 = CYLINDRICAL_SURFACE ( 'NONE', #10145, 0.5000000000000004441 ) ;
#35684 = ORIENTED_EDGE ( 'NONE', *, *, #1420, .F. ) ;
#35685 = VECTOR ( 'NONE', #1955, 1000.000000000000000 ) ;
#35686 = VERTEX_POINT ( 'NONE', #44342 ) ;
#35687 = CARTESIAN_POINT ( 'NONE',  ( 113.3040265531850537, 0.000000000000000000, 165.0000000000000000 ) ) ;
#35688 = LINE ( 'NONE', #39271, #311 ) ;
#35689 = AXIS2_PLACEMENT_3D ( 'NONE', #23071, #19213, #35158 ) ;
#35690 = VERTEX_POINT ( 'NONE', #5609 ) ;
#35691 = FACE_OUTER_BOUND ( 'NONE', #37830, .T. ) ;
#35692 = FACE_OUTER_BOUND ( 'NONE', #16040, .T. ) ;
#35693 = DIRECTION ( 'NONE',  ( 0.000000000000000000, 0.000000000000000000, 1.000000000000000000 ) ) ;
#35694 = CARTESIAN_POINT ( 'NONE',  ( -86.69597344681494633, -1.750000000000009992, 160.8182875569279702 ) ) ;
#35695 = CARTESIAN_POINT ( 'NONE',  ( 193.3040265531851105, -1.750000000000010658, 120.8182875569279702 ) ) ;
#35696 = VECTOR ( 'NONE', #22124, 1000.000000000000000 ) ;
#35697 = EDGE_CURVE ( 'NONE', #9233, #30056, #11339, .T. ) ;
#35698 = ORIENTED_EDGE ( 'NONE', *, *, #27057, .F. ) ;
#35699 = ADVANCED_FACE ( 'NONE', ( #24623 ), #25373, .F. ) ;
#35700 = CYLINDRICAL_SURFACE ( 'NONE', #21813, 4.000000000000003553 ) ;
#35701 = VECTOR ( 'NONE', #15112, 1000.000000000000000 ) ;
#35702 = CARTESIAN_POINT ( 'NONE',  ( -164.4973046169135955, 70.03596893647589638, -93.79675437945476801 ) ) ;
#35703 = VECTOR ( 'NONE', #16673, 1000.000000000000000 ) ;
#35704 = EDGE_LOOP ( 'NONE', ( #19696, #18642, #11263, #35786 ) ) ;
#35705 = CARTESIAN_POINT ( 'NONE',  ( 164.9999999999999716, 6.000000000000060396, -350.0000000000001705 ) ) ;
#35706 = ADVANCED_FACE ( 'NONE', ( #8729 ), #48667, .T. ) ;
#35707 = DIRECTION ( 'NONE',  ( -1.000000000000000000, -0.000000000000000000, -0.000000000000000000 ) ) ;
#35708 = CARTESIAN_POINT ( 'NONE',  ( 340.0000000000000568, 169.0000000000000284, 343.9999999999998295 ) ) ;
#35709 = EDGE_LOOP ( 'NONE', ( #27893, #25105, #48373, #32582 ) ) ;
#35710 = AXIS2_PLACEMENT_3D ( 'NONE', #40239, #1992, #48637 ) ;
#35711 = CARTESIAN_POINT ( 'NONE',  ( -1.104213410210672430, -0.6509177773818179968, 9.976582533991678048 ) ) ;
#35712 = EDGE_CURVE ( 'NONE', #21405, #7855, #20509, .T. ) ;
#35713 = CARTESIAN_POINT ( 'NONE',  ( 35.05402655318504657, 2.143131898507880377E-16, -40.93171244307205825 ) ) ;
#35714 = DIRECTION ( 'NONE',  ( -1.000000000000000000, -0.000000000000000000, -0.000000000000000000 ) ) ;
#35715 = EDGE_CURVE ( 'NONE', #25915, #48491, #13056, .T. ) ;
#35716 = CARTESIAN_POINT ( 'NONE',  ( 344.0000000000000000, 174.9999999999996589, -340.0000000000002842 ) ) ;
#35717 = ORIENTED_EDGE ( 'NONE', *, *, #31504, .T. ) ;
#35718 = CARTESIAN_POINT ( 'NONE',  ( -6.695973446814940111, 0.000000000000000000, -165.0000000000000000 ) ) ;
#35719 = CARTESIAN_POINT ( 'NONE',  ( 29.39982726364966581, 16.78152490921169360, 8.356839323120299312 ) ) ;
#35720 = EDGE_CURVE ( 'NONE', #36600, #7468, #36178, .T. ) ;
#35721 = CARTESIAN_POINT ( 'NONE',  ( -26.18032376592659105, 21.95228666728381128, 7.455576670931136185 ) ) ;
#35722 = ORIENTED_EDGE ( 'NONE', *, *, #50468, .T. ) ;
#35723 = ORIENTED_EDGE ( 'NONE', *, *, #25967, .T. ) ;
#35724 = DIRECTION ( 'NONE',  ( 0.9767437569925631058, -4.158490309726805533E-16, 0.2144099651976388021 ) ) ;
#35725 = CARTESIAN_POINT ( 'NONE',  ( 33.30402655318503946, -1.750000000000009992, -159.1817124430720298 ) ) ;
#35726 = CARTESIAN_POINT ( 'NONE',  ( -7.787881821992606035, -1.707024098816393165, -7.318364664277154930E-16 ) ) ;
#35727 = VECTOR ( 'NONE', #38327, 1000.000000000000000 ) ;
#35728 = CARTESIAN_POINT ( 'NONE',  ( 183.0000000000000000, 165.0000000000000000, -344.0000000000001137 ) ) ;
#35729 = AXIS2_PLACEMENT_3D ( 'NONE', #11688, #10671, #3467 ) ;
#35730 = CARTESIAN_POINT ( 'NONE',  ( 195.0540265531851105, 2.143131898507880377E-16, -37.43171244307205825 ) ) ;
#35731 = ORIENTED_EDGE ( 'NONE', *, *, #32922, .T. ) ;
#35732 = DIRECTION ( 'NONE',  ( -1.000000000000000000, -0.000000000000000000, -0.000000000000000000 ) ) ;
#35733 = VECTOR ( 'NONE', #47010, 1000.000000000000000 ) ;
#35734 = CARTESIAN_POINT ( 'NONE',  ( 168.9999999999999716, -97.49999999999998579, -350.0000000000001705 ) ) ;
#35735 = CARTESIAN_POINT ( 'NONE',  ( 7.608425291889091113, -36.72004717559254772, 7.697694107796188234 ) ) ;
#35736 = CARTESIAN_POINT ( 'NONE',  ( 356.0000000000000000, 165.0000000000000000, -106.0000000000001990 ) ) ;
#35737 = VERTEX_POINT ( 'NONE', #17168 ) ;
#35738 = CARTESIAN_POINT ( 'NONE',  ( -86.69597344681496054, 0.000000000000000000, -165.0000000000000000 ) ) ;
#35739 = VERTEX_POINT ( 'NONE', #20756 ) ;
#35740 = DIRECTION ( 'NONE',  ( -0.000000000000000000, -0.000000000000000000, -1.000000000000000000 ) ) ;
#35741 = VECTOR ( 'NONE', #11643, 1000.000000000000000 ) ;
#35742 = ORIENTED_EDGE ( 'NONE', *, *, #47179, .F. ) ;
#35743 = CARTESIAN_POINT ( 'NONE',  ( 22.69295089195473736, 45.31600496604706052, 7.455576670931136185 ) ) ;
#35744 = CARTESIAN_POINT ( 'NONE',  ( 73.30402655318508209, -1.750000000000010214, 40.81828755692798438 ) ) ;
#35745 = CARTESIAN_POINT ( 'NONE',  ( 195.0540265531851105, 2.143131898507880377E-16, 42.56828755692798438 ) ) ;
#35746 = VECTOR ( 'NONE', #35345, 1000.000000000000000 ) ;
#35747 = VERTEX_POINT ( 'NONE', #769 ) ;
#35748 = EDGE_CURVE ( 'NONE', #49664, #3886, #15539, .T. ) ;
#35749 = VECTOR ( 'NONE', #20129, 1000.000000000000000 ) ;
#35750 = FACE_OUTER_BOUND ( 'NONE', #36110, .T. ) ;
#35751 = CARTESIAN_POINT ( 'NONE',  ( 0.000000000000000000, 181.0000000000000284, -360.0000000000002274 ) ) ;
#35752 = EDGE_LOOP ( 'NONE', ( #44249, #31105, #43463 ) ) ;
#35753 = DIRECTION ( 'NONE',  ( 1.132880637372608740E-16, 4.718402560806925739E-50, 1.000000000000000000 ) ) ;
#35754 = LINE ( 'NONE', #11873, #38843 ) ;
#35755 = DIRECTION ( 'NONE',  ( -1.000000000000000000, 0.000000000000000000, 0.000000000000000000 ) ) ;
#35756 = CARTESIAN_POINT ( 'NONE',  ( 168.9999999999999716, -168.9999999999999432, -350.0000000000001705 ) ) ;
#35757 = ORIENTED_EDGE ( 'NONE', *, *, #24268, .T. ) ;
#35758 = ORIENTED_EDGE ( 'NONE', *, *, #4220, .T. ) ;
#35759 = DIRECTION ( 'NONE',  ( -0.7233555441435720601, 0.6904757466825007794, 0.000000000000000000 ) ) ;
#35760 = VECTOR ( 'NONE', #26703, 1000.000000000000000 ) ;
#35761 = EDGE_CURVE ( 'NONE', #11032, #11806, #1526, .T. ) ;
#35762 = VERTEX_POINT ( 'NONE', #16929 ) ;
#35763 = ADVANCED_FACE ( 'NONE', ( #24867 ), #32834, .F. ) ;
#35764 = CARTESIAN_POINT ( 'NONE',  ( 5.551115123125782702E-14, -180.9999999999999716, 343.9999999999997726 ) ) ;
#35765 = CARTESIAN_POINT ( 'NONE',  ( 130.0000000000015064, 17.00000000000000000, 35.00000000000000000 ) ) ;
#35766 = DIRECTION ( 'NONE',  ( -0.000000000000000000, -0.000000000000000000, -1.000000000000000000 ) ) ;
#35767 = ORIENTED_EDGE ( 'NONE', *, *, #7975, .T. ) ;
#35768 = CARTESIAN_POINT ( 'NONE',  ( 1.011271242968688311, -0.7347315653655855927, -3.333333333333333481 ) ) ;
#35769 = ORIENTED_EDGE ( 'NONE', *, *, #7571, .F. ) ;
#35770 = B_SPLINE_CURVE_WITH_KNOTS ( 'NONE', 3,
 ( #48367, #1721, #17613, #33526 ),
 .UNSPECIFIED., .F., .F.,
 ( 4, 4 ),
 ( 0.001937412222931650689, 0.003978261222106149742 ),
 .UNSPECIFIED. ) ;
#35771 = CARTESIAN_POINT ( 'NONE',  ( 73.30402655318508209, 0.000000000000000000, 165.0000000000000000 ) ) ;
#35772 = ADVANCED_FACE ( 'NONE', ( #13305 ), #28964, .T. ) ;
#35773 = EDGE_CURVE ( 'NONE', #48958, #8816, #14571, .T. ) ;
#35775 = VECTOR ( 'NONE', #22727, 1000.000000000000000 ) ;
#35774 = CARTESIAN_POINT ( 'NONE',  ( -4.763548243873389154, 16.57409059453848599, 8.727788335465566760 ) ) ;
#35776 = ORIENTED_EDGE ( 'NONE', *, *, #37506, .T. ) ;
#35777 = VERTEX_POINT ( 'NONE', #37448 ) ;
#35778 = VECTOR ( 'NONE', #7428, 1000.000000000000000 ) ;
#35779 = ORIENTED_EDGE ( 'NONE', *, *, #36329, .F. ) ;
#35780 = CARTESIAN_POINT ( 'NONE',  ( 21.24469349090191983, -33.89193117067290473, 910.0000000000000000 ) ) ;
#35781 = EDGE_CURVE ( 'NONE', #5809, #32394, #25627, .T. ) ;
#35782 = CARTESIAN_POINT ( 'NONE',  ( -84.94597344681494633, 2.143131898507880377E-16, 159.0682875569279702 ) ) ;
#35783 = CARTESIAN_POINT ( 'NONE',  ( 165.0000000000000000, 2.775557561562891351E-14, -99.00000000000014211 ) ) ;
#35784 = ORIENTED_EDGE ( 'NONE', *, *, #5509, .F. ) ;
#35785 = DIRECTION ( 'NONE',  ( 0.000000000000000000, -0.000000000000000000, -1.000000000000000000 ) ) ;
#35786 = ORIENTED_EDGE ( 'NONE', *, *, #3598, .F. ) ;
#35787 = CIRCLE ( 'NONE', #45573, 1.750000000000015543 ) ;
#35788 = CARTESIAN_POINT ( 'NONE',  ( 181.0000000000000000, -93.49999999999998579, -340.0000000000001137 ) ) ;
#35789 = ORIENTED_EDGE ( 'NONE', *, *, #38139, .T. ) ;
#35790 =( BOUNDED_CURVE ( )  B_SPLINE_CURVE ( 3, ( #29195, #44812, #49142, #5834 ),
 .UNSPECIFIED., .F., .F. ) 
 B_SPLINE_CURVE_WITH_KNOTS ( ( 4, 4 ),
 ( 3.141592653589793116, 4.712388980384689674 ),
 .UNSPECIFIED. ) 
 CURVE ( )  GEOMETRIC_REPRESENTATION_ITEM ( )  RATIONAL_B_SPLINE_CURVE ( ( 1.000000000000000000, 0.8047378541243649375, 0.8047378541243649375, 1.000000000000000000 ) ) 
 REPRESENTATION_ITEM ( '' )  );
#35791 = FACE_OUTER_BOUND ( 'NONE', #25723, .T. ) ;
#35792 = LINE ( 'NONE', #8319, #42412 ) ;
#35793 = CARTESIAN_POINT ( 'NONE',  ( 168.9999999999999716, -164.9999999999999432, 343.9999999999998863 ) ) ;
#35794 = LINE ( 'NONE', #28314, #14342 ) ;
#35795 = FACE_OUTER_BOUND ( 'NONE', #41662, .T. ) ;
#35796 = CARTESIAN_POINT ( 'NONE',  ( -128.4459734468149463, -1.025126265847081886, 79.06828755692797017 ) ) ;
#35797 = EDGE_LOOP ( 'NONE', ( #46368, #23927, #13334, #32622, #19376, #38382, #20157, #7759 ) ) ;
#35798 = ORIENTED_EDGE ( 'NONE', *, *, #17205, .T. ) ;
#35799 = CARTESIAN_POINT ( 'NONE',  ( -124.9459734468149463, 2.143131898507842906E-16, 165.0000000000000000 ) ) ;
#35800 =( BOUNDED_CURVE ( )  B_SPLINE_CURVE ( 3, ( #13597, #48450, #17450, #44614 ),
 .UNSPECIFIED., .F., .F. ) 
 B_SPLINE_CURVE_WITH_KNOTS ( ( 4, 4 ),
 ( 1.570796326794896558, 3.141592653589793116 ),
 .UNSPECIFIED. ) 
 CURVE ( )  GEOMETRIC_REPRESENTATION_ITEM ( )  RATIONAL_B_SPLINE_CURVE ( ( 1.000000000000000000, 0.8047378541243649375, 0.8047378541243649375, 1.000000000000000000 ) ) 
 REPRESENTATION_ITEM ( '' )  );
#35801 = CARTESIAN_POINT ( 'NONE',  ( 164.9999999999999716, -180.9999999999999716, -340.0000000000001137 ) ) ;
#35802 = DIRECTION ( 'NONE',  ( 0.000000000000000000, -0.3846153846153845812, -0.9230769230769231282 ) ) ;
#35803 = DIRECTION ( 'NONE',  ( 0.000000000000000000, 3.186989995019654210E-49, 1.000000000000000000 ) ) ;
#35804 = CIRCLE ( 'NONE', #9538, 1.750000000000008438 ) ;
#35805 = VECTOR ( 'NONE', #30703, 1000.000000000000000 ) ;
#35806 = PLANE ( 'NONE',  #35198 ) ;
#35807 = EDGE_LOOP ( 'NONE', ( #34795, #41669, #43662, #32258 ) ) ;
#35808 = CARTESIAN_POINT ( 'NONE',  ( -166.6959734468149463, 1.750000000000009992, 0.8182875569279768335 ) ) ;
#35809 =( BOUNDED_CURVE ( )  B_SPLINE_CURVE ( 3, ( #23236, #12203, #27354, #39669 ),
 .UNSPECIFIED., .F., .F. ) 
 B_SPLINE_CURVE_WITH_KNOTS ( ( 4, 4 ),
 ( 3.141592653589793116, 4.712388980384689674 ),
 .UNSPECIFIED. ) 
 CURVE ( )  GEOMETRIC_REPRESENTATION_ITEM ( )  RATIONAL_B_SPLINE_CURVE ( ( 1.000000000000000000, 0.8047378541243649375, 0.8047378541243649375, 1.000000000000000000 ) ) 
 REPRESENTATION_ITEM ( '' )  );
#35810 = LINE ( 'NONE', #12917, #36186 ) ;
#35811 = EDGE_CURVE ( 'NONE', #47399, #936, #4449, .T. ) ;
#35812 = EDGE_LOOP ( 'NONE', ( #44578, #30479, #50328, #1373, #8708 ) ) ;
#35813 = VECTOR ( 'NONE', #13326, 1000.000000000000000 ) ;
#35814 = CARTESIAN_POINT ( 'NONE',  ( 1.249999999999999778, -0.000000000000000000, -3.333333333333333481 ) ) ;
#35815 = CARTESIAN_POINT ( 'NONE',  ( 35.00000000000152767, 16.00000000000000000, 35.00000000000000000 ) ) ;
#35816 = CARTESIAN_POINT ( 'NONE',  ( 181.0000000000000000, -254.5000000000000000, -114.9999999999999574 ) ) ;
#35817 = ORIENTED_EDGE ( 'NONE', *, *, #20959, .T. ) ;
#35818 = ORIENTED_EDGE ( 'NONE', *, *, #9089, .T. ) ;
#35819 = DIRECTION ( 'NONE',  ( 0.000000000000000000, -1.000000000000000000, 0.000000000000000000 ) ) ;
#35820 = AXIS2_PLACEMENT_3D ( 'NONE', #29231, #17676, #22528 ) ;
#35821 = CARTESIAN_POINT ( 'NONE',  ( 31.28977333267368621, -11.25592690310905652, -2.408242355805840784 ) ) ;
#35822 = EDGE_LOOP ( 'NONE', ( #24496, #19338, #29008, #3708 ) ) ;
#35823 = ORIENTED_EDGE ( 'NONE', *, *, #35160, .F. ) ;
#35824 = CARTESIAN_POINT ( 'NONE',  ( 181.0000000000000000, -272.4999999999999432, -357.9999999999999432 ) ) ;
#35825 = FACE_OUTER_BOUND ( 'NONE', #47676, .T. ) ;
#35826 = CARTESIAN_POINT ( 'NONE',  ( 0.000000000000000000, 165.0000000000000000, 355.9999999999997726 ) ) ;
#35827 = CARTESIAN_POINT ( 'NONE',  ( -205.6708471809678827, -1.750000000000009548, 41.84341382277508359 ) ) ;
#35828 = ORIENTED_EDGE ( 'NONE', *, *, #27760, .F. ) ;
#35829 = EDGE_LOOP ( 'NONE', ( #34000, #28232, #23661, #476, #28125, #22402, #19449, #26002 ) ) ;
#35830 = ORIENTED_EDGE ( 'NONE', *, *, #19620, .T. ) ;
#35831 = DIRECTION ( 'NONE',  ( -1.000000000000000000, -0.000000000000000000, -0.000000000000000000 ) ) ;
#35832 = ORIENTED_EDGE ( 'NONE', *, *, #11819, .T. ) ;
#35833 = VECTOR ( 'NONE', #21030, 1000.000000000000000 ) ;
#35834 = LINE ( 'NONE', #8109, #31202 ) ;
#35835 = EDGE_LOOP ( 'NONE', ( #9351, #40769, #5385, #8418, #19487, #16096, #35317, #47573 ) ) ;
#35836 = ORIENTED_EDGE ( 'NONE', *, *, #14219, .T. ) ;
#35837 = CARTESIAN_POINT ( 'NONE',  ( 185.0000000000000284, -9.999999999999953815, -111.0000000000001563 ) ) ;
#35838 = ADVANCED_FACE ( 'NONE', ( #14826 ), #30481, .F. ) ;
#35839 = CARTESIAN_POINT ( 'NONE',  ( -25.60949810002096783, -43.19700938445173932, 1.847720168420772691 ) ) ;
#35840 = CARTESIAN_POINT ( 'NONE',  ( 0.3862712429686978033, -1.188820645368937834, 10.00000000000000000 ) ) ;
#35841 = ORIENTED_EDGE ( 'NONE', *, *, #24923, .T. ) ;
#35842 = ORIENTED_EDGE ( 'NONE', *, *, #34657, .F. ) ;
#35843 = CARTESIAN_POINT ( 'NONE',  ( -30.87089393895367451, 12.69923079256638232, -9.367992836599951190 ) ) ;
#35844 = VERTEX_POINT ( 'NONE', #46087 ) ;
#35845 = LINE ( 'NONE', #15810, #7522 ) ;
#35846 = DIRECTION ( 'NONE',  ( 0.000000000000000000, 0.000000000000000000, -1.000000000000000000 ) ) ;
#35847 = DIRECTION ( 'NONE',  ( 1.860490536778032451E-50, 0.000000000000000000, -1.000000000000000000 ) ) ;
#35848 = CARTESIAN_POINT ( 'NONE',  ( 35.00000000000028422, 17.00000000000000000, -60.00000000000000000 ) ) ;
#35849 = ORIENTED_EDGE ( 'NONE', *, *, #14281, .T. ) ;
#35850 = CARTESIAN_POINT ( 'NONE',  ( 29.99999999999998579, 17.00000000000000000, -90.00000000000000000 ) ) ;
#35851 = CARTESIAN_POINT ( 'NONE',  ( 14.49999999999999822, -3.557843729863133575, 15.59977635401528673 ) ) ;
#35852 = CARTESIAN_POINT ( 'NONE',  ( 342.8284271247461561, -167.0000000000001137, -342.0000000000002842 ) ) ;
#35853 = ADVANCED_FACE ( 'NONE', ( #41768 ), #41262, .F. ) ;
#35854 = CYLINDRICAL_SURFACE ( 'NONE', #14027, 0.5000000000000004441 ) ;
#35855 = CARTESIAN_POINT ( 'NONE',  ( -48.44597344681495343, 0.000000000000000000, 79.06828755692797017 ) ) ;
#35856 = CARTESIAN_POINT ( 'NONE',  ( -166.6959734468149463, 1.750000000000009992, 160.8182875569279702 ) ) ;
#35857 = DIRECTION ( 'NONE',  ( 0.000000000000000000, 0.9749645535258955054, 0.2223603367690637767 ) ) ;
#35858 = ORIENTED_EDGE ( 'NONE', *, *, #37611, .T. ) ;
#35859 = AXIS2_PLACEMENT_3D ( 'NONE', #20499, #36169, #6908 ) ;
#35860 = CARTESIAN_POINT ( 'NONE',  ( 35.05402655318504657, 2.143131898507880377E-16, 39.06828755692798438 ) ) ;
#35861 = VERTEX_POINT ( 'NONE', #3016 ) ;
#35862 = CARTESIAN_POINT ( 'NONE',  ( -8.445973446814976526, 0.000000000000000000, -120.9317124430720725 ) ) ;
#35863 = CARTESIAN_POINT ( 'NONE',  ( 55.00000000000002132, 52.49999999999999289, 5.000000000000000000 ) ) ;
#35864 = FACE_OUTER_BOUND ( 'NONE', #15888, .T. ) ;
#35865 = ORIENTED_EDGE ( 'NONE', *, *, #23099, .F. ) ;
#35866 = CARTESIAN_POINT ( 'NONE',  ( 113.3040265531850537, 1.749999999999997335, 80.81828755692798438 ) ) ;
#35867 = ORIENTED_EDGE ( 'NONE', *, *, #28995, .F. ) ;
#35868 = ORIENTED_EDGE ( 'NONE', *, *, #8953, .F. ) ;
#35869 = DIRECTION ( 'NONE',  ( 0.000000000000000000, 0.000000000000000000, -1.000000000000000000 ) ) ;
#35870 = CARTESIAN_POINT ( 'NONE',  ( -8.445973446814976526, 0.000000000000000000, 79.06828755692795596 ) ) ;
#35871 = ORIENTED_EDGE ( 'NONE', *, *, #43896, .T. ) ;
#35872 = CARTESIAN_POINT ( 'NONE',  ( 0.000000000000000000, -250.0000000000000000, -224.9999999999999716 ) ) ;
#35873 = CARTESIAN_POINT ( 'NONE',  ( 185.0000000000000000, 175.0000000000000284, -344.0000000000001137 ) ) ;
#35874 =( BOUNDED_CURVE ( )  B_SPLINE_CURVE ( 3, ( #12873, #1339, #49235, #9525 ),
 .UNSPECIFIED., .F., .F. ) 
 B_SPLINE_CURVE_WITH_KNOTS ( ( 4, 4 ),
 ( 4.712388980384689674, 6.283185307179586232 ),
 .UNSPECIFIED. ) 
 CURVE ( )  GEOMETRIC_REPRESENTATION_ITEM ( )  RATIONAL_B_SPLINE_CURVE ( ( 1.000000000000000000, 0.8047378541243649375, 0.8047378541243649375, 1.000000000000000000 ) ) 
 REPRESENTATION_ITEM ( '' )  );
#35875 = ORIENTED_EDGE ( 'NONE', *, *, #32738, .F. ) ;
#35876 = LINE ( 'NONE', #32532, #19417 ) ;
#35877 = ORIENTED_EDGE ( 'NONE', *, *, #17092, .T. ) ;
#35878 = DIRECTION ( 'NONE',  ( -1.000000000000000000, 0.000000000000000000, 0.000000000000000000 ) ) ;
#35879 = DIRECTION ( 'NONE',  ( -1.000000000000000000, 0.000000000000000000, -0.000000000000000000 ) ) ;
#35880 = CARTESIAN_POINT ( 'NONE',  ( -7.359817328027146388, -15.16751262232800102, 2.590526750877053086 ) ) ;
#35881 = VERTEX_POINT ( 'NONE', #2025 ) ;
#35882 = ADVANCED_FACE ( 'NONE', ( #2765 ), #22524, .F. ) ;
#35883 = CARTESIAN_POINT ( 'NONE',  ( 75.05402655318509630, 2.143131898507880377E-16, -80.93171244307204404 ) ) ;
#35884 = LINE ( 'NONE', #31270, #31941 ) ;
#35885 = ORIENTED_EDGE ( 'NONE', *, *, #23285, .T. ) ;
#35886 = ORIENTED_EDGE ( 'NONE', *, *, #35644, .F. ) ;
#35887 = ORIENTED_EDGE ( 'NONE', *, *, #28790, .F. ) ;
#35888 = CARTESIAN_POINT ( 'NONE',  ( -205.6708471809678827, -1.750000000000009548, 121.8434138227750623 ) ) ;
#35889 = EDGE_CURVE ( 'NONE', #25229, #4997, #1633, .T. ) ;
#35890 = CARTESIAN_POINT ( 'NONE',  ( 33.30402655318503946, -1.750000000000010658, 120.8182875569279702 ) ) ;
#35891 = VERTEX_POINT ( 'NONE', #6622 ) ;
#35892 = ADVANCED_FACE ( 'NONE', ( #33335 ), #6369, .T. ) ;
#35893 = CARTESIAN_POINT ( 'NONE',  ( -20.40054609052957701, 26.26366202847989229, -3.760136334089591248 ) ) ;
#35894 = CARTESIAN_POINT ( 'NONE',  ( -126.6959734468149321, 0.000000000000000000, -165.0000000000000000 ) ) ;
#35895 = DIRECTION ( 'NONE',  ( 0.000000000000000000, 0.000000000000000000, 1.000000000000000000 ) ) ;
#35896 = EDGE_CURVE ( 'NONE', #35472, #2521, #34097, .T. ) ;
#35897 = CARTESIAN_POINT ( 'NONE',  ( 111.5540265531850679, 0.000000000000000000, -157.4317124430720582 ) ) ;
#35898 = DIRECTION ( 'NONE',  ( 0.000000000000000000, 1.000000000000000000, -2.537652627714643577E-15 ) ) ;
#35899 = VECTOR ( 'NONE', #10942, 1000.000000000000000 ) ;
#35900 = CARTESIAN_POINT ( 'NONE',  ( 151.5540265531850537, 1.025126265847089213, 159.0682875569279418 ) ) ;
#35901 = DIRECTION ( 'NONE',  ( 0.000000000000000000, 0.000000000000000000, 1.000000000000000000 ) ) ;
#35902 = CARTESIAN_POINT ( 'NONE',  ( -84.94597344681494633, 2.143131898507880377E-16, 165.0000000000000000 ) ) ;
#35903 = FACE_OUTER_BOUND ( 'NONE', #12202, .T. ) ;
#35904 = PLANE ( 'NONE',  #30552 ) ;
#35905 = LINE ( 'NONE', #20733, #30154 ) ;
#35906 = CARTESIAN_POINT ( 'NONE',  ( 210.0000000000000568, 2.143131898507880377E-16, -160.9317124430720298 ) ) ;
#35907 = DIRECTION ( 'NONE',  ( -0.7233555441435720601, 0.6904757466825006684, -0.000000000000000000 ) ) ;
#35908 = ORIENTED_EDGE ( 'NONE', *, *, #3553, .T. ) ;
#35909 = DIRECTION ( 'NONE',  ( 1.000000000000000000, 0.000000000000000000, 2.958228394578794270E-31 ) ) ;
#35910 = CARTESIAN_POINT ( 'NONE',  ( -128.4459734468149179, 0.000000000000000000, 165.0000000000000000 ) ) ;
#35911 = CYLINDRICAL_SURFACE ( 'NONE', #8639, 1.750000000000010214 ) ;
#35912 = EDGE_CURVE ( 'NONE', #20654, #37507, #16585, .T. ) ;
#35913 = EDGE_CURVE ( 'NONE', #37462, #19934, #29983, .T. ) ;
#35915 = VERTEX_POINT ( 'NONE', #10226 ) ;
#35914 = EDGE_CURVE ( 'NONE', #10238, #30616, #43439, .T. ) ;
#35916 = EDGE_CURVE ( 'NONE', #10114, #6437, #22277, .T. ) ;
#35917 = DIRECTION ( 'NONE',  ( 1.000000000000000000, 0.000000000000000000, 0.000000000000000000 ) ) ;
#35918 = EDGE_LOOP ( 'NONE', ( #23168, #50624, #21065, #18510, #48576, #33106 ) ) ;
#35919 = EDGE_CURVE ( 'NONE', #23987, #39539, #4907, .T. ) ;
#35920 = FACE_OUTER_BOUND ( 'NONE', #39428, .T. ) ;
#35921 = CARTESIAN_POINT ( 'NONE',  ( 181.0000000000000000, -272.4999999999999432, -355.9999999999999432 ) ) ;
#35922 = CARTESIAN_POINT ( 'NONE',  ( 183.0000000000000000, -180.9999999999999716, -350.0000000000001705 ) ) ;
#35923 = ADVANCED_FACE ( 'NONE', ( #10475 ), #18163, .T. ) ;
#35924 = ORIENTED_EDGE ( 'NONE', *, *, #36998, .F. ) ;
#35925 =( NAMED_UNIT ( * ) PLANE_ANGLE_UNIT ( ) SI_UNIT ( $, .RADIAN. ) );
#35926 = VERTEX_POINT ( 'NONE', #46850 ) ;
#35927 = VERTEX_POINT ( 'NONE', #30747 ) ;
#35928 =( BOUNDED_CURVE ( )  B_SPLINE_CURVE ( 3, ( #45376, #22052, #37730, #6159 ),
 .UNSPECIFIED., .F., .F. ) 
 B_SPLINE_CURVE_WITH_KNOTS ( ( 4, 4 ),
 ( 0.000000000000000000, 1.570796326794896558 ),
 .UNSPECIFIED. ) 
 CURVE ( )  GEOMETRIC_REPRESENTATION_ITEM ( )  RATIONAL_B_SPLINE_CURVE ( ( 1.000000000000000000, 0.8047378541243649375, 0.8047378541243649375, 1.000000000000000000 ) ) 
 REPRESENTATION_ITEM ( '' )  );
#35929 = VECTOR ( 'NONE', #46184, 1000.000000000000000 ) ;
#35930 = ORIENTED_EDGE ( 'NONE', *, *, #24045, .F. ) ;
#35931 = CARTESIAN_POINT ( 'NONE',  ( -69.99999999999940314, 17.00000000000000000, -30.00000000000000000 ) ) ;
#35932 = DIRECTION ( 'NONE',  ( 0.000000000000000000, 0.000000000000000000, 1.000000000000000000 ) ) ;
#35933 = VERTEX_POINT ( 'NONE', #210 ) ;
#35934 = DIRECTION ( 'NONE',  ( 0.000000000000000000, 0.000000000000000000, 1.000000000000000000 ) ) ;
#35935 = CARTESIAN_POINT ( 'NONE',  ( -206.6959734468149463, 0.000000000000000000, 165.0000000000000000 ) ) ;
#35936 = CARTESIAN_POINT ( 'NONE',  ( 193.3040265531851105, 1.750000000000009992, 160.8182875569279702 ) ) ;
#35937 =( BOUNDED_CURVE ( )  B_SPLINE_CURVE ( 3, ( #49534, #18526, #2867, #18269 ),
 .UNSPECIFIED., .F., .F. ) 
 B_SPLINE_CURVE_WITH_KNOTS ( ( 4, 4 ),
 ( 1.570796326794896558, 3.141592653589793116 ),
 .UNSPECIFIED. ) 
 CURVE ( )  GEOMETRIC_REPRESENTATION_ITEM ( )  RATIONAL_B_SPLINE_CURVE ( ( 1.000000000000000000, 0.8047378541243649375, 0.8047378541243649375, 1.000000000000000000 ) ) 
 REPRESENTATION_ITEM ( '' )  );
#35938 = CARTESIAN_POINT ( 'NONE',  ( -27.33593271309441874, 41.94268121623345991, -9.367992836599951190 ) ) ;
#35939 = ADVANCED_FACE ( 'NONE', ( #34860 ), #50696, .F. ) ;
#35940 = ORIENTED_EDGE ( 'NONE', *, *, #25279, .T. ) ;
#35941 = DIRECTION ( 'NONE',  ( -1.000000000000000000, 0.000000000000000000, 0.000000000000000000 ) ) ;
#35942 = EDGE_CURVE ( 'NONE', #7894, #49308, #38452, .T. ) ;
#35943 = EDGE_LOOP ( 'NONE', ( #13643, #27227, #27607, #39315 ) ) ;
#35944 = EDGE_CURVE ( 'NONE', #4997, #25229, #37712, .T. ) ;
#35945 = DIRECTION ( 'NONE',  ( 0.000000000000000000, 0.000000000000000000, -1.000000000000000000 ) ) ;
#35946 = LINE ( 'NONE', #781, #40891 ) ;
#35947 = VERTEX_POINT ( 'NONE', #27145 ) ;
#35948 = DIRECTION ( 'NONE',  ( -0.000000000000000000, -1.000000000000000000, -0.000000000000000000 ) ) ;
#35949 = CARTESIAN_POINT ( 'NONE',  ( -88.44597344681494633, 1.025126265847089657, 119.0682875569279560 ) ) ;
#35950 = B_SPLINE_SURFACE_WITH_KNOTS ( 'NONE', 3, 3, ( 
 ( #34361, #21795, #30251, #22796 ),
 ( #26657, #38476, #3286, #18687 ),
 ( #33603, #45853, #49944, #18182 ),
 ( #10739, #6143, #50191, #29743 ) ),
 .UNSPECIFIED., .F., .F., .F.,
 ( 4, 4 ),
 ( 4, 4 ),
 ( 0.000000000000000000, 1.000000000000000000 ),
 ( 0.000000000000000000, 1.000000000000000000 ),
 .UNSPECIFIED. ) ;
#35951 = EDGE_LOOP ( 'NONE', ( #36877, #24511, #10504, #33508 ) ) ;
#35952 = DIRECTION ( 'NONE',  ( 1.000000000000000000, 0.000000000000000000, 0.000000000000000000 ) ) ;
#35953 = CARTESIAN_POINT ( 'NONE',  ( 72.27890028733797578, 1.750000000000009548, 159.7931612910809065 ) ) ;
#35954 = DIRECTION ( 'NONE',  ( 0.000000000000000000, 3.186989995019654210E-49, 1.000000000000000000 ) ) ;
#35955 = ORIENTED_EDGE ( 'NONE', *, *, #25315, .F. ) ;
#35956 = CYLINDRICAL_SURFACE ( 'NONE', #41698, 1.750000000000001554 ) ;
#35957 = FACE_OUTER_BOUND ( 'NONE', #24767, .T. ) ;
#35958 = EDGE_CURVE ( 'NONE', #36804, #16909, #19439, .T. ) ;
#35959 = CARTESIAN_POINT ( 'NONE',  ( 1.011271242968683648, 0.7347315653655930312, 10.00000000000000000 ) ) ;
#35960 = ORIENTED_EDGE ( 'NONE', *, *, #21889, .F. ) ;
#35961 = ORIENTED_EDGE ( 'NONE', *, *, #18975, .F. ) ;
#35962 = SHAPE_DEFINITION_REPRESENTATION ( #24891, #34661 ) ;
#35963 = DIRECTION ( 'NONE',  ( 0.000000000000000000, 0.000000000000000000, 1.000000000000000000 ) ) ;
#35964 = CARTESIAN_POINT ( 'NONE',  ( 349.9999999999999432, -184.9999999999999716, 355.9999999999997726 ) ) ;
#35965 = AXIS2_PLACEMENT_3D ( 'NONE', #19852, #24984, #20617 ) ;
#35966 = DIRECTION ( 'NONE',  ( -0.000000000000000000, -0.000000000000000000, -1.000000000000000000 ) ) ;
#35967 = ADVANCED_FACE ( 'NONE', ( #4046 ), #38698, .F. ) ;
#35968 = CARTESIAN_POINT ( 'NONE',  ( -84.94597344681493212, -1.025126265847089657, -80.93171244307201562 ) ) ;
#35969 = DIRECTION ( 'NONE',  ( -0.000000000000000000, -0.000000000000000000, -1.000000000000000000 ) ) ;
#35970 = VERTEX_POINT ( 'NONE', #3269 ) ;
#35971 = CARTESIAN_POINT ( 'NONE',  ( 0.000000000000000000, 0.000000000000000000, 910.0000000000000000 ) ) ;
#35972 = DIRECTION ( 'NONE',  ( 0.000000000000000000, 5.664403186863042467E-17, 1.000000000000000000 ) ) ;
#35973 = CARTESIAN_POINT ( 'NONE',  ( 1.086995624458622967, -37.52050741145076529, -3.721387749823088953 ) ) ;
#35974 = CARTESIAN_POINT ( 'NONE',  ( 0.5113015165352333691, 1.175527691268683395, 9.948547179989619238 ) ) ;
#35976 = VERTEX_POINT ( 'NONE', #12245 ) ;
#35975 = EDGE_CURVE ( 'NONE', #43110, #24017, #11493, .T. ) ;
#35977 = FACE_BOUND ( 'NONE', #28267, .T. ) ;
#35978 = EDGE_CURVE ( 'NONE', #35538, #14525, #12003, .T. ) ;
#35979 = ORIENTED_EDGE ( 'NONE', *, *, #46870, .F. ) ;
#35980 = CARTESIAN_POINT ( 'NONE',  ( 9.358026734184097251, 0.000000000000000000, 0.000000000000000000 ) ) ;
#35981 = EDGE_LOOP ( 'NONE', ( #36769, #19168, #38347, #46466, #47352, #40430 ) ) ;
#35982 = DIRECTION ( 'NONE',  ( -0.000000000000000000, -0.000000000000000000, -1.000000000000000000 ) ) ;
#35983 = FACE_OUTER_BOUND ( 'NONE', #36563, .T. ) ;
#35984 = EDGE_CURVE ( 'NONE', #29962, #42166, #46596, .T. ) ;
#35985 = CARTESIAN_POINT ( 'NONE',  ( 339.9999999999999432, -166.6568542494925111, 341.6568542494923690 ) ) ;
#35986 = PLANE ( 'NONE',  #39485 ) ;
#35987 = ORIENTED_EDGE ( 'NONE', *, *, #6406, .F. ) ;
#35988 = B_SPLINE_CURVE_WITH_KNOTS ( 'NONE', 3,
 ( #38151, #37401, #30172, #10923 ),
 .UNSPECIFIED., .F., .F.,
 ( 4, 4 ),
 ( 3.878959614448864246E-18, 0.002458791966311092876 ),
 .UNSPECIFIED. ) ;
#35989 = EDGE_CURVE ( 'NONE', #11925, #39413, #35120, .T. ) ;
#35990 = ADVANCED_FACE ( 'NONE', ( #23805 ), #11247, .T. ) ;
#35992 = CARTESIAN_POINT ( 'NONE',  ( 349.9999999999999432, -180.9999999999999716, 359.9999999999997726 ) ) ;
#35991 = B_SPLINE_CURVE_WITH_KNOTS ( 'NONE', 3,
 ( #17974, #41340, #33653, #49744 ),
 .UNSPECIFIED., .F., .F.,
 ( 4, 4 ),
 ( 0.9895749839358296551, 1.000000000000000000 ),
 .UNSPECIFIED. ) ;
#35993 = CARTESIAN_POINT ( 'NONE',  ( 153.3040265531850537, 1.750000000000010658, -79.18171244307201562 ) ) ;
#35994 = ORIENTED_EDGE ( 'NONE', *, *, #34840, .F. ) ;
#35995 = DIRECTION ( 'NONE',  ( 1.000000000000000000, -4.996003610813203446E-16, -7.930164450086814785E-16 ) ) ;
#35996 = LINE ( 'NONE', #837, #1943 ) ;
#35997 = LINE ( 'NONE', #32383, #49127 ) ;
#35998 = PLANE ( 'NONE',  #12724 ) ;
#35999 = EDGE_CURVE ( 'NONE', #31506, #42696, #15597, .T. ) ;
#36000 = ORIENTED_EDGE ( 'NONE', *, *, #23018, .T. ) ;
#36001 = EDGE_LOOP ( 'NONE', ( #28786, #2482 ) ) ;
#36002 = FACE_OUTER_BOUND ( 'NONE', #44047, .T. ) ;
#36003 = VECTOR ( 'NONE', #11456, 1000.000000000000000 ) ;
#36004 = VECTOR ( 'NONE', #13607, 1000.000000000000000 ) ;
#36005 = ORIENTED_EDGE ( 'NONE', *, *, #12915, .F. ) ;
#36006 = DIRECTION ( 'NONE',  ( -1.000000000000000000, 0.000000000000000000, -0.000000000000000000 ) ) ;
#36007 = LINE ( 'NONE', #24701, #48832 ) ;
#36008 = LINE ( 'NONE', #8546, #30499 ) ;
#36009 = ORIENTED_EDGE ( 'NONE', *, *, #19414, .T. ) ;
#36011 = AXIS2_PLACEMENT_3D ( 'NONE', #41620, #10820, #26472 ) ;
#36010 = CARTESIAN_POINT ( 'NONE',  ( 15.42815683172628738, 34.17926237904582365, 7.697694107796191787 ) ) ;
#36012 = VECTOR ( 'NONE', #37705, 1000.000000000000000 ) ;
#36013 = AXIS2_PLACEMENT_3D ( 'NONE', #18703, #23067, #38741 ) ;
#36014 = PLANE ( 'NONE',  #42283 ) ;
#36015 = VECTOR ( 'NONE', #12189, 1000.000000000000000 ) ;
#36016 = CARTESIAN_POINT ( 'NONE',  ( -205.6708471809678827, -1.750000000000010436, 119.7931612910808781 ) ) ;
#36017 = VERTEX_POINT ( 'NONE', #31258 ) ;
#36018 = EDGE_LOOP ( 'NONE', ( #39191, #30967, #23382, #28042, #49259 ) ) ;
#36019 = ORIENTED_EDGE ( 'NONE', *, *, #42774, .F. ) ;
#36020 = DIRECTION ( 'NONE',  ( 3.172065745548403743E-16, 1.000000000000000000, 0.000000000000000000 ) ) ;
#36021 = CARTESIAN_POINT ( 'NONE',  ( -85.67084718096784002, -1.750000000000009326, 159.7931612910809065 ) ) ;
#36022 = LINE ( 'NONE', #863, #6866 ) ;
#36023 = VERTEX_POINT ( 'NONE', #15084 ) ;
#36024 = DIRECTION ( 'NONE',  ( 1.000000000000000000, 0.000000000000000000, 0.000000000000000000 ) ) ;
#36025 = EDGE_LOOP ( 'NONE', ( #31625, #36066 ) ) ;
#36026 = CARTESIAN_POINT ( 'NONE',  ( 0.3862712429686894766, -1.188820645368940276, -3.333333333333333481 ) ) ;
#36027 = VERTEX_POINT ( 'NONE', #39466 ) ;
#36028 = FACE_OUTER_BOUND ( 'NONE', #12562, .T. ) ;
#36029 = CARTESIAN_POINT ( 'NONE',  ( 1.782521105131670724, -0.3635605703593869920, 9.903764339332079558 ) ) ;
#36030 = DIRECTION ( 'NONE',  ( 0.000000000000000000, 1.000000000000000000, 0.000000000000000000 ) ) ;
#36031 = FILL_AREA_STYLE ('',( #48267 ) ) ;
#36032 = CARTESIAN_POINT ( 'NONE',  ( 432.7825420346616170, -62.49999999999997158, -120.5992382549688671 ) ) ;
#36033 = DIRECTION ( 'NONE',  ( 0.000000000000000000, 0.000000000000000000, -1.000000000000000000 ) ) ;
#36034 = ORIENTED_EDGE ( 'NONE', *, *, #24672, .F. ) ;
#36035 = DIRECTION ( 'NONE',  ( -1.000000000000000000, 0.000000000000000000, -7.793956916774525800E-48 ) ) ;
#36036 = CARTESIAN_POINT ( 'NONE',  ( 340.0000000000000568, 181.0000000000000284, 341.9999999999997726 ) ) ;
#36037 = PLANE ( 'NONE',  #19322 ) ;
#36038 = EDGE_CURVE ( 'NONE', #45415, #31206, #43694, .T. ) ;
#36039 = AXIS2_PLACEMENT_3D ( 'NONE', #22888, #14944, #19536 ) ;
#36040 = CARTESIAN_POINT ( 'NONE',  ( 210.0000000000000568, 0.000000000000000000, 80.81828755692798438 ) ) ;
#36041 = EDGE_CURVE ( 'NONE', #37345, #28357, #9854, .T. ) ;
#36042 = FACE_OUTER_BOUND ( 'NONE', #25974, .T. ) ;
#36043 = EDGE_LOOP ( 'NONE', ( #25268, #19662, #1655, #10361 ) ) ;
#36044 = VECTOR ( 'NONE', #45671, 1000.000000000000000 ) ;
#36045 = DIRECTION ( 'NONE',  ( 1.586032892321652236E-16, 1.000000000000000000, 6.853681917100419162E-49 ) ) ;
#36046 = ADVANCED_FACE ( 'NONE', ( #23275 ), #3790, .F. ) ;
#36047 = CARTESIAN_POINT ( 'NONE',  ( -46.69597344681494633, 1.750000000000009992, 0.8182875569279768335 ) ) ;
#36048 = EDGE_CURVE ( 'NONE', #22765, #14851, #31512, .T. ) ;
#36049 = ADVANCED_FACE ( 'NONE', ( #5042 ), #16865, .F. ) ;
#36050 = ORIENTED_EDGE ( 'NONE', *, *, #30285, .T. ) ;
#36051 = VECTOR ( 'NONE', #18785, 1000.000000000000000 ) ;
#36052 = CARTESIAN_POINT ( 'NONE',  ( 112.2789002873379758, -1.749999999999996891, 81.84341382277506227 ) ) ;
#36053 = CARTESIAN_POINT ( 'NONE',  ( 214.9999999999999432, -175.0000000000000000, 500.0000000000000000 ) ) ;
#36054 = LINE ( 'NONE', #24494, #42568 ) ;
#36055 = EDGE_CURVE ( 'NONE', #39166, #12051, #45485, .T. ) ;
#36056 = DIRECTION ( 'NONE',  ( 1.000000000000000000, 0.000000000000000000, 0.000000000000000000 ) ) ;
#36057 = ORIENTED_EDGE ( 'NONE', *, *, #5899, .T. ) ;
#36058 = VERTEX_POINT ( 'NONE', #1220 ) ;
#36059 = DIRECTION ( 'NONE',  ( -0.000000000000000000, -0.000000000000000000, -1.000000000000000000 ) ) ;
#36060 = CARTESIAN_POINT ( 'NONE',  ( 7.129058724844953510, 15.30620660340485095, 9.178419661560148768 ) ) ;
#36061 = ORIENTED_EDGE ( 'NONE', *, *, #32849, .T. ) ;
#36062 = VERTEX_POINT ( 'NONE', #5301 ) ;
#36063 = LINE ( 'NONE', #47301, #34634 ) ;
#36064 = CARTESIAN_POINT ( 'NONE',  ( 28.96803024440893992, 18.11533787072037072, 7.455576670931136185 ) ) ;
#36065 = DIRECTION ( 'NONE',  ( -0.000000000000000000, -1.000000000000000000, -0.000000000000000000 ) ) ;
#36066 = ORIENTED_EDGE ( 'NONE', *, *, #25818, .T. ) ;
#36067 = ORIENTED_EDGE ( 'NONE', *, *, #1547, .T. ) ;
#36068 = VERTEX_POINT ( 'NONE', #35872 ) ;
#36069 = CARTESIAN_POINT ( 'NONE',  ( -210.0000000000000568, 0.000000000000000000, 120.8182875569279702 ) ) ;
#36070 = AXIS2_PLACEMENT_3D ( 'NONE', #22508, #3776, #47846 ) ;
#36071 =( BOUNDED_CURVE ( )  B_SPLINE_CURVE ( 3, ( #4212, #19845, #35526, #20858 ),
 .UNSPECIFIED., .F., .F. ) 
 B_SPLINE_CURVE_WITH_KNOTS ( ( 4, 4 ),
 ( 3.141592653589793116, 4.712388980384689674 ),
 .UNSPECIFIED. ) 
 CURVE ( )  GEOMETRIC_REPRESENTATION_ITEM ( )  RATIONAL_B_SPLINE_CURVE ( ( 1.000000000000000000, 0.8047378541243649375, 0.8047378541243649375, 1.000000000000000000 ) ) 
 REPRESENTATION_ITEM ( '' )  );
#36072 = AXIS2_PLACEMENT_3D ( 'NONE', #28575, #48030, #5981 ) ;
#36073 = CARTESIAN_POINT ( 'NONE',  ( -6.906132195718435618, -3.984195806739584178, 1.626303258728256651E-16 ) ) ;
#36074 = EDGE_LOOP ( 'NONE', ( #8110, #35205, #481, #30305, #43411, #11185, #45466, #35423 ) ) ;
#36075 = ORIENTED_EDGE ( 'NONE', *, *, #30543, .F. ) ;
#36076 = DIRECTION ( 'NONE',  ( 0.000000000000000000, 0.000000000000000000, -1.000000000000000000 ) ) ;
#36077 = CIRCLE ( 'NONE', #11447, 2.000000000000001776 ) ;
#36078 = EDGE_CURVE ( 'NONE', #30725, #29367, #39970, .T. ) ;
#36080 = CARTESIAN_POINT ( 'NONE',  ( -1.250000000000000222, 0.000000000000000000, -10.00000000000000000 ) ) ;
#36079 =( BOUNDED_CURVE ( )  B_SPLINE_CURVE ( 3, ( #25971, #26459, #11061, #2349 ),
 .UNSPECIFIED., .F., .F. ) 
 B_SPLINE_CURVE_WITH_KNOTS ( ( 4, 4 ),
 ( 1.570796326794896558, 3.141592653589793116 ),
 .UNSPECIFIED. ) 
 CURVE ( )  GEOMETRIC_REPRESENTATION_ITEM ( )  RATIONAL_B_SPLINE_CURVE ( ( 1.000000000000000000, 0.8047378541243649375, 0.8047378541243649375, 1.000000000000000000 ) ) 
 REPRESENTATION_ITEM ( '' )  );
#36081 = CIRCLE ( 'NONE', #36936, 4.000000000000003553 ) ;
#36082 = FACE_OUTER_BOUND ( 'NONE', #3143, .T. ) ;
#36083 = ORIENTED_EDGE ( 'NONE', *, *, #14902, .F. ) ;
#36084 = EDGE_LOOP ( 'NONE', ( #13893, #5934, #1596, #47498, #43225, #43868 ) ) ;
#36085 = ADVANCED_FACE ( 'NONE', ( #8666 ), #12492, .F. ) ;
#36086 = CARTESIAN_POINT ( 'NONE',  ( 16.76006782980217125, -2.050259795448531541, 9.178419661560148768 ) ) ;
#36087 = SURFACE_STYLE_FILL_AREA ( #19403 ) ;
#36088 = ORIENTED_EDGE ( 'NONE', *, *, #7333, .T. ) ;
#36089 = VECTOR ( 'NONE', #47732, 1000.000000000000000 ) ;
#36090 = FACE_OUTER_BOUND ( 'NONE', #36686, .T. ) ;
#36091 = CARTESIAN_POINT ( 'NONE',  ( -14.49999999999999822, -46.51315789473684248, 5.916985404131814619 ) ) ;
#36092 = CARTESIAN_POINT ( 'NONE',  ( 350.0000000000000000, 185.0000000000000284, -356.0000000000002274 ) ) ;
#36093 = LINE ( 'NONE', #32234, #47810 ) ;
#36094 = ORIENTED_EDGE ( 'NONE', *, *, #130, .F. ) ;
#36095 = DIRECTION ( 'NONE',  ( -1.000000000000000000, 0.000000000000000000, 0.000000000000000000 ) ) ;
#36096 = CARTESIAN_POINT ( 'NONE',  ( 50.11058929355270664, -7.578863168071591438, 7.455576670931136185 ) ) ;
#36097 =( BOUNDED_CURVE ( )  B_SPLINE_CURVE ( 3, ( #43142, #309, #1055, #8006 ),
 .UNSPECIFIED., .F., .F. ) 
 B_SPLINE_CURVE_WITH_KNOTS ( ( 4, 4 ),
 ( 4.712388980384689674, 6.283185307179586232 ),
 .UNSPECIFIED. ) 
 CURVE ( )  GEOMETRIC_REPRESENTATION_ITEM ( )  RATIONAL_B_SPLINE_CURVE ( ( 1.000000000000000000, 0.8047378541243649375, 0.8047378541243649375, 1.000000000000000000 ) ) 
 REPRESENTATION_ITEM ( '' )  );
#36098 = DIRECTION ( 'NONE',  ( -1.000000000000000000, -0.000000000000000000, -0.000000000000000000 ) ) ;
#36099 = B_SPLINE_CURVE_WITH_KNOTS ( 'NONE', 3,
 ( #11790, #12793, #8201, #8711 ),
 .UNSPECIFIED., .F., .F.,
 ( 4, 4 ),
 ( 0.9688112071879413367, 0.9724175925769212858 ),
 .UNSPECIFIED. ) ;
#36100 = CARTESIAN_POINT ( 'NONE',  ( -8.445973446814962315, 1.025126265847096763, 2.568287556927999926 ) ) ;
#36101 = B_SPLINE_CURVE_WITH_KNOTS ( 'NONE', 3,
 ( #8248, #4394, #22873, #34441 ),
 .UNSPECIFIED., .F., .F.,
 ( 4, 4 ),
 ( 3.127317220692750759E-18, 0.002458791966311098948 ),
 .UNSPECIFIED. ) ;
#36102 = DIRECTION ( 'NONE',  ( 0.000000000000000000, 1.000000000000000000, -1.604368532695312981E-16 ) ) ;
#36103 = DIRECTION ( 'NONE',  ( 1.000000000000000000, 0.000000000000000000, 0.000000000000000000 ) ) ;
#36104 = DIRECTION ( 'NONE',  ( -1.000000000000000000, -0.000000000000000000, -0.000000000000000000 ) ) ;
#36105 = AXIS2_PLACEMENT_3D ( 'NONE', #9834, #29846, #6490 ) ;
#36106 = ORIENTED_EDGE ( 'NONE', *, *, #13274, .F. ) ;
#36107 = DIRECTION ( 'NONE',  ( -0.000000000000000000, -0.000000000000000000, -1.000000000000000000 ) ) ;
#36108 = AXIS2_PLACEMENT_3D ( 'NONE', #14625, #18211, #2320 ) ;
#36109 = DIRECTION ( 'NONE',  ( -1.156482317317870492E-16, 1.000000000000000000, 0.000000000000000000 ) ) ;
#36110 = EDGE_LOOP ( 'NONE', ( #34981, #37978, #21145 ) ) ;
#36111 = CARTESIAN_POINT ( 'NONE',  ( -4.531159320492035292, -41.49457383023836599, -8.080361901872242569 ) ) ;
#36112 = EDGE_CURVE ( 'NONE', #32609, #37650, #9688, .T. ) ;
#36113 = LINE ( 'NONE', #40954, #19099 ) ;
#36114 = AXIS2_PLACEMENT_3D ( 'NONE', #35643, #42786, #11261 ) ;
#36115 = VECTOR ( 'NONE', #17192, 1000.000000000000000 ) ;
#36116 = EDGE_LOOP ( 'NONE', ( #29602, #9331, #41988, #22672 ) ) ;
#36117 = AXIS2_PLACEMENT_3D ( 'NONE', #29450, #41006, #40252 ) ;
#36118 = ORIENTED_EDGE ( 'NONE', *, *, #21898, .F. ) ;
#36119 = ORIENTED_EDGE ( 'NONE', *, *, #42623, .T. ) ;
#36120 = CARTESIAN_POINT ( 'NONE',  ( 240.0000000000000000, -164.9999999999999716, 474.9999999999998863 ) ) ;
#36121 = CARTESIAN_POINT ( 'NONE',  ( -168.4459734468149747, -1.025126265847089879, 122.5682875569280128 ) ) ;
#36122 = ORIENTED_EDGE ( 'NONE', *, *, #19842, .T. ) ;
#36123 = CARTESIAN_POINT ( 'NONE',  ( 130.0000000000012221, 16.00000000000000000, 30.00000000000000000 ) ) ;
#36124 = CARTESIAN_POINT ( 'NONE',  ( -166.6959734468149463, -1.750000000000009992, 0.8182875569279768335 ) ) ;
#36125 = VERTEX_POINT ( 'NONE', #8413 ) ;
#36126 = FACE_OUTER_BOUND ( 'NONE', #33816, .T. ) ;
#36127 = VERTEX_POINT ( 'NONE', #36123 ) ;
#36128 = FACE_OUTER_BOUND ( 'NONE', #26468, .T. ) ;
#36129 = CARTESIAN_POINT ( 'NONE',  ( 155.0540265531850537, 1.025126265847088991, 162.5682875569279133 ) ) ;
#36130 = DIRECTION ( 'NONE',  ( -1.000000000000000000, -0.000000000000000000, -0.000000000000000000 ) ) ;
#36131 = ORIENTED_EDGE ( 'NONE', *, *, #45727, .F. ) ;
#36132 = DIRECTION ( 'NONE',  ( 0.000000000000000000, 0.000000000000000000, 1.000000000000000000 ) ) ;
#36133 = CARTESIAN_POINT ( 'NONE',  ( 5.320787806771834383, -8.466948512617054945, 0.000000000000000000 ) ) ;
#36134 = ORIENTED_EDGE ( 'NONE', *, *, #36211, .T. ) ;
#36135 = ORIENTED_EDGE ( 'NONE', *, *, #12404, .T. ) ;
#36136 = ORIENTED_EDGE ( 'NONE', *, *, #3986, .T. ) ;
#36137 = CARTESIAN_POINT ( 'NONE',  ( 1.011271242968694084, -0.7347315653655782652, 3.333333333333333481 ) ) ;
#36138 = CARTESIAN_POINT ( 'NONE',  ( -1.275949648750062559, 0.1226307170720055406, 9.967237415621763574 ) ) ;
#36139 = ORIENTED_EDGE ( 'NONE', *, *, #26929, .T. ) ;
#36140 = EDGE_CURVE ( 'NONE', #50570, #45326, #20201, .T. ) ;
#36141 = CIRCLE ( 'NONE', #13982, 4.000000000000003553 ) ;
#36142 = DIRECTION ( 'NONE',  ( 1.000000000000000000, 0.000000000000000000, 0.000000000000000000 ) ) ;
#36143 = CARTESIAN_POINT ( 'NONE',  ( 181.0000000000000000, -268.4999999999999432, -339.9999999999998863 ) ) ;
#36144 = CARTESIAN_POINT ( 'NONE',  ( 356.0000000000001137, -166.9999999999999432, 341.9999999999998295 ) ) ;
#36145 = VECTOR ( 'NONE', #11354, 1000.000000000000000 ) ;
#36146 = CARTESIAN_POINT ( 'NONE',  ( -126.6959734468149321, 1.749999999999997335, 80.81828755692798438 ) ) ;
#36147 = DIRECTION ( 'NONE',  ( -0.8090169943749507819, 0.5877852522924685852, 0.000000000000000000 ) ) ;
#36148 = CARTESIAN_POINT ( 'NONE',  ( 183.0000000000000000, -164.9999999999999432, -356.0000000000001705 ) ) ;
#36149 = CARTESIAN_POINT ( 'NONE',  ( 36.97942854200454832, -6.226705766838405154, 8.914903342594563185 ) ) ;
#36150 = PLANE ( 'NONE',  #44656 ) ;
#36151 = DIRECTION ( 'NONE',  ( -0.000000000000000000, -0.3790464617558786942, 0.9253776417389547593 ) ) ;
#36152 = AXIS2_PLACEMENT_3D ( 'NONE', #26365, #42009, #6862 ) ;
#36153 = LINE ( 'NONE', #4818, #8054 ) ;
#36154 = FACE_OUTER_BOUND ( 'NONE', #35943, .T. ) ;
#36155 = CARTESIAN_POINT ( 'NONE',  ( 181.0000000000000284, -180.9999999999999716, -115.0000000000001279 ) ) ;
#36156 = ORIENTED_EDGE ( 'NONE', *, *, #24112, .F. ) ;
#36157 = CARTESIAN_POINT ( 'NONE',  ( -0.8995557290265571160, -5.891360144184186076, -3.659182332138577465E-16 ) ) ;
#36158 = CARTESIAN_POINT ( 'NONE',  ( -14.29087950072019098, -9.652079258044555132, 8.727788335465566760 ) ) ;
#36159 = LINE ( 'NONE', #1261, #23391 ) ;
#36160 = CARTESIAN_POINT ( 'NONE',  ( -164.9459734468149463, -1.025126265847088991, 159.0682875569279418 ) ) ;
#36161 = ORIENTED_EDGE ( 'NONE', *, *, #17824, .F. ) ;
#36162 = SPHERICAL_SURFACE ( 'NONE', #8407, 0.5000000000000000000 ) ;
#36163 = CARTESIAN_POINT ( 'NONE',  ( 168.9999999999999716, -268.4999999999999432, -349.9999999999999432 ) ) ;
#36164 =( BOUNDED_CURVE ( )  B_SPLINE_CURVE ( 3, ( #31342, #24405, #15937, #43125 ),
 .UNSPECIFIED., .F., .F. ) 
 B_SPLINE_CURVE_WITH_KNOTS ( ( 4, 4 ),
 ( 0.000000000000000000, 1.570796326794896558 ),
 .UNSPECIFIED. ) 
 CURVE ( )  GEOMETRIC_REPRESENTATION_ITEM ( )  RATIONAL_B_SPLINE_CURVE ( ( 1.000000000000000000, 0.8047378541243649375, 0.8047378541243649375, 1.000000000000000000 ) ) 
 REPRESENTATION_ITEM ( '' )  );
#36165 = ORIENTED_EDGE ( 'NONE', *, *, #2771, .F. ) ;
#36166 = CARTESIAN_POINT ( 'NONE',  ( -1.111507796622772881, -1.112188257001367697, 9.945241992664895392 ) ) ;
#36167 = EDGE_CURVE ( 'NONE', #20022, #41021, #5168, .T. ) ;
#36168 = DIRECTION ( 'NONE',  ( -1.000000000000000000, 0.000000000000000000, 0.000000000000000000 ) ) ;
#36169 = DIRECTION ( 'NONE',  ( 1.333906992743555050E-23, -1.000000000000000000, 0.000000000000000000 ) ) ;
#36170 = EDGE_LOOP ( 'NONE', ( #9709, #28318, #1028, #25679, #44731 ) ) ;
#36171 = CARTESIAN_POINT ( 'NONE',  ( 181.0000000000000000, 8.000000000000062172, -350.0000000000001705 ) ) ;
#36172 = ORIENTED_EDGE ( 'NONE', *, *, #49084, .T. ) ;
#36173 = ORIENTED_EDGE ( 'NONE', *, *, #43441, .F. ) ;
#36174 = ADVANCED_FACE ( 'NONE', ( #13243 ), #20440, .T. ) ;
#36175 = AXIS2_PLACEMENT_3D ( 'NONE', #35304, #3454, #31191 ) ;
#36176 = EDGE_CURVE ( 'NONE', #34456, #27906, #28654, .T. ) ;
#36177 = ORIENTED_EDGE ( 'NONE', *, *, #2719, .T. ) ;
#36178 = LINE ( 'NONE', #21511, #36888 ) ;
#36179 = DIRECTION ( 'NONE',  ( 0.000000000000000000, 2.537652627714642000E-15, 1.000000000000000000 ) ) ;
#36180 = ORIENTED_EDGE ( 'NONE', *, *, #32748, .T. ) ;
#36181 = PLANE ( 'NONE',  #36904 ) ;
#36182 = FACE_OUTER_BOUND ( 'NONE', #39074, .T. ) ;
#36183 = EDGE_CURVE ( 'NONE', #5869, #41405, #27890, .T. ) ;
#36184 = DIRECTION ( 'NONE',  ( -0.2599384441937559465, -0.8000082703740970524, 0.5407575913134972101 ) ) ;
#36185 = EDGE_CURVE ( 'NONE', #44566, #45963, #20703, .T. ) ;
#36186 = VECTOR ( 'NONE', #24487, 1000.000000000000000 ) ;
#36187 = LINE ( 'NONE', #8735, #25138 ) ;
#36188 = B_SPLINE_CURVE_WITH_KNOTS ( 'NONE', 3,
 ( #22753, #38422, #3238, #18886 ),
 .UNSPECIFIED., .F., .F.,
 ( 4, 4 ),
 ( 0.003717756508417797024, 0.009855839453069397890 ),
 .UNSPECIFIED. ) ;
#36189 = ORIENTED_EDGE ( 'NONE', *, *, #44978, .F. ) ;
#36190 = LINE ( 'NONE', #48176, #37904 ) ;
#36191 = EDGE_CURVE ( 'NONE', #27608, #23039, #44280, .T. ) ;
#36192 = ORIENTED_EDGE ( 'NONE', *, *, #23396, .T. ) ;
#36193 = CARTESIAN_POINT ( 'NONE',  ( -4.641001526964560142, -33.28196331604080171, -8.016098858316199838 ) ) ;
#36194 = CARTESIAN_POINT ( 'NONE',  ( 232.4999999999999716, -169.9999999999999716, 62.29650858650038003 ) ) ;
#36195 = ORIENTED_EDGE ( 'NONE', *, *, #7057, .T. ) ;
#36196 = LINE ( 'NONE', #24641, #49912 ) ;
#36197 = DIRECTION ( 'NONE',  ( -1.000000000000000000, -6.344131455081961406E-16, 4.759647537211363479E-16 ) ) ;
#36198 = ADVANCED_FACE ( 'NONE', ( #40208 ), #1715, .T. ) ;
#36199 = ORIENTED_EDGE ( 'NONE', *, *, #24802, .F. ) ;
#36200 = EDGE_CURVE ( 'NONE', #16946, #47659, #14936, .T. ) ;
#36201 = CARTESIAN_POINT ( 'NONE',  ( -50.11058929355266400, 7.578863168071933387, 7.455576670931136185 ) ) ;
#36202 = CARTESIAN_POINT ( 'NONE',  ( -0.3370904143228943828, -0.2449105217885308716, 10.00000000000000000 ) ) ;
#36203 = LINE ( 'NONE', #789, #7389 ) ;
#36204 = DIRECTION ( 'NONE',  ( -1.000000000000000000, 0.000000000000000000, 1.860490536778032451E-50 ) ) ;
#36205 = ADVANCED_FACE ( 'NONE', ( #4551 ), #7642, .T. ) ;
#36206 = EDGE_CURVE ( 'NONE', #33842, #39985, #33284, .T. ) ;
#36207 = ORIENTED_EDGE ( 'NONE', *, *, #2908, .T. ) ;
#36208 = DIRECTION ( 'NONE',  ( 0.000000000000000000, -0.000000000000000000, -1.000000000000000000 ) ) ;
#36209 = DIRECTION ( 'NONE',  ( 0.000000000000000000, 0.000000000000000000, 1.000000000000000000 ) ) ;
#36210 = VECTOR ( 'NONE', #34233, 1000.000000000000000 ) ;
#36211 = EDGE_CURVE ( 'NONE', #18575, #19633, #29408, .T. ) ;
#36212 = CIRCLE ( 'NONE', #27189, 2.000000000000001776 ) ;
#36213 = FACE_OUTER_BOUND ( 'NONE', #20376, .T. ) ;
#36214 = VERTEX_POINT ( 'NONE', #25563 ) ;
#36215 = EDGE_LOOP ( 'NONE', ( #8557, #26529, #17401, #5989, #5866, #21152 ) ) ;
#36216 = ITEM_DEFINED_TRANSFORMATION ( 'NONE', 'NONE', #24228,  #45486 ) ;
#36217 = LINE ( 'NONE', #20043, #16323 ) ;
#36218 = CARTESIAN_POINT ( 'NONE',  ( -10.70590866674912967, 12.76446523155714985, -3.546734833711462365 ) ) ;
#36219 = CARTESIAN_POINT ( 'NONE',  ( -86.69597344681494633, -1.750000000000010658, -79.18171244307201562 ) ) ;
#36220 = PLANE ( 'NONE',  #20736 ) ;
#36221 = ORIENTED_EDGE ( 'NONE', *, *, #5899, .F. ) ;
#36222 = CARTESIAN_POINT ( 'NONE',  ( 210.0000000000000568, 0.000000000000000000, -77.43171244307200141 ) ) ;
#36224 = AXIS2_PLACEMENT_3D ( 'NONE', #35365, #50679, #4032 ) ;
#36223 = LINE ( 'NONE', #40315, #40886 ) ;
#36225 = CARTESIAN_POINT ( 'NONE',  ( 14.49999999999999822, -46.51315789473684248, 6.315789473684215949 ) ) ;
#36226 = EDGE_CURVE ( 'NONE', #15550, #10514, #9658, .T. ) ;
#36227 = FILL_AREA_STYLE_COLOUR ( '', #15782 ) ;
#36228 =( BOUNDED_CURVE ( )  B_SPLINE_CURVE ( 3, ( #29541, #29799, #10046, #44905 ),
 .UNSPECIFIED., .F., .F. ) 
 B_SPLINE_CURVE_WITH_KNOTS ( ( 4, 4 ),
 ( 1.570796326794896558, 3.141592653589793116 ),
 .UNSPECIFIED. ) 
 CURVE ( )  GEOMETRIC_REPRESENTATION_ITEM ( )  RATIONAL_B_SPLINE_CURVE ( ( 1.000000000000000000, 0.8047378541243649375, 0.8047378541243649375, 1.000000000000000000 ) ) 
 REPRESENTATION_ITEM ( '' )  );
#36229 = VERTEX_POINT ( 'NONE', #14768 ) ;
#36230 = ADVANCED_FACE ( 'NONE', ( #18601 ), #48863, .T. ) ;
#36231 = CARTESIAN_POINT ( 'NONE',  ( 115.0540265531850395, 2.143131898507847836E-16, -120.9317124430720156 ) ) ;
#36232 = ORIENTED_EDGE ( 'NONE', *, *, #29577, .T. ) ;
#36233 = EDGE_CURVE ( 'NONE', #46718, #24760, #30675, .T. ) ;
#36234 = VERTEX_POINT ( 'NONE', #37888 ) ;
#36235 = LINE ( 'NONE', #16471, #25430 ) ;
#36236 = EDGE_CURVE ( 'NONE', #5307, #26103, #13750, .T. ) ;
#36237 = CARTESIAN_POINT ( 'NONE',  ( -1.011271242968693862, 0.7347315653655780432, 3.333333333333333481 ) ) ;
#36238 =( BOUNDED_CURVE ( )  B_SPLINE_CURVE ( 3, ( #45366, #41796, #5890, #37719 ),
 .UNSPECIFIED., .F., .F. ) 
 B_SPLINE_CURVE_WITH_KNOTS ( ( 4, 4 ),
 ( 1.570796326794896558, 3.141592653589793116 ),
 .UNSPECIFIED. ) 
 CURVE ( )  GEOMETRIC_REPRESENTATION_ITEM ( )  RATIONAL_B_SPLINE_CURVE ( ( 1.000000000000000000, 0.8047378541243649375, 0.8047378541243649375, 1.000000000000000000 ) ) 
 REPRESENTATION_ITEM ( '' )  );
#36239 = DIRECTION ( 'NONE',  ( 0.000000000000000000, 0.000000000000000000, 1.000000000000000000 ) ) ;
#36240 = DIRECTION ( 'NONE',  ( 0.000000000000000000, 0.000000000000000000, 1.000000000000000000 ) ) ;
#36241 = ORIENTED_EDGE ( 'NONE', *, *, #11922, .F. ) ;
#36242 = EDGE_CURVE ( 'NONE', #23942, #41850, #9907, .T. ) ;
#36243 = LINE ( 'NONE', #40581, #11413 ) ;
#36244 = ORIENTED_EDGE ( 'NONE', *, *, #36436, .F. ) ;
#36245 = CARTESIAN_POINT ( 'NONE',  ( -84.94597344681493212, 1.025126265847089213, -0.9317124430720324924 ) ) ;
#36246 = DIRECTION ( 'NONE',  ( 0.000000000000000000, 1.000000000000000000, 0.000000000000000000 ) ) ;
#36247 = CARTESIAN_POINT ( 'NONE',  ( 193.3040265531851105, 0.000000000000000000, 165.0000000000000000 ) ) ;
#36248 = DIRECTION ( 'NONE',  ( -1.000000000000000000, -0.000000000000000000, -0.000000000000000000 ) ) ;
#36249 = VECTOR ( 'NONE', #24150, 1000.000000000000000 ) ;
#36250 = VERTEX_POINT ( 'NONE', #45282 ) ;
#36251 = ORIENTED_EDGE ( 'NONE', *, *, #31857, .T. ) ;
#36252 = CARTESIAN_POINT ( 'NONE',  ( 193.3040265531851105, 1.750000000000009992, -159.1817124430720298 ) ) ;
#36253 = ADVANCED_FACE ( 'NONE', ( #41965 ), #50606, .T. ) ;
#36254 = VECTOR ( 'NONE', #49282, 1000.000000000000000 ) ;
#36255 = ORIENTED_EDGE ( 'NONE', *, *, #41057, .T. ) ;
#36256 = AXIS2_PLACEMENT_3D ( 'NONE', #23361, #16176, #19496 ) ;
#36257 = DIRECTION ( 'NONE',  ( -1.000000000000000000, 0.000000000000000000, 0.000000000000000000 ) ) ;
#36258 = CARTESIAN_POINT ( 'NONE',  ( -88.44597344681494633, -1.025126265847089657, 42.56828755692799149 ) ) ;
#36259 = FACE_OUTER_BOUND ( 'NONE', #18280, .T. ) ;
#36260 = EDGE_CURVE ( 'NONE', #13365, #3878, #22467, .T. ) ;
#36261 = EDGE_LOOP ( 'NONE', ( #37511, #27749 ) ) ;
#36262 = CARTESIAN_POINT ( 'NONE',  ( 164.9999999999999716, 16.00000000000000000, -24.99999999999999289 ) ) ;
#36263 = FACE_OUTER_BOUND ( 'NONE', #5243, .T. ) ;
#36264 = B_SPLINE_SURFACE_WITH_KNOTS ( 'NONE', 3, 3, ( 
 ( #5039, #1467, #1215, #16860 ),
 ( #32524, #48104, #32759, #48357 ),
 ( #7321, #26321, #2702, #26063 ),
 ( #34529, #22957, #50110, #6811 ) ),
 .UNSPECIFIED., .F., .F., .F.,
 ( 4, 4 ),
 ( 4, 4 ),
 ( 0.000000000000000000, 1.000000000000000000 ),
 ( 0.000000000000000000, 1.000000000000000000 ),
 .UNSPECIFIED. ) ;
#36265 = CARTESIAN_POINT ( 'NONE',  ( 135.0000000000000000, 17.00000000000000000, -114.9999999999999858 ) ) ;
#36266 = DIRECTION ( 'NONE',  ( -1.000000000000000000, -0.000000000000000000, -0.000000000000000000 ) ) ;
#36267 = DIRECTION ( 'NONE',  ( 1.000000000000000000, 0.000000000000000000, 0.000000000000000000 ) ) ;
#36268 = EDGE_CURVE ( 'NONE', #22181, #10836, #21837, .T. ) ;
#36270 = ORIENTED_EDGE ( 'NONE', *, *, #14408, .T. ) ;
#36269 = EDGE_CURVE ( 'NONE', #39985, #50479, #19879, .T. ) ;
#36271 = ORIENTED_EDGE ( 'NONE', *, *, #44298, .F. ) ;
#36272 = VERTEX_POINT ( 'NONE', #23219 ) ;
#36273 = CARTESIAN_POINT ( 'NONE',  ( 191.5540265531851105, 0.000000000000000000, -120.9317124430720156 ) ) ;
#36274 = ADVANCED_FACE ( 'NONE', ( #3979 ), #19112, .F. ) ;
#36275 = DIRECTION ( 'NONE',  ( 1.000000000000000000, 0.000000000000000000, -0.000000000000000000 ) ) ;
#36276 = DIRECTION ( 'NONE',  ( -1.000000000000000000, 0.000000000000000000, 0.000000000000000000 ) ) ;
#36277 = CIRCLE ( 'NONE', #34610, 1.750000000000015543 ) ;
#36278 = EDGE_CURVE ( 'NONE', #35739, #29362, #18850, .T. ) ;
#36279 = ORIENTED_EDGE ( 'NONE', *, *, #2424, .F. ) ;
#36280 = DIRECTION ( 'NONE',  ( -1.000000000000000000, 0.000000000000000000, 1.860490536778032451E-50 ) ) ;
#36281 = VERTEX_POINT ( 'NONE', #7080 ) ;
#36282 = EDGE_CURVE ( 'NONE', #41447, #38146, #15533, .T. ) ;
#36283 = CARTESIAN_POINT ( 'NONE',  ( -30.12518629743573584, -14.70074613238887551, 1.847720168420772691 ) ) ;
#36284 = ORIENTED_EDGE ( 'NONE', *, *, #38250, .T. ) ;
#36285 = CARTESIAN_POINT ( 'NONE',  ( 0.000000000000000000, 0.000000000000000000, 0.000000000000000000 ) ) ;
#36286 = FACE_OUTER_BOUND ( 'NONE', #26296, .T. ) ;
#36287 = DIRECTION ( 'NONE',  ( -0.000000000000000000, -0.000000000000000000, -1.000000000000000000 ) ) ;
#36288 = PLANE ( 'NONE',  #16038 ) ;
#36289 = CARTESIAN_POINT ( 'NONE',  ( 31.44259251615245176, 38.95901822126168668, -9.367992836599951190 ) ) ;
#36290 = CARTESIAN_POINT ( 'NONE',  ( -1.086995624458622967, 37.52050741145076529, -3.721387749823088953 ) ) ;
#36291 = VECTOR ( 'NONE', #35336, 1000.000000000000000 ) ;
#36292 = CARTESIAN_POINT ( 'NONE',  ( -2.538055338523177440, -33.28424297489108596, -9.367992836599954742 ) ) ;
#36293 = EDGE_LOOP ( 'NONE', ( #32362, #31675, #21003 ) ) ;
#36294 = DIRECTION ( 'NONE',  ( 0.000000000000000000, 1.000000000000000000, 0.000000000000000000 ) ) ;
#36295 = CIRCLE ( 'NONE', #14124, 4.000000000000003553 ) ;
#36296 = LINE ( 'NONE', #44200, #25285 ) ;
#36297 = DIRECTION ( 'NONE',  ( -9.711650524620651178E-33, 1.223873602809432483E-48, -1.000000000000000000 ) ) ;
#36298 = VERTEX_POINT ( 'NONE', #42967 ) ;
#36299 = EDGE_CURVE ( 'NONE', #23256, #40728, #33365, .T. ) ;
#36300 = VECTOR ( 'NONE', #10073, 1000.000000000000000 ) ;
#36301 = CARTESIAN_POINT ( 'NONE',  ( -164.9999999999990905, 17.00000000000000000, -24.99999999999999289 ) ) ;
#36302 = VERTEX_POINT ( 'NONE', #46783 ) ;
#36303 = CARTESIAN_POINT ( 'NONE',  ( -3.345242017215803276, 2.159124855890678596, -2.642742795433417058E-16 ) ) ;
#36304 = CARTESIAN_POINT ( 'NONE',  ( 4.592425496802573972E-16, 23.48684210526316107, 3.750000000000000000 ) ) ;
#36305 = ADVANCED_BREP_SHAPE_REPRESENTATION ( '', ( #22574, #45486 ), #12706 ) ;
#36306 = ORIENTED_EDGE ( 'NONE', *, *, #14634, .F. ) ;
#36307 = CARTESIAN_POINT ( 'NONE',  ( 113.3040265531850537, -1.749999999999997335, 80.81828755692798438 ) ) ;
#36308 = CARTESIAN_POINT ( 'NONE',  ( -208.4459734468148611, -1.025126265847089657, 42.56828755692799149 ) ) ;
#36309 = DIRECTION ( 'NONE',  ( 1.000000000000000000, -0.000000000000000000, -0.000000000000000000 ) ) ;
#36310 = CARTESIAN_POINT ( 'NONE',  ( -0.3862712429686729343, -1.188820645368946050, 10.00000000000000000 ) ) ;
#36311 = EDGE_CURVE ( 'NONE', #18807, #36974, #32333, .T. ) ;
#36312 = VECTOR ( 'NONE', #33413, 1000.000000000000000 ) ;
#36313 = ORIENTED_EDGE ( 'NONE', *, *, #44291, .T. ) ;
#36314 = ORIENTED_EDGE ( 'NONE', *, *, #47983, .F. ) ;
#36315 = CARTESIAN_POINT ( 'NONE',  ( 3.975459390375365665, 0.2195152216756870167, 1.992221491942114397E-15 ) ) ;
#36316 = CARTESIAN_POINT ( 'NONE',  ( 169.0000000000000284, 175.0000000000000284, 359.9999999999998863 ) ) ;
#36317 = ORIENTED_EDGE ( 'NONE', *, *, #33357, .F. ) ;
#36318 = ORIENTED_EDGE ( 'NONE', *, *, #30292, .T. ) ;
#36319 = CYLINDRICAL_SURFACE ( 'NONE', #37105, 0.4999999999999992228 ) ;
#36320 = CARTESIAN_POINT ( 'NONE',  ( -168.4459734468149463, 0.000000000000000000, 165.0000000000000000 ) ) ;
#36321 = CARTESIAN_POINT ( 'NONE',  ( 0.3862712429686978033, -1.188820645368937834, 10.00000000000000000 ) ) ;
#36322 = FACE_OUTER_BOUND ( 'NONE', #12266, .T. ) ;
#36323 = VERTEX_POINT ( 'NONE', #30685 ) ;
#36324 = ORIENTED_EDGE ( 'NONE', *, *, #46763, .T. ) ;
#36325 = AXIS2_PLACEMENT_3D ( 'NONE', #25598, #17638, #29200 ) ;
#36326 = ORIENTED_EDGE ( 'NONE', *, *, #29694, .F. ) ;
#36327 = DIRECTION ( 'NONE',  ( -1.000000000000000000, 0.000000000000000000, 0.000000000000000000 ) ) ;
#36328 = EDGE_CURVE ( 'NONE', #41828, #8682, #15778, .T. ) ;
#36329 = EDGE_CURVE ( 'NONE', #45864, #43342, #50631, .T. ) ;
#36330 = AXIS2_PLACEMENT_3D ( 'NONE', #7439, #11017, #3562 ) ;
#36331 = CARTESIAN_POINT ( 'NONE',  ( -15.80799809827351154, 29.65358618225718956, -8.016098858316199838 ) ) ;
#36332 = ORIENTED_EDGE ( 'NONE', *, *, #43212, .F. ) ;
#36333 = ORIENTED_EDGE ( 'NONE', *, *, #5838, .F. ) ;
#36334 = CARTESIAN_POINT ( 'NONE',  ( -1.250000000000000222, 0.000000000000000000, 10.00000000000000000 ) ) ;
#36335 = CARTESIAN_POINT ( 'NONE',  ( 15.00099850811936264, 7.462898891544210933, 9.403735324607438884 ) ) ;
#36336 = EDGE_CURVE ( 'NONE', #45355, #1022, #39227, .T. ) ;
#36337 = ORIENTED_EDGE ( 'NONE', *, *, #36562, .T. ) ;
#36338 = ORIENTED_EDGE ( 'NONE', *, *, #16984, .F. ) ;
#36339 = EDGE_CURVE ( 'NONE', #15139, #24711, #11187, .T. ) ;
#36340 = CARTESIAN_POINT ( 'NONE',  ( 210.0000000000000568, 0.000000000000000000, -79.18171244307201562 ) ) ;
#36341 = FILL_AREA_STYLE_COLOUR ( '', #16592 ) ;
#36342 = ORIENTED_EDGE ( 'NONE', *, *, #29644, .T. ) ;
#36343 = EDGE_CURVE ( 'NONE', #3066, #20304, #33078, .T. ) ;
#36344 = PLANE ( 'NONE',  #10664 ) ;
#36345 = CARTESIAN_POINT ( 'NONE',  ( -48.44597344681496054, 1.025126265847089657, 119.0682875569279560 ) ) ;
#36346 = FACE_BOUND ( 'NONE', #17472, .T. ) ;
#36347 = DIRECTION ( 'NONE',  ( 0.000000000000000000, 0.000000000000000000, 1.000000000000000000 ) ) ;
#36348 = ORIENTED_EDGE ( 'NONE', *, *, #36590, .T. ) ;
#36349 = CARTESIAN_POINT ( 'NONE',  ( -30.87089393895367095, 12.69923079256638587, -9.367992836599954742 ) ) ;
#36350 = B_SPLINE_CURVE_WITH_KNOTS ( 'NONE', 3,
 ( #9142, #48096, #36111, #24801 ),
 .UNSPECIFIED., .F., .F.,
 ( 4, 4 ),
 ( 0.000000000000000000, 0.2545280377015988749 ),
 .UNSPECIFIED. ) ;
#36351 = CYLINDRICAL_SURFACE ( 'NONE', #29780, 4.000000000000003553 ) ;
#36352 = EDGE_CURVE ( 'NONE', #15608, #8293, #19856, .T. ) ;
#36353 = FACE_OUTER_BOUND ( 'NONE', #7880, .T. ) ;
#36354 = DIRECTION ( 'NONE',  ( -8.673617379884028076E-17, 1.000000000000000000, 0.000000000000000000 ) ) ;
#36355 = DIRECTION ( 'NONE',  ( 0.000000000000000000, 0.000000000000000000, 1.000000000000000000 ) ) ;
#36356 = VECTOR ( 'NONE', #45312, 1000.000000000000000 ) ;
#36357 = CARTESIAN_POINT ( 'NONE',  ( -0.8589491062558242129, -0.9799133293386017574, 9.961922210043272941 ) ) ;
#36358 = CARTESIAN_POINT ( 'NONE',  ( -44.94597344681493922, 2.143131898507880377E-16, -80.93171244307204404 ) ) ;
#36359 = DIRECTION ( 'NONE',  ( -0.000000000000000000, -0.000000000000000000, -1.000000000000000000 ) ) ;
#36360 = VECTOR ( 'NONE', #13984, 1000.000000000000000 ) ;
#36361 = ORIENTED_EDGE ( 'NONE', *, *, #30680, .T. ) ;
#36362 = CARTESIAN_POINT ( 'NONE',  ( 17.34922095635755568, 33.24536858281893359, 8.914903342594564961 ) ) ;
#36363 = AXIS2_PLACEMENT_3D ( 'NONE', #5720, #17783, #21369 ) ;
#36364 = DIRECTION ( 'NONE',  ( -1.000000000000000000, -0.000000000000000000, -0.000000000000000000 ) ) ;
#36365 = ORIENTED_EDGE ( 'NONE', *, *, #29939, .F. ) ;
#36366 = FACE_OUTER_BOUND ( 'NONE', #1699, .T. ) ;
#36367 = CARTESIAN_POINT ( 'NONE',  ( 12.35406723005396046, -11.51001571518080624, 9.178419661560148768 ) ) ;
#36368 = CARTESIAN_POINT ( 'NONE',  ( 32.27890028733795447, -1.750000000000010214, -78.15658617722490931 ) ) ;
#36369 = EDGE_LOOP ( 'NONE', ( #17213, #34482, #47877, #8117, #1297, #12914 ) ) ;
#36370 = DIRECTION ( 'NONE',  ( -3.172065784643302499E-16, -1.000000000000000000, 2.537652627714642000E-15 ) ) ;
#36371 = B_SPLINE_SURFACE_WITH_KNOTS ( 'NONE', 3, 3, ( 
 ( #38807, #15691, #6984, #11601 ),
 ( #18770, #11086, #42876, #23398 ),
 ( #38048, #30335, #39066, #30592 ),
 ( #22633, #19021, #3373, #3889 ) ),
 .UNSPECIFIED., .F., .F., .F.,
 ( 4, 4 ),
 ( 4, 4 ),
 ( 0.000000000000000000, 1.000000000000000000 ),
 ( 0.000000000000000000, 1.000000000000000000 ),
 .UNSPECIFIED. ) ;
#36372 = ORIENTED_EDGE ( 'NONE', *, *, #34809, .T. ) ;
#36373 = ORIENTED_EDGE ( 'NONE', *, *, #2693, .T. ) ;
#36374 = CARTESIAN_POINT ( 'NONE',  ( -165.0000000000000284, 16.00000000000000000, -114.9999999999999858 ) ) ;
#36375 = ADVANCED_FACE ( 'NONE', ( #50114 ), #43281, .T. ) ;
#36376 = PLANE ( 'NONE',  #39407 ) ;
#36377 =( BOUNDED_CURVE ( )  B_SPLINE_CURVE ( 3, ( #19106, #50369, #29655, #45276 ),
 .UNSPECIFIED., .F., .F. ) 
 B_SPLINE_CURVE_WITH_KNOTS ( ( 4, 4 ),
 ( 1.570796326794896558, 3.141592653589793116 ),
 .UNSPECIFIED. ) 
 CURVE ( )  GEOMETRIC_REPRESENTATION_ITEM ( )  RATIONAL_B_SPLINE_CURVE ( ( 1.000000000000000000, 0.8047378541243649375, 0.8047378541243649375, 1.000000000000000000 ) ) 
 REPRESENTATION_ITEM ( '' )  );
#36378 = AXIS2_PLACEMENT_3D ( 'NONE', #35330, #35580, #3475 ) ;
#36379 = EDGE_LOOP ( 'NONE', ( #8665, #2415, #47918, #24886 ) ) ;
#36380 = CARTESIAN_POINT ( 'NONE',  ( -1.365263087672800246, 0.5437404457009007430, 9.958264684458713489 ) ) ;
#36381 = DIRECTION ( 'NONE',  ( 0.000000000000000000, 1.000000000000000000, -1.822804496942679766E-16 ) ) ;
#36382 = ORIENTED_EDGE ( 'NONE', *, *, #29686, .F. ) ;
#36383 = ORIENTED_EDGE ( 'NONE', *, *, #21469, .F. ) ;
#36384 =( BOUNDED_CURVE ( )  B_SPLINE_CURVE ( 3, ( #44424, #17501, #33423, #17757 ),
 .UNSPECIFIED., .F., .F. ) 
 B_SPLINE_CURVE_WITH_KNOTS ( ( 4, 4 ),
 ( 0.000000000000000000, 1.570796326794896780 ),
 .UNSPECIFIED. ) 
 CURVE ( )  GEOMETRIC_REPRESENTATION_ITEM ( )  RATIONAL_B_SPLINE_CURVE ( ( 1.000000000000000000, 0.8047378541243649375, 0.8047378541243649375, 1.000000000000000000 ) ) 
 REPRESENTATION_ITEM ( '' )  );
#36385 = CARTESIAN_POINT ( 'NONE',  ( -48.44597344681495343, 0.000000000000000000, -77.43171244307198720 ) ) ;
#36386 = ORIENTED_EDGE ( 'NONE', *, *, #34611, .T. ) ;
#36387 = FACE_OUTER_BOUND ( 'NONE', #30362, .T. ) ;
#36388 = CARTESIAN_POINT ( 'NONE',  ( -126.6959734468149321, 0.000000000000000000, 165.0000000000000000 ) ) ;
#36389 = CARTESIAN_POINT ( 'NONE',  ( 210.0000000000000568, 0.000000000000000000, 120.8182875569279702 ) ) ;
#36390 = VERTEX_POINT ( 'NONE', #36582 ) ;
#36391 = CARTESIAN_POINT ( 'NONE',  ( 350.0000000000001137, 167.0000000000000000, 343.9999999999997726 ) ) ;
#36392 = CARTESIAN_POINT ( 'NONE',  ( 22.69295089195473736, 45.31600496604706052, 7.455576670931136185 ) ) ;
#36393 = VECTOR ( 'NONE', #42337, 1000.000000000000000 ) ;
#36394 = ORIENTED_EDGE ( 'NONE', *, *, #2138, .T. ) ;
#36395 = ORIENTED_EDGE ( 'NONE', *, *, #30880, .F. ) ;
#36396 = VERTEX_POINT ( 'NONE', #8601 ) ;
#36397 = CARTESIAN_POINT ( 'NONE',  ( -6.695973446814940111, -1.750000000000023315, 160.8182875569279702 ) ) ;
#36398 = CIRCLE ( 'NONE', #24081, 0.4999999999999997224 ) ;
#36399 =( BOUNDED_CURVE ( )  B_SPLINE_CURVE ( 3, ( #50181, #35128, #15358, #12255 ),
 .UNSPECIFIED., .F., .F. ) 
 B_SPLINE_CURVE_WITH_KNOTS ( ( 4, 4 ),
 ( 1.570796326794896558, 3.141592653589793116 ),
 .UNSPECIFIED. ) 
 CURVE ( )  GEOMETRIC_REPRESENTATION_ITEM ( )  RATIONAL_B_SPLINE_CURVE ( ( 1.000000000000000000, 0.8047378541243649375, 0.8047378541243649375, 1.000000000000000000 ) ) 
 REPRESENTATION_ITEM ( '' )  );
#36400 = DIRECTION ( 'NONE',  ( -0.000000000000000000, -0.000000000000000000, -1.000000000000000000 ) ) ;
#36401 = VERTEX_POINT ( 'NONE', #909 ) ;
#36402 = EDGE_CURVE ( 'NONE', #6007, #41927, #10083, .T. ) ;
#36403 = DIRECTION ( 'NONE',  ( -1.000000000000000000, -0.000000000000000000, -0.000000000000000000 ) ) ;
#36404 = VECTOR ( 'NONE', #3054, 1000.000000000000000 ) ;
#36405 = EDGE_CURVE ( 'NONE', #20673, #47737, #28095, .T. ) ;
#36406 = CARTESIAN_POINT ( 'NONE',  ( -4.945973446814903696, 2.143131898507912917E-16, -0.9317124430720524764 ) ) ;
#36407 = CARTESIAN_POINT ( 'NONE',  ( 111.5540265531850537, -1.025126265847081664, -157.4317124430720582 ) ) ;
#36408 = FACE_OUTER_BOUND ( 'NONE', #2051, .T. ) ;
#36409 = DIRECTION ( 'NONE',  ( 0.000000000000000000, 0.000000000000000000, -1.000000000000000000 ) ) ;
#36410 = EDGE_CURVE ( 'NONE', #6960, #15590, #5935, .T. ) ;
#36411 = CARTESIAN_POINT ( 'NONE',  ( -88.44597344681494633, 1.025126265847089435, -117.4317124430720156 ) ) ;
#36412 = CARTESIAN_POINT ( 'NONE',  ( -207.7210997126620384, 1.750000000000009548, -160.2068387089191219 ) ) ;
#36413 = DIRECTION ( 'NONE',  ( -0.000000000000000000, -0.000000000000000000, -1.000000000000000000 ) ) ;
#36414 = DIRECTION ( 'NONE',  ( -0.000000000000000000, -0.000000000000000000, -1.000000000000000000 ) ) ;
#36415 = UNCERTAINTY_MEASURE_WITH_UNIT (LENGTH_MEASURE( 1.000000000000000082E-05 ), #26535, 'distance_accuracy_value', 'NONE');
#36416 = AXIS2_PLACEMENT_3D ( 'NONE', #36921, #36671, #48386 ) ;
#36417 = DIRECTION ( 'NONE',  ( -0.000000000000000000, -1.000000000000000000, -0.000000000000000000 ) ) ;
#36418 = ORIENTED_EDGE ( 'NONE', *, *, #46290, .T. ) ;
#36419 = DIRECTION ( 'NONE',  ( 0.9908916497796512735, 0.000000000000000000, 0.1346615698592613375 ) ) ;
#36420 = LINE ( 'NONE', #42193, #25354 ) ;
#36421 = LINE ( 'NONE', #21000, #27500 ) ;
#36422 = CARTESIAN_POINT ( 'NONE',  ( -9.999999999999921840, -0.04964634317306688277, 9.296265711052123848 ) ) ;
#36423 = ORIENTED_EDGE ( 'NONE', *, *, #19252, .T. ) ;
#36424 = CARTESIAN_POINT ( 'NONE',  ( 183.0000000000000284, -180.9999999999999716, -115.0000000000001279 ) ) ;
#36425 = CARTESIAN_POINT ( 'NONE',  ( 325.0507910275983932, -325.0507910275983932, 321.8002831173224649 ) ) ;
#36426 = AXIS2_PLACEMENT_3D ( 'NONE', #28655, #28413, #9908 ) ;
#36427 = ORIENTED_EDGE ( 'NONE', *, *, #5298, .T. ) ;
#36428 = LINE ( 'NONE', #43842, #7334 ) ;
#36429 = VECTOR ( 'NONE', #9020, 1000.000000000000000 ) ;
#36430 = PLANE ( 'NONE',  #33169 ) ;
#36431 = CARTESIAN_POINT ( 'NONE',  ( 168.9999999999998579, -166.9999999999999432, -340.0000000000001137 ) ) ;
#36432 = ORIENTED_EDGE ( 'NONE', *, *, #12452, .F. ) ;
#36433 = ORIENTED_EDGE ( 'NONE', *, *, #8625, .F. ) ;
#36434 = VERTEX_POINT ( 'NONE', #20135 ) ;
#36435 = AXIS2_PLACEMENT_3D ( 'NONE', #25651, #45620, #37226 ) ;
#36436 = EDGE_CURVE ( 'NONE', #27396, #18807, #31742, .T. ) ;
#36437 = ORIENTED_EDGE ( 'NONE', *, *, #9943, .F. ) ;
#36438 = CARTESIAN_POINT ( 'NONE',  ( 193.3040265531851105, -1.750000000000010658, 80.81828755692798438 ) ) ;
#36439 = CARTESIAN_POINT ( 'NONE',  ( -23.82716369509181575, -44.49195112875988656, 8.356839323120299312 ) ) ;
#36440 =( BOUNDED_CURVE ( )  B_SPLINE_CURVE ( 3, ( #50275, #14925, #30846, #15433 ),
 .UNSPECIFIED., .F., .F. ) 
 B_SPLINE_CURVE_WITH_KNOTS ( ( 4, 4 ),
 ( 3.141592653589793116, 4.712388980384689674 ),
 .UNSPECIFIED. ) 
 CURVE ( )  GEOMETRIC_REPRESENTATION_ITEM ( )  RATIONAL_B_SPLINE_CURVE ( ( 1.000000000000000000, 0.8047378541243649375, 0.8047378541243649375, 1.000000000000000000 ) ) 
 REPRESENTATION_ITEM ( '' )  );
#36441 = ORIENTED_EDGE ( 'NONE', *, *, #24735, .F. ) ;
#36442 = CARTESIAN_POINT ( 'NONE',  ( 360.0000000000000000, -169.0000000000000568, -344.0000000000002842 ) ) ;
#36443 = DIRECTION ( 'NONE',  ( 0.000000000000000000, 0.000000000000000000, 1.000000000000000000 ) ) ;
#36444 = PLANE ( 'NONE',  #37239 ) ;
#36445 = FACE_OUTER_BOUND ( 'NONE', #45136, .T. ) ;
#36446 = ORIENTED_EDGE ( 'NONE', *, *, #15994, .T. ) ;
#36447 = PLANE ( 'NONE',  #35455 ) ;
#36448 = VECTOR ( 'NONE', #1190, 1000.000000000000000 ) ;
#36449 = EDGE_LOOP ( 'NONE', ( #44091, #26531, #43494, #36796, #24212, #33427, #39160, #8480, #49293, #40288, #23151, #42073 ) ) ;
#36450 = CARTESIAN_POINT ( 'NONE',  ( 164.9999999999999716, -9.999999999999953815, -350.0000000000001705 ) ) ;
#36451 = CARTESIAN_POINT ( 'NONE',  ( 358.0000000000000000, -169.0000000000001137, -344.0000000000002842 ) ) ;
#36452 = TOROIDAL_SURFACE ( 'NONE', #24981, 14.00000000000000355, 20.99999999999999289 ) ;
#36453 = VERTEX_POINT ( 'NONE', #28850 ) ;
#36454 = ORIENTED_EDGE ( 'NONE', *, *, #14862, .F. ) ;
#36455 = CARTESIAN_POINT ( 'NONE',  ( -4.945973446814916130, 1.025126265847097429, 79.06828755692792754 ) ) ;
#36456 = CARTESIAN_POINT ( 'NONE',  ( -48.44597344681495343, 0.000000000000000000, 2.568287556927978166 ) ) ;
#36457 = EDGE_LOOP ( 'NONE', ( #15710, #48499, #6836, #6447 ) ) ;
#36458 = CYLINDRICAL_SURFACE ( 'NONE', #16916, 1.750000000000015543 ) ;
#36459 = DIRECTION ( 'NONE',  ( -0.000000000000000000, -3.186989995019654210E-49, -1.000000000000000000 ) ) ;
#36460 = DIRECTION ( 'NONE',  ( 0.000000000000000000, -2.537652627714643577E-15, -1.000000000000000000 ) ) ;
#36461 = CARTESIAN_POINT ( 'NONE',  ( 15.73090589902275482, 29.60029367929053024, 1.847720168420772691 ) ) ;
#36462 = ORIENTED_EDGE ( 'NONE', *, *, #33903, .T. ) ;
#36463 = AXIS2_PLACEMENT_3D ( 'NONE', #18673, #18170, #14836 ) ;
#36464 = LINE ( 'NONE', #16682, #5656 ) ;
#36466 = EDGE_CURVE ( 'NONE', #2880, #27411, #4742, .T. ) ;
#36465 = CARTESIAN_POINT ( 'NONE',  ( -88.44597344681494633, 1.025126265847089657, -80.93171244307201562 ) ) ;
#36467 = CARTESIAN_POINT ( 'NONE',  ( 151.5540265531850537, 1.025126265847089213, 162.5682875569279133 ) ) ;
#36468 = ORIENTED_EDGE ( 'NONE', *, *, #9025, .T. ) ;
#36469 = AXIS2_PLACEMENT_3D ( 'NONE', #43812, #4809, #48380 ) ;
#36470 = ORIENTED_EDGE ( 'NONE', *, *, #8476, .T. ) ;
#36471 = ITEM_DEFINED_TRANSFORMATION ( 'NONE', 'NONE', #31598,  #45486 ) ;
#36472 = CARTESIAN_POINT ( 'NONE',  ( 35.05402655318504657, 2.143131898507880377E-16, -160.9317124430720582 ) ) ;
#36473 = CARTESIAN_POINT ( 'NONE',  ( 115.0540265531850395, -1.025126265847081664, -77.43171244307201562 ) ) ;
#36474 = CARTESIAN_POINT ( 'NONE',  ( -128.4459734468149179, 0.000000000000000000, 82.56828755692795596 ) ) ;
#36475 = CARTESIAN_POINT ( 'NONE',  ( 344.0000000000000568, -167.0000000000001137, 342.0000000000000000 ) ) ;
#36476 = EDGE_LOOP ( 'NONE', ( #34637, #11994 ) ) ;
#36477 = DIRECTION ( 'NONE',  ( -0.000000000000000000, -0.000000000000000000, -1.000000000000000000 ) ) ;
#36478 = ADVANCED_FACE ( 'NONE', ( #20644 ), #36319, .T. ) ;
#36479 = DIRECTION ( 'NONE',  ( 7.793956916774525800E-48, 0.000000000000000000, 1.000000000000000000 ) ) ;
#36480 = LINE ( 'NONE', #16965, #6139 ) ;
#36481 = ADVANCED_FACE ( 'NONE', ( #35825 ), #1162, .F. ) ;
#36482 = ORIENTED_EDGE ( 'NONE', *, *, #1734, .F. ) ;
#36483 = VECTOR ( 'NONE', #38950, 1000.000000000000000 ) ;
#36484 = CARTESIAN_POINT ( 'NONE',  ( 192.2789002873380184, -1.750000000000010214, 119.7931612910808781 ) ) ;
#36485 = EDGE_LOOP ( 'NONE', ( #38769, #48014, #43993, #36734 ) ) ;
#36486 = DIRECTION ( 'NONE',  ( 1.000000000000000000, -1.586032892321652236E-16, -1.586032892321651989E-16 ) ) ;
#36487 = AXIS2_PLACEMENT_3D ( 'NONE', #25225, #28571, #12910 ) ;
#36488 = VERTEX_POINT ( 'NONE', #16800 ) ;
#36489 = DIRECTION ( 'NONE',  ( 0.000000000000000000, 2.537652627714642000E-15, 1.000000000000000000 ) ) ;
#36490 = CARTESIAN_POINT ( 'NONE',  ( 0.000000000000000000, -250.0000000000000000, 225.0000000000000000 ) ) ;
#36491 = EDGE_CURVE ( 'NONE', #48821, #8324, #8353, .T. ) ;
#36492 = CARTESIAN_POINT ( 'NONE',  ( -204.9459734468149463, 2.143131898507880377E-16, -157.4317124430720582 ) ) ;
#36493 = CARTESIAN_POINT ( 'NONE',  ( 135.0000000000003411, 16.00000000000000000, -60.00000000000000000 ) ) ;
#36494 = EDGE_CURVE ( 'NONE', #32259, #47711, #1414, .T. ) ;
#36495 = ORIENTED_EDGE ( 'NONE', *, *, #40577, .F. ) ;
#36496 = ADVANCED_FACE ( 'NONE', ( #48300 ), #40408, .T. ) ;
#36497 = COLOUR_RGB ( '',0.7921568627450980005, 0.8196078431372548767, 0.9333333333333333481 ) ;
#36498 = CARTESIAN_POINT ( 'NONE',  ( -126.6959734468149321, 1.749999999999996891, 0.8182875569279768335 ) ) ;
#36499 = ORIENTED_EDGE ( 'NONE', *, *, #17362, .T. ) ;
#36500 = CARTESIAN_POINT ( 'NONE',  ( -166.6959734468149463, 1.750000000000010214, 40.81828755692798438 ) ) ;
#36501 = AXIS2_PLACEMENT_3D ( 'NONE', #21207, #48615, #13506 ) ;
#36502 = CARTESIAN_POINT ( 'NONE',  ( 36.08557433729230013, -35.58569447144767395, 7.455576670931136185 ) ) ;
#36503 = PLANE ( 'NONE',  #16391 ) ;
#36504 = CARTESIAN_POINT ( 'NONE',  ( -128.4459734468149179, 0.000000000000000000, -117.4317124430720725 ) ) ;
#36505 = CARTESIAN_POINT ( 'NONE',  ( 47.22310614333766665, 16.46562252335956344, -3.760136334089591248 ) ) ;
#36506 = VERTEX_POINT ( 'NONE', #39912 ) ;
#36507 = PRODUCT_DEFINITION_FORMATION_WITH_SPECIFIED_SOURCE ( 'ANY', '', #33111, .NOT_KNOWN. ) ;
#36508 = ORIENTED_EDGE ( 'NONE', *, *, #43212, .T. ) ;
#36509 = CARTESIAN_POINT ( 'NONE',  ( 168.9999999999999716, -164.9999999999999432, 355.9999999999998863 ) ) ;
#36510 = AXIS2_PLACEMENT_3D ( 'NONE', #23187, #7285, #43198 ) ;
#36511 = EDGE_LOOP ( 'NONE', ( #30756, #22158, #33849, #31268, #19066, #17723, #19186, #18488 ) ) ;
#36512 = PLANE ( 'NONE',  #17577 ) ;
#36513 = DIRECTION ( 'NONE',  ( 1.000000000000000000, 0.000000000000000000, 0.000000000000000000 ) ) ;
#36514 = DIRECTION ( 'NONE',  ( -1.000000000000000000, 0.000000000000000000, 0.000000000000000000 ) ) ;
#36515 = EDGE_LOOP ( 'NONE', ( #45705, #49999, #3724, #18311, #47860, #14907 ) ) ;
#36516 = DIRECTION ( 'NONE',  ( -0.000000000000000000, -0.000000000000000000, -1.000000000000000000 ) ) ;
#36517 = EDGE_CURVE ( 'NONE', #5465, #11313, #50127, .T. ) ;
#36518 = CARTESIAN_POINT ( 'NONE',  ( 350.0000000000000000, -168.9999999999999432, -360.0000000000002274 ) ) ;
#36519 = CARTESIAN_POINT ( 'NONE',  ( -33.43156050989129824, 4.370686678976795747, 8.807470649214879543 ) ) ;
#36520 = DIRECTION ( 'NONE',  ( -7.793956916774524585E-48, 0.000000000000000000, -1.000000000000000000 ) ) ;
#36521 = LINE ( 'NONE', #25711, #23923 ) ;
#36522 = VECTOR ( 'NONE', #40089, 1000.000000000000000 ) ;
#36523 = EDGE_CURVE ( 'NONE', #28864, #39878, #12190, .T. ) ;
#36524 = VERTEX_POINT ( 'NONE', #12434 ) ;
#36525 = EDGE_CURVE ( 'NONE', #29858, #36660, #36063, .T. ) ;
#36526 = ORIENTED_EDGE ( 'NONE', *, *, #10874, .T. ) ;
#36527 = ORIENTED_EDGE ( 'NONE', *, *, #300, .F. ) ;
#36528 = VECTOR ( 'NONE', #25607, 1000.000000000000000 ) ;
#36529 = CARTESIAN_POINT ( 'NONE',  ( 0.000000000000000000, 50.00000000000000000, 0.000000000000000000 ) ) ;
#36530 = EDGE_CURVE ( 'NONE', #21643, #21466, #267, .T. ) ;
#36531 = FACE_OUTER_BOUND ( 'NONE', #29221, .T. ) ;
#36532 = VECTOR ( 'NONE', #40060, 1000.000000000000000 ) ;
#36533 = CARTESIAN_POINT ( 'NONE',  ( 193.3040265531851105, 1.750000000000009992, 0.8182875569279768335 ) ) ;
#36534 = EDGE_LOOP ( 'NONE', ( #8371, #11701, #22073, #37073, #1714, #24572 ) ) ;
#36535 = ADVANCED_FACE ( 'NONE', ( #15156 ), #46421, .F. ) ;
#36536 = DIRECTION ( 'NONE',  ( -2.958228394578794708E-31, 0.000000000000000000, 1.000000000000000000 ) ) ;
#36537 = EDGE_LOOP ( 'NONE', ( #26527, #11353, #26784, #7329 ) ) ;
#36538 = DIRECTION ( 'NONE',  ( 1.000000000000000000, 0.000000000000000000, 0.000000000000000000 ) ) ;
#36539 = CARTESIAN_POINT ( 'NONE',  ( 0.4166666666666669072, 0.000000000000000000, 10.00000000000000000 ) ) ;
#36540 = CIRCLE ( 'NONE', #47127, 2.000000000000001776 ) ;
#36541 = CARTESIAN_POINT ( 'NONE',  ( -164.9459734468149463, 2.143131898507880377E-16, 165.0000000000000000 ) ) ;
#36542 = CARTESIAN_POINT ( 'NONE',  ( 155.0540265531850537, 2.143131898507880377E-16, -157.4317124430720582 ) ) ;
#36543 = AXIS2_PLACEMENT_3D ( 'NONE', #9871, #44496, #6016 ) ;
#36544 = CARTESIAN_POINT ( 'NONE',  ( -126.6959734468149321, 0.000000000000000000, 165.0000000000000000 ) ) ;
#36545 = CIRCLE ( 'NONE', #21746, 3.749999999999975575 ) ;
#36546 = CARTESIAN_POINT ( 'NONE',  ( 183.0000000000000000, -93.49999999999998579, -115.0000000000001563 ) ) ;
#36547 = VERTEX_POINT ( 'NONE', #9603 ) ;
#36548 = CARTESIAN_POINT ( 'NONE',  ( -48.44597344681495343, 0.000000000000000000, 2.568287556927978166 ) ) ;
#36549 =( BOUNDED_CURVE ( )  B_SPLINE_CURVE ( 3, ( #24348, #13019, #47885, #17134 ),
 .UNSPECIFIED., .F., .F. ) 
 B_SPLINE_CURVE_WITH_KNOTS ( ( 4, 4 ),
 ( 3.141592653589793116, 4.712388980384689674 ),
 .UNSPECIFIED. ) 
 CURVE ( )  GEOMETRIC_REPRESENTATION_ITEM ( )  RATIONAL_B_SPLINE_CURVE ( ( 1.000000000000000000, 0.8047378541243649375, 0.8047378541243649375, 1.000000000000000000 ) ) 
 REPRESENTATION_ITEM ( '' )  );
#36550 = CYLINDRICAL_SURFACE ( 'NONE', #36619, 1.750000000000036193 ) ;
#36551 = FACE_OUTER_BOUND ( 'NONE', #50311, .T. ) ;
#36552 = CARTESIAN_POINT ( 'NONE',  ( -15.57957361750255565, -5.755602074545403291, 3.266473740018926541 ) ) ;
#36553 = CIRCLE ( 'NONE', #45170, 4.000000000000003553 ) ;
#36554 = LINE ( 'NONE', #43709, #20661 ) ;
#36555 = ORIENTED_EDGE ( 'NONE', *, *, #16629, .F. ) ;
#36556 = CARTESIAN_POINT ( 'NONE',  ( 224.9999999999999716, -164.9999999999999716, 62.29650858650038003 ) ) ;
#36557 = ORIENTED_EDGE ( 'NONE', *, *, #39649, .T. ) ;
#36558 = CARTESIAN_POINT ( 'NONE',  ( -119.9999999999990905, 17.00000000000000000, -24.99999999999999289 ) ) ;
#36559 = LINE ( 'NONE', #1395, #12701 ) ;
#36560 = EDGE_CURVE ( 'NONE', #38860, #16290, #22601, .T. ) ;
#36561 = CARTESIAN_POINT ( 'NONE',  ( 130.0000000000021032, 17.00000000000000000, 95.00000000000000000 ) ) ;
#36562 = EDGE_CURVE ( 'NONE', #12204, #5465, #11309, .T. ) ;
#36563 = EDGE_LOOP ( 'NONE', ( #19336, #3252, #20164, #19953 ) ) ;
#36564 = ORIENTED_EDGE ( 'NONE', *, *, #21983, .T. ) ;
#36565 = EDGE_CURVE ( 'NONE', #39650, #30823, #23100, .T. ) ;
#36566 = VECTOR ( 'NONE', #49237, 1000.000000000000000 ) ;
#36567 = ADVANCED_FACE ( 'NONE', ( #40904 ), #17803, .T. ) ;
#36568 = CARTESIAN_POINT ( 'NONE',  ( 169.0000000000000000, 2.775557561562891351E-14, -97.00000000000014211 ) ) ;
#36569 = CARTESIAN_POINT ( 'NONE',  ( 27.31081730472575941, 41.96092862852144378, 3.199614146704519602 ) ) ;
#36570 = VECTOR ( 'NONE', #19119, 1000.000000000000000 ) ;
#36571 = PLANE ( 'NONE',  #33583 ) ;
#36572 = ADVANCED_FACE ( 'NONE', ( #32971 ), #5744, .F. ) ;
#36573 = CYLINDRICAL_SURFACE ( 'NONE', #20121, 1.750000000000015543 ) ;
#36574 = EDGE_CURVE ( 'NONE', #28586, #44854, #3343, .T. ) ;
#36575 = VECTOR ( 'NONE', #30401, 1000.000000000000000 ) ;
#36576 = ORIENTED_EDGE ( 'NONE', *, *, #15297, .T. ) ;
#36577 = ORIENTED_EDGE ( 'NONE', *, *, #11245, .T. ) ;
#36578 = CARTESIAN_POINT ( 'NONE',  ( -4.641001526964561918, -33.28196331604080171, -8.016098858316205167 ) ) ;
#36579 = CARTESIAN_POINT ( 'NONE',  ( 46.11867747200574996, -19.86470446310233484, -8.016098858316199838 ) ) ;
#36580 = ORIENTED_EDGE ( 'NONE', *, *, #5031, .T. ) ;
#36581 = ORIENTED_EDGE ( 'NONE', *, *, #22663, .F. ) ;
#36582 = CARTESIAN_POINT ( 'NONE',  ( -1.080000014127418639, -0.7606467978654640749, 9.943883492372872723 ) ) ;
#36583 = CARTESIAN_POINT ( 'NONE',  ( -86.69597344681496054, 0.000000000000000000, 165.0000000000000000 ) ) ;
#36584 = FACE_OUTER_BOUND ( 'NONE', #37060, .T. ) ;
#36585 = CARTESIAN_POINT ( 'NONE',  ( 356.0000000000000568, 185.0000000000001137, 359.9999999999998295 ) ) ;
#36586 = VECTOR ( 'NONE', #15175, 1000.000000000000000 ) ;
#36587 = ORIENTED_EDGE ( 'NONE', *, *, #15821, .F. ) ;
#36588 = ORIENTED_EDGE ( 'NONE', *, *, #35253, .F. ) ;
#36589 = VERTEX_POINT ( 'NONE', #33469 ) ;
#36590 = EDGE_CURVE ( 'NONE', #269, #39568, #40344, .T. ) ;
#36591 = AXIS2_PLACEMENT_3D ( 'NONE', #20435, #35869, #697 ) ;
#36592 = DIRECTION ( 'NONE',  ( 1.000000000000000000, 0.000000000000000000, 0.000000000000000000 ) ) ;
#36593 = EDGE_CURVE ( 'NONE', #11397, #32226, #18989, .T. ) ;
#36594 = EDGE_CURVE ( 'NONE', #37650, #17197, #48809, .T. ) ;
#36595 = DIRECTION ( 'NONE',  ( -1.000000000000000000, -0.000000000000000000, -0.000000000000000000 ) ) ;
#36596 = ORIENTED_EDGE ( 'NONE', *, *, #35665, .F. ) ;
#36597 = ORIENTED_EDGE ( 'NONE', *, *, #3692, .T. ) ;
#36598 = CARTESIAN_POINT ( 'NONE',  ( -7.359817328027146388, -15.16751262232800102, 2.590526750877053086 ) ) ;
#36599 = CARTESIAN_POINT ( 'NONE',  ( 355.9999999999999432, -185.0000000000000284, 359.9999999999998295 ) ) ;
#36600 = VERTEX_POINT ( 'NONE', #34414 ) ;
#36601 = ORIENTED_EDGE ( 'NONE', *, *, #22880, .F. ) ;
#36602 = CARTESIAN_POINT ( 'NONE',  ( 33.43156050989131955, -4.370686678976570150, 8.807470649214879543 ) ) ;
#36603 = FACE_OUTER_BOUND ( 'NONE', #38496, .T. ) ;
#36604 = ORIENTED_EDGE ( 'NONE', *, *, #37898, .T. ) ;
#36605 = CIRCLE ( 'NONE', #43126, 4.000000000000003553 ) ;
#36606 = CYLINDRICAL_SURFACE ( 'NONE', #6848, 1.750000000000001554 ) ;
#36607 = CARTESIAN_POINT ( 'NONE',  ( 35.00000000000216716, 17.00000000000000000, 95.00000000000000000 ) ) ;
#36608 = CARTESIAN_POINT ( 'NONE',  ( 185.0000000000000000, 165.0000000000000000, -356.0000000000001705 ) ) ;
#36609 = AXIS2_PLACEMENT_3D ( 'NONE', #30307, #34677, #26451 ) ;
#36610 = CARTESIAN_POINT ( 'NONE',  ( 183.0000000000000284, -180.9999999999993747, -115.0000000000001279 ) ) ;
#36611 = AXIS2_PLACEMENT_3D ( 'NONE', #21722, #44114, #48879 ) ;
#36612 = ORIENTED_EDGE ( 'NONE', *, *, #15637, .T. ) ;
#36613 = EDGE_CURVE ( 'NONE', #50318, #31422, #13695, .T. ) ;
#36614 = CARTESIAN_POINT ( 'NONE',  ( -33.01266944765060174, 5.813986777101691317, 1.847720168420772691 ) ) ;
#36615 = CYLINDRICAL_SURFACE ( 'NONE', #9306, 1.750000000000036193 ) ;
#36616 = CARTESIAN_POINT ( 'NONE',  ( -3.695802964311593719, -9.324875653452746604, 9.390253821402618328 ) ) ;
#36617 = PLANE ( 'NONE',  #32341 ) ;
#36618 = VECTOR ( 'NONE', #22346, 1000.000000000000000 ) ;
#36619 = AXIS2_PLACEMENT_3D ( 'NONE', #8696, #38987, #47131 ) ;
#36620 = EDGE_CURVE ( 'NONE', #35055, #2039, #36695, .T. ) ;
#36621 = DIRECTION ( 'NONE',  ( 0.000000000000000000, 0.000000000000000000, 1.000000000000000000 ) ) ;
#36622 = CARTESIAN_POINT ( 'NONE',  ( -128.4459734468149463, 1.025126265847081886, 79.06828755692797017 ) ) ;
#36623 = CARTESIAN_POINT ( 'NONE',  ( 33.89193117067293315, 33.89193117067293315, 910.0000000000000000 ) ) ;
#36624 = B_SPLINE_CURVE_WITH_KNOTS ( 'NONE', 3,
 ( #36133, #977, #4060, #12260 ),
 .UNSPECIFIED., .F., .F.,
 ( 4, 4 ),
 ( 0.001924139378288104675, 0.008062652406780950951 ),
 .UNSPECIFIED. ) ;
#36625 = CARTESIAN_POINT ( 'NONE',  ( 130.0000000000002842, 16.00000000000000000, -60.00000000000000000 ) ) ;
#36626 = AXIS2_PLACEMENT_3D ( 'NONE', #8037, #27778, #35759 ) ;
#36627 = ORIENTED_EDGE ( 'NONE', *, *, #5195, .F. ) ;
#36628 = CARTESIAN_POINT ( 'NONE',  ( 360.0000000000000568, 165.0000000000000000, -106.0000000000001990 ) ) ;
#36629 = EDGE_CURVE ( 'NONE', #3137, #38752, #9982, .T. ) ;
#36630 = EDGE_CURVE ( 'NONE', #2449, #19301, #41979, .T. ) ;
#36631 = CARTESIAN_POINT ( 'NONE',  ( 155.0540265531850537, 1.025126265847089657, 42.56828755692799149 ) ) ;
#36632 = ORIENTED_EDGE ( 'NONE', *, *, #20678, .T. ) ;
#36633 = CARTESIAN_POINT ( 'NONE',  ( 185.0000000000000284, -174.9999999999999716, -99.00000000000014211 ) ) ;
#36634 = CARTESIAN_POINT ( 'NONE',  ( 13.59579750444771307, -10.60877755095900632, 8.727788335465566760 ) ) ;
#36635 = CARTESIAN_POINT ( 'NONE',  ( 85.00000000000213163, 16.00000000000000000, 95.00000000000000000 ) ) ;
#36636 = EDGE_CURVE ( 'NONE', #23942, #18077, #28432, .T. ) ;
#36637 = ORIENTED_EDGE ( 'NONE', *, *, #2950, .F. ) ;
#36638 = CYLINDRICAL_SURFACE ( 'NONE', #11024, 50.00000000000000000 ) ;
#36639 = ORIENTED_EDGE ( 'NONE', *, *, #9948, .F. ) ;
#36640 = LINE ( 'NONE', #36374, #38191 ) ;
#36641 = EDGE_CURVE ( 'NONE', #16065, #6629, #30558, .T. ) ;
#36642 = DIRECTION ( 'NONE',  ( -1.000000000000000000, 0.000000000000000000, 0.000000000000000000 ) ) ;
#36643 = ADVANCED_FACE ( 'NONE', ( #43352 ), #31589, .T. ) ;
#36644 = AXIS2_PLACEMENT_3D ( 'NONE', #22975, #28544, #11957 ) ;
#36645 = ORIENTED_EDGE ( 'NONE', *, *, #45591, .T. ) ;
#36646 = CARTESIAN_POINT ( 'NONE',  ( 135.0000000000015632, 17.00000000000000000, 60.00000000000000000 ) ) ;
#36647 = CARTESIAN_POINT ( 'NONE',  ( 34.32915281903212446, 1.750000000000009548, 1.843413822775065825 ) ) ;
#36648 = ORIENTED_EDGE ( 'NONE', *, *, #33741, .F. ) ;
#36649 = ORIENTED_EDGE ( 'NONE', *, *, #9563, .T. ) ;
#36650 = ADVANCED_FACE ( 'NONE', ( #20273 ), #779, .F. ) ;
#36651 = FACE_OUTER_BOUND ( 'NONE', #30638, .T. ) ;
#36652 = ORIENTED_EDGE ( 'NONE', *, *, #40589, .T. ) ;
#36653 = CARTESIAN_POINT ( 'NONE',  ( 0.6108107228405675881, -1.056024183042613140, 9.963925895596188909 ) ) ;
#36654 = CARTESIAN_POINT ( 'NONE',  ( 185.0000000000000000, -5.999999999999950262, 339.9999999999998295 ) ) ;
#36655 = CARTESIAN_POINT ( 'NONE',  ( -164.9999999999990905, 16.00000000000000000, -24.99999999999999289 ) ) ;
#36656 = ORIENTED_EDGE ( 'NONE', *, *, #12687, .F. ) ;
#36657 = DIRECTION ( 'NONE',  ( 1.000000000000000000, 0.000000000000000000, 0.000000000000000000 ) ) ;
#36658 =( NAMED_UNIT ( * ) PLANE_ANGLE_UNIT ( ) SI_UNIT ( $, .RADIAN. ) );
#36659 = ORIENTED_EDGE ( 'NONE', *, *, #22227, .T. ) ;
#36660 = VERTEX_POINT ( 'NONE', #12561 ) ;
#36661 = ORIENTED_EDGE ( 'NONE', *, *, #37764, .F. ) ;
#36662 = CARTESIAN_POINT ( 'NONE',  ( 0.000000000000000000, 28.48684210526315752, 0.000000000000000000 ) ) ;
#36663 = CARTESIAN_POINT ( 'NONE',  ( 193.3040265531851105, 1.750000000000010658, -79.18171244307201562 ) ) ;
#36664 = ORIENTED_EDGE ( 'NONE', *, *, #48073, .T. ) ;
#36665 = VECTOR ( 'NONE', #45726, 1000.000000000000000 ) ;
#36666 = LINE ( 'NONE', #1490, #14312 ) ;
#36667 = FACE_OUTER_BOUND ( 'NONE', #35150, .T. ) ;
#36668 = CARTESIAN_POINT ( 'NONE',  ( 194.9999999999999716, 164.9999999999999716, 500.0000000000000000 ) ) ;
#36669 = CARTESIAN_POINT ( 'NONE',  ( 357.1715728752537871, -183.0000000000000284, 357.9999999999998295 ) ) ;
#36670 = DIRECTION ( 'NONE',  ( -1.000000000000000000, -0.000000000000000000, -0.000000000000000000 ) ) ;
#36671 = DIRECTION ( 'NONE',  ( -1.000000000000000000, -0.000000000000000000, -0.000000000000000000 ) ) ;
#36672 = CARTESIAN_POINT ( 'NONE',  ( -1.011271242968677875, -0.7347315653656004697, -10.00000000000000000 ) ) ;
#36673 = DIRECTION ( 'NONE',  ( 0.000000000000000000, 0.4027858274925602000, 0.9152942571496522906 ) ) ;
#36674 = CARTESIAN_POINT ( 'NONE',  ( 181.0000000000000284, -174.9999999999999716, -113.0000000000001563 ) ) ;
#36675 = DIRECTION ( 'NONE',  ( -0.000000000000000000, -1.000000000000000000, -0.000000000000000000 ) ) ;
#36676 = EDGE_CURVE ( 'NONE', #38146, #45661, #6838, .T. ) ;
#36677 = DIRECTION ( 'NONE',  ( 1.000000000000000000, 0.000000000000000000, 0.000000000000000000 ) ) ;
#36678 = AXIS2_PLACEMENT_3D ( 'NONE', #21539, #45862, #18692 ) ;
#36679 = CARTESIAN_POINT ( 'NONE',  ( 114.3291528190321173, -1.749999999999996669, 161.8434138227750907 ) ) ;
#36680 = ORIENTED_EDGE ( 'NONE', *, *, #43353, .T. ) ;
#36681 = DIRECTION ( 'NONE',  ( -0.000000000000000000, -0.000000000000000000, 1.000000000000000000 ) ) ;
#36682 = DIRECTION ( 'NONE',  ( -0.000000000000000000, -1.000000000000000000, -0.000000000000000000 ) ) ;
#36683 = CARTESIAN_POINT ( 'NONE',  ( -1.055760676366898521, -37.52140099356444836, -2.490396854064190535 ) ) ;
#36684 = CARTESIAN_POINT ( 'NONE',  ( -4.945973446814903696, 2.143131898507912917E-16, 165.0000000000000000 ) ) ;
#36685 =( BOUNDED_CURVE ( )  B_SPLINE_CURVE ( 3, ( #21531, #34360, #29489, #6142 ),
 .UNSPECIFIED., .F., .F. ) 
 B_SPLINE_CURVE_WITH_KNOTS ( ( 4, 4 ),
 ( 1.570796326794896558, 3.141592653589793116 ),
 .UNSPECIFIED. ) 
 CURVE ( )  GEOMETRIC_REPRESENTATION_ITEM ( )  RATIONAL_B_SPLINE_CURVE ( ( 1.000000000000000000, 0.8047378541243649375, 0.8047378541243649375, 1.000000000000000000 ) ) 
 REPRESENTATION_ITEM ( '' )  );
#36686 = EDGE_LOOP ( 'NONE', ( #34796, #13789, #11459, #21275, #24933, #23713 ) ) ;
#36687 = DIRECTION ( 'NONE',  ( -1.000000000000000000, 0.000000000000000000, 0.000000000000000000 ) ) ;
#36688 = EDGE_CURVE ( 'NONE', #35301, #44339, #28230, .T. ) ;
#36689 = EDGE_CURVE ( 'NONE', #6739, #28163, #8225, .T. ) ;
#36690 = PLANE ( 'NONE',  #18817 ) ;
#36691 = ORIENTED_EDGE ( 'NONE', *, *, #6538, .T. ) ;
#36692 = CARTESIAN_POINT ( 'NONE',  ( -0.3370904143228963812, 0.2449105217885287067, -10.00000000000000000 ) ) ;
#36693 = FACE_OUTER_BOUND ( 'NONE', #46033, .T. ) ;
#36694 = CARTESIAN_POINT ( 'NONE',  ( 113.3040265531850537, 1.749999999999997335, -119.1817124430720440 ) ) ;
#36695 =( BOUNDED_CURVE ( )  B_SPLINE_CURVE ( 3, ( #21649, #5996, #37338, #2164 ),
 .UNSPECIFIED., .F., .F. ) 
 B_SPLINE_CURVE_WITH_KNOTS ( ( 4, 4 ),
 ( 1.570796326794896558, 3.141592653589793116 ),
 .UNSPECIFIED. ) 
 CURVE ( )  GEOMETRIC_REPRESENTATION_ITEM ( )  RATIONAL_B_SPLINE_CURVE ( ( 1.000000000000000000, 0.8047378541243649375, 0.8047378541243649375, 1.000000000000000000 ) ) 
 REPRESENTATION_ITEM ( '' )  );
#36696 = ORIENTED_EDGE ( 'NONE', *, *, #25889, .T. ) ;
#36697 = CARTESIAN_POINT ( 'NONE',  ( -206.6959734468149463, -1.750000000000010658, 120.8182875569279702 ) ) ;
#36698 = B_SPLINE_SURFACE_WITH_KNOTS ( 'NONE', 3, 3, ( 
 ( #3715, #14754, #18590, #50103 ),
 ( #50619, #18838, #34522, #26561 ),
 ( #6803, #15012, #46018, #22952 ),
 ( #19366, #10649, #3189, #49843 ) ),
 .UNSPECIFIED., .F., .F., .F.,
 ( 4, 4 ),
 ( 4, 4 ),
 ( 0.000000000000000000, 1.000000000000000000 ),
 ( 0.000000000000000000, 1.000000000000000000 ),
 .UNSPECIFIED. ) ;
#36699 = ORIENTED_EDGE ( 'NONE', *, *, #9578, .F. ) ;
#36700 = ORIENTED_EDGE ( 'NONE', *, *, #18436, .F. ) ;
#36701 = EDGE_CURVE ( 'NONE', #44615, #48417, #27214, .T. ) ;
#36702 = EDGE_CURVE ( 'NONE', #21514, #44231, #25898, .T. ) ;
#36703 = ORIENTED_EDGE ( 'NONE', *, *, #24340, .F. ) ;
#36704 = CARTESIAN_POINT ( 'NONE',  ( 349.9999999999999432, -184.9999999999999716, 343.9999999999997726 ) ) ;
#36705 = CARTESIAN_POINT ( 'NONE',  ( 210.0000000000000568, 0.000000000000000000, -39.18171244307202983 ) ) ;
#36706 = ORIENTED_EDGE ( 'NONE', *, *, #27182, .F. ) ;
#36707 = DIRECTION ( 'NONE',  ( 0.000000000000000000, -1.000000000000000000, 0.000000000000000000 ) ) ;
#36708 = DIRECTION ( 'NONE',  ( -0.000000000000000000, -0.000000000000000000, -1.000000000000000000 ) ) ;
#36709 = EDGE_CURVE ( 'NONE', #43962, #25778, #25576, .T. ) ;
#36710 = CARTESIAN_POINT ( 'NONE',  ( 185.0000000000000284, 2.775557561562891351E-14, -99.00000000000014211 ) ) ;
#36711 =( BOUNDED_CURVE ( )  B_SPLINE_CURVE ( 3, ( #6328, #2715, #17364, #6066 ),
 .UNSPECIFIED., .F., .F. ) 
 B_SPLINE_CURVE_WITH_KNOTS ( ( 4, 4 ),
 ( 4.712388980384689674, 6.283185307179586232 ),
 .UNSPECIFIED. ) 
 CURVE ( )  GEOMETRIC_REPRESENTATION_ITEM ( )  RATIONAL_B_SPLINE_CURVE ( ( 1.000000000000000000, 0.8047378541243649375, 0.8047378541243649375, 1.000000000000000000 ) ) 
 REPRESENTATION_ITEM ( '' )  );
#36712 = CARTESIAN_POINT ( 'NONE',  ( 0.6909887759939999929, -1.008432015058921438, 9.987567862361069970 ) ) ;
#36713 = ORIENTED_EDGE ( 'NONE', *, *, #48795, .T. ) ;
#36714 = DIRECTION ( 'NONE',  ( -1.000000000000000000, -0.000000000000000000, -0.000000000000000000 ) ) ;
#36715 = EDGE_LOOP ( 'NONE', ( #28854, #9014, #43855, #2844, #4496, #14136 ) ) ;
#36716 = AXIS2_PLACEMENT_3D ( 'NONE', #17575, #45744, #49081 ) ;
#36717 = FACE_OUTER_BOUND ( 'NONE', #43188, .T. ) ;
#36718 = DIRECTION ( 'NONE',  ( 0.000000000000000000, 0.9749645535258959494, 0.2223603367690620558 ) ) ;
#36719 = ORIENTED_EDGE ( 'NONE', *, *, #17194, .T. ) ;
#36720 = ORIENTED_EDGE ( 'NONE', *, *, #2424, .T. ) ;
#36721 = ORIENTED_EDGE ( 'NONE', *, *, #7190, .T. ) ;
#36722 = CARTESIAN_POINT ( 'NONE',  ( 168.9999999999999716, 165.0000000000000000, -344.0000000000001137 ) ) ;
#36723 = CARTESIAN_POINT ( 'NONE',  ( 355.9999999999999432, 183.0000000000002558, -358.0000000000003411 ) ) ;
#36724 = EDGE_LOOP ( 'NONE', ( #41969, #11485, #28822, #25121 ) ) ;
#36725 = CARTESIAN_POINT ( 'NONE',  ( -34.95136153415531766, 36.40974830873496870, 8.356839323120299312 ) ) ;
#36726 = LINE ( 'NONE', #25652, #48318 ) ;
#36727 = DIRECTION ( 'NONE',  ( 1.000000000000000000, -0.000000000000000000, 0.000000000000000000 ) ) ;
#36728 = ORIENTED_EDGE ( 'NONE', *, *, #39395, .F. ) ;
#36729 = DIRECTION ( 'NONE',  ( -1.000000000000000000, 0.000000000000000000, -0.000000000000000000 ) ) ;
#36730 = CARTESIAN_POINT ( 'NONE',  ( 1.040834085586084257E-14, -6.912230148066169200, -5.000000000000000000 ) ) ;
#36731 = EDGE_CURVE ( 'NONE', #40834, #18563, #20670, .T. ) ;
#36732 = VECTOR ( 'NONE', #27040, 1000.000000000000000 ) ;
#36733 = DIRECTION ( 'NONE',  ( 0.000000000000000000, 0.000000000000000000, -1.000000000000000000 ) ) ;
#36734 = ORIENTED_EDGE ( 'NONE', *, *, #48490, .T. ) ;
#36735 = ADVANCED_FACE ( 'NONE', ( #7721, #38773 ), #27719, .T. ) ;
#36736 = VERTEX_POINT ( 'NONE', #34936 ) ;
#36737 = CONTEXT_DEPENDENT_SHAPE_REPRESENTATION ( #21397, #50282 ) ;
#36738 = DIRECTION ( 'NONE',  ( 0.000000000000000000, 0.000000000000000000, 1.000000000000000000 ) ) ;
#36739 = DIRECTION ( 'NONE',  ( -1.000000000000000000, 0.000000000000000000, -7.793956916774525800E-48 ) ) ;
#36740 = CARTESIAN_POINT ( 'NONE',  ( 0.1287570809895630941, -0.3962735484563133515, 10.00000000000000000 ) ) ;
#36741 = CARTESIAN_POINT ( 'NONE',  ( 210.0000000000000568, 0.000000000000000000, -79.18171244307201562 ) ) ;
#36742 = ORIENTED_EDGE ( 'NONE', *, *, #37858, .F. ) ;
#36743 = CYLINDRICAL_SURFACE ( 'NONE', #37646, 1.749999999999987566 ) ;
#36744 = CARTESIAN_POINT ( 'NONE',  ( 185.0000000000000000, -174.9999999999999716, -356.0000000000001705 ) ) ;
#36745 = DIRECTION ( 'NONE',  ( 0.000000000000000000, 0.000000000000000000, -1.000000000000000000 ) ) ;
#36746 = ORIENTED_EDGE ( 'NONE', *, *, #13930, .F. ) ;
#36747 = CARTESIAN_POINT ( 'NONE',  ( -27.33593271309441519, 41.94268121623345280, -9.367992836599951190 ) ) ;
#36749 = VERTEX_POINT ( 'NONE', #23611 ) ;
#36748 = VECTOR ( 'NONE', #15056, 1000.000000000000000 ) ;
#36750 = CARTESIAN_POINT ( 'NONE',  ( 35.51846793572394034, -35.99772139009119343, 7.906207997025717304 ) ) ;
#36751 = ORIENTED_EDGE ( 'NONE', *, *, #41535, .F. ) ;
#36752 = CARTESIAN_POINT ( 'NONE',  ( 210.0000000000000568, 0.000000000000000000, 42.56828755692799149 ) ) ;
#36753 = CARTESIAN_POINT ( 'NONE',  ( -8.470991794550055687, -5.371644396275288003, 9.390253821402620105 ) ) ;
#36754 = CARTESIAN_POINT ( 'NONE',  ( -204.9459734468149463, 2.143131898507890731E-16, -165.0000000000000000 ) ) ;
#36755 = ORIENTED_EDGE ( 'NONE', *, *, #28503, .F. ) ;
#36756 = ORIENTED_EDGE ( 'NONE', *, *, #23394, .F. ) ;
#36757 = CARTESIAN_POINT ( 'NONE',  ( 153.3040265531850537, -1.750000000000009992, -159.1817124430720298 ) ) ;
#36758 = CARTESIAN_POINT ( 'NONE',  ( 0.7601424845489945792, -1.297311920616997627, 9.927319414211225990 ) ) ;
#36759 = CARTESIAN_POINT ( 'NONE',  ( 34.08355720199905647, -2.371364769369109116, 7.455576670931136185 ) ) ;
#36760 = CARTESIAN_POINT ( 'NONE',  ( -46.69597344681494633, -1.750000000000010214, -39.18171244307202983 ) ) ;
#36761 = EDGE_CURVE ( 'NONE', #32625, #1717, #15412, .T. ) ;
#36762 = DIRECTION ( 'NONE',  ( -1.000000000000000000, 0.000000000000000000, -0.000000000000000000 ) ) ;
#36763 = EDGE_LOOP ( 'NONE', ( #18146, #39503, #14204, #21770 ) ) ;
#36764 = VERTEX_POINT ( 'NONE', #16417 ) ;
#36765 = CARTESIAN_POINT ( 'NONE',  ( 2.500000000000002665, 204.9999999999999716, -234.7500000000000000 ) ) ;
#36766 = ORIENTED_EDGE ( 'NONE', *, *, #3769, .F. ) ;
#36767 = PLANE ( 'NONE',  #11161 ) ;
#36768 = CARTESIAN_POINT ( 'NONE',  ( 357.1715728752537302, -183.0000000000001705, -358.0000000000003411 ) ) ;
#36769 = ORIENTED_EDGE ( 'NONE', *, *, #48091, .F. ) ;
#36770 = DIRECTION ( 'NONE',  ( 1.000000000000000000, 0.000000000000000000, -1.586032892321652482E-16 ) ) ;
#36771 = DIRECTION ( 'NONE',  ( -1.000000000000000000, 0.000000000000000000, 0.000000000000000000 ) ) ;
#36772 = ORIENTED_EDGE ( 'NONE', *, *, #23465, .F. ) ;
#36773 = CARTESIAN_POINT ( 'NONE',  ( 1.249999999999999778, 0.000000000000000000, 10.00000000000000000 ) ) ;
#36774 = DIRECTION ( 'NONE',  ( 0.000000000000000000, 1.000000000000000000, -5.664403186863042467E-17 ) ) ;
#36775 = DIRECTION ( 'NONE',  ( -1.000000000000000000, 0.000000000000000000, 0.000000000000000000 ) ) ;
#36776 = FACE_OUTER_BOUND ( 'NONE', #40968, .T. ) ;
#36777 = VERTEX_POINT ( 'NONE', #35695 ) ;
#36778 = VECTOR ( 'NONE', #123, 1000.000000000000000 ) ;
#36779 = ORIENTED_EDGE ( 'NONE', *, *, #37829, .T. ) ;
#36780 = EDGE_LOOP ( 'NONE', ( #32229, #42126, #34270, #11916, #42398, #42930 ) ) ;
#36781 = FACE_OUTER_BOUND ( 'NONE', #31228, .T. ) ;
#36782 = CARTESIAN_POINT ( 'NONE',  ( 32.36066692128250821, -7.813306791042813337, 3.199614146704519602 ) ) ;
#36783 = CARTESIAN_POINT ( 'NONE',  ( -6.208157169185024138, 36.98937201184289592, 8.506357886886741326 ) ) ;
#36784 = CARTESIAN_POINT ( 'NONE',  ( 9.483938762529211530, -3.217310375392752331, 3.215106848023439934 ) ) ;
#36785 = CLOSED_SHELL ( 'NONE', ( #47836, #5441, #30635, #10468, #17076, #17274, #20829, #18662, #32569, #1784, #28776, #19677, #21735, #22683, #10445, #47285, #8591, #28343, #30872, #48749, #33556 ) ) ;
#36786 = EDGE_LOOP ( 'NONE', ( #6520, #33298, #29105, #39658 ) ) ;
#36787 = CARTESIAN_POINT ( 'NONE',  ( 169.0000000000000000, -272.5000000000000000, -94.99999999999988631 ) ) ;
#36788 = ORIENTED_EDGE ( 'NONE', *, *, #17913, .T. ) ;
#36789 = SHAPE_REPRESENTATION_RELATIONSHIP ( 'NONE' , 'NONE' ,  #50327, #37482 ) ;
#36790 = CARTESIAN_POINT ( 'NONE',  ( -64.99999999999783995, 17.00000000000000000, 115.0000000000000142 ) ) ;
#36791 = DIRECTION ( 'NONE',  ( -0.000000000000000000, -6.123233995736766036E-17, 1.000000000000000000 ) ) ;
#36792 = CARTESIAN_POINT ( 'NONE',  ( -165.3973046169136012, -62.56198943095993315, -94.69675437945474528 ) ) ;
#36793 = CARTESIAN_POINT ( 'NONE',  ( 152.2789002873379900, 1.750000000000009548, -160.2068387089191219 ) ) ;
#36794 = DIRECTION ( 'NONE',  ( 0.000000000000000000, 0.000000000000000000, 1.000000000000000000 ) ) ;
#36795 = LINE ( 'NONE', #36546, #32182 ) ;
#36796 = ORIENTED_EDGE ( 'NONE', *, *, #15794, .F. ) ;
#36797 = CARTESIAN_POINT ( 'NONE',  ( -10.00000000000000178, -37.59858392880988731, -7.836098764781820769 ) ) ;
#36798 = B_SPLINE_SURFACE_WITH_KNOTS ( 'NONE', 3, 3, ( 
 ( #33509, #25804, #71, #39081 ),
 ( #19541, #41448, #7772, #22450 ),
 ( #30153, #6552, #41703, #22206 ),
 ( #10405, #3901, #38122, #35225 ) ),
 .UNSPECIFIED., .F., .F., .F.,
 ( 4, 4 ),
 ( 4, 4 ),
 ( 0.000000000000000000, 1.000000000000000000 ),
 ( 0.000000000000000000, 1.000000000000000000 ),
 .UNSPECIFIED. ) ;
#36799 = CARTESIAN_POINT ( 'NONE',  ( 0.000000000000000000, 185.0000000000000284, -356.0000000000002274 ) ) ;
#36800 = CARTESIAN_POINT ( 'NONE',  ( -119.9999999999994174, 17.00000000000000000, -54.99999999999999289 ) ) ;
#36801 = CARTESIAN_POINT ( 'NONE',  ( 80.00000000000153477, 17.00000000000000000, 60.00000000000000000 ) ) ;
#36802 = EDGE_LOOP ( 'NONE', ( #24078, #22409, #40879, #5563, #13257, #15800 ) ) ;
#36803 = CYLINDRICAL_SURFACE ( 'NONE', #27001, 2.000000000000001776 ) ;
#36804 = VERTEX_POINT ( 'NONE', #31068 ) ;
#36805 = CARTESIAN_POINT ( 'NONE',  ( -4.945973446814916130, 1.025126265847097651, -77.43171244307197298 ) ) ;
#36806 = DIRECTION ( 'NONE',  ( 0.000000000000000000, 0.2223603367690619725, -0.9749645535258958384 ) ) ;
#36807 = CARTESIAN_POINT ( 'NONE',  ( 1.228394325311184421, -1.341866297401743235, 9.903764339332088440 ) ) ;
#36808 = VECTOR ( 'NONE', #50344, 1000.000000000000000 ) ;
#36809 = ORIENTED_EDGE ( 'NONE', *, *, #41208, .F. ) ;
#36810 = VECTOR ( 'NONE', #34449, 1000.000000000000000 ) ;
#36811 = EDGE_CURVE ( 'NONE', #18711, #3809, #46669, .T. ) ;
#36812 = CARTESIAN_POINT ( 'NONE',  ( 168.9999999999999716, 8.000000000000062172, -350.0000000000001705 ) ) ;
#36813 = CARTESIAN_POINT ( 'NONE',  ( 0.3862712429686810944, 1.188820645368943607, 10.00000000000000000 ) ) ;
#36815 = VECTOR ( 'NONE', #9495, 1000.000000000000000 ) ;
#36814 = DIRECTION ( 'NONE',  ( 0.000000000000000000, -2.537652627714643577E-15, -1.000000000000000000 ) ) ;
#36816 = AXIS2_PLACEMENT_3D ( 'NONE', #6637, #38469, #45847 ) ;
#36817 = DIRECTION ( 'NONE',  ( -0.000000000000000000, 1.000000000000000000, -1.604368532695312981E-16 ) ) ;
#36818 = ADVANCED_FACE ( 'NONE', ( #4372 ), #39030, .F. ) ;
#36819 = ORIENTED_EDGE ( 'NONE', *, *, #13028, .F. ) ;
#36820 = AXIS2_PLACEMENT_3D ( 'NONE', #12577, #32094, #16442 ) ;
#36821 = VERTEX_POINT ( 'NONE', #4117 ) ;
#36822 = DIRECTION ( 'NONE',  ( 1.110223024625156171E-16, -0.7071067811865475727, -0.7071067811865475727 ) ) ;
#36823 = ADVANCED_FACE ( 'NONE', ( #25 ), #15660, .F. ) ;
#36824 = CARTESIAN_POINT ( 'NONE',  ( -0.3862712429686977478, 1.188820645368937390, 10.00000000000000000 ) ) ;
#36825 = EDGE_CURVE ( 'NONE', #9839, #15483, #16939, .T. ) ;
#36826 = VECTOR ( 'NONE', #42522, 1000.000000000000000 ) ;
#36827 = ORIENTED_EDGE ( 'NONE', *, *, #3553, .F. ) ;
#36828 = ORIENTED_EDGE ( 'NONE', *, *, #12063, .T. ) ;
#36829 = DIRECTION ( 'NONE',  ( 1.000000000000000000, 0.000000000000000000, -4.625929269271584521E-16 ) ) ;
#36830 = DIRECTION ( 'NONE',  ( -3.172065784643302499E-16, -1.000000000000000000, 2.537652627714642000E-15 ) ) ;
#36831 = CARTESIAN_POINT ( 'NONE',  ( -48.44597344681495343, 0.000000000000000000, -120.9317124430720725 ) ) ;
#36832 = CARTESIAN_POINT ( 'NONE',  ( -1.637465050678293954, -0.1702693745679247084, 9.936700280135957186 ) ) ;
#36833 = ORIENTED_EDGE ( 'NONE', *, *, #17539, .F. ) ;
#36834 = ORIENTED_EDGE ( 'NONE', *, *, #40232, .F. ) ;
#36835 = ORIENTED_EDGE ( 'NONE', *, *, #45604, .T. ) ;
#36836 = ADVANCED_FACE ( 'NONE', ( #4858 ), #40530, .F. ) ;
#36837 = FACE_OUTER_BOUND ( 'NONE', #17652, .T. ) ;
#36838 = EDGE_CURVE ( 'NONE', #6015, #35970, #2032, .T. ) ;
#36839 = DIRECTION ( 'NONE',  ( -1.000000000000000000, -0.000000000000000000, -0.000000000000000000 ) ) ;
#36840 = ORIENTED_EDGE ( 'NONE', *, *, #13619, .T. ) ;
#36841 = VERTEX_POINT ( 'NONE', #28732 ) ;
#36842 = B_SPLINE_CURVE_WITH_KNOTS ( 'NONE', 3,
 ( #29398, #49358, #14244, #26060 ),
 .UNSPECIFIED., .F., .F.,
 ( 4, 4 ),
 ( 1.734723475976807094E-18, 0.002458791966311101550 ),
 .UNSPECIFIED. ) ;
#36843 = CARTESIAN_POINT ( 'NONE',  ( 33.30402655318503946, -1.750000000000009992, 0.8182875569279768335 ) ) ;
#36844 =( BOUNDED_CURVE ( )  B_SPLINE_CURVE ( 3, ( #10887, #33999, #14738, #14484 ),
 .UNSPECIFIED., .F., .F. ) 
 B_SPLINE_CURVE_WITH_KNOTS ( ( 4, 4 ),
 ( 3.141592653589793116, 4.712388980384689674 ),
 .UNSPECIFIED. ) 
 CURVE ( )  GEOMETRIC_REPRESENTATION_ITEM ( )  RATIONAL_B_SPLINE_CURVE ( ( 1.000000000000000000, 0.8047378541243649375, 0.8047378541243649375, 1.000000000000000000 ) ) 
 REPRESENTATION_ITEM ( '' )  );
#36845 = CARTESIAN_POINT ( 'NONE',  ( -206.6959734468149463, -1.750000000000009992, 0.8182875569279768335 ) ) ;
#36846 = ORIENTED_EDGE ( 'NONE', *, *, #48830, .F. ) ;
#36847 = EDGE_CURVE ( 'NONE', #38131, #30152, #13064, .T. ) ;
#36848 = ADVANCED_FACE ( 'NONE', ( #13810 ), #13569, .F. ) ;
#36849 = VERTEX_POINT ( 'NONE', #1029 ) ;
#36850 = CARTESIAN_POINT ( 'NONE',  ( 49.67735855322978011, -8.912210285361751971, 8.356839323120299312 ) ) ;
#36851 = CARTESIAN_POINT ( 'NONE',  ( 0.3862712429686810944, 1.188820645368943607, -10.00000000000000000 ) ) ;
#36853 = VERTEX_POINT ( 'NONE', #29234 ) ;
#36852 = VECTOR ( 'NONE', #23907, 1000.000000000000000 ) ;
#36854 = DIRECTION ( 'NONE',  ( 0.000000000000000000, 0.000000000000000000, -1.000000000000000000 ) ) ;
#36855 = EDGE_CURVE ( 'NONE', #23492, #50585, #36190, .T. ) ;
#36856 = CYLINDRICAL_SURFACE ( 'NONE', #18551, 1.750000000000001554 ) ;
#36857 = DIRECTION ( 'NONE',  ( 0.000000000000000000, 0.000000000000000000, -1.000000000000000000 ) ) ;
#36858 = FACE_OUTER_BOUND ( 'NONE', #7242, .T. ) ;
#36859 = EDGE_CURVE ( 'NONE', #15591, #21384, #21522, .T. ) ;
#36860 = AXIS2_PLACEMENT_3D ( 'NONE', #3707, #31174, #11665 ) ;
#36861 = CARTESIAN_POINT ( 'NONE',  ( -208.4459734468148611, 1.025126265847089435, -40.93171244307204404 ) ) ;
#36862 = ORIENTED_EDGE ( 'NONE', *, *, #3616, .F. ) ;
#36863 = CIRCLE ( 'NONE', #25359, 1.880036658038868991 ) ;
#36864 = EDGE_CURVE ( 'NONE', #47416, #2022, #22307, .T. ) ;
#36866 = AXIS2_PLACEMENT_3D ( 'NONE', #31302, #31557, #31042 ) ;
#36865 = DIRECTION ( 'NONE',  ( 0.000000000000000000, 0.000000000000000000, 1.000000000000000000 ) ) ;
#36867 = ADVANCED_FACE ( 'NONE', ( #32336 ), #36447, .F. ) ;
#36868 = FACE_OUTER_BOUND ( 'NONE', #31556, .T. ) ;
#36869 = CARTESIAN_POINT ( 'NONE',  ( 194.9999999999999432, -173.0000000000000000, 352.0000000000000568 ) ) ;
#36870 = LINE ( 'NONE', #33004, #6098 ) ;
#36871 = VECTOR ( 'NONE', #31437, 1000.000000000000000 ) ;
#36872 = CARTESIAN_POINT ( 'NONE',  ( 344.0000000000000000, -174.9999999999999432, 341.9999999999998295 ) ) ;
#36873 = CARTESIAN_POINT ( 'NONE',  ( 6.875132362119187768, -50.00000000000000711, 8.356839323120299312 ) ) ;
#36874 = CARTESIAN_POINT ( 'NONE',  ( 175.0000000000000000, 0.000000000000000000, 122.5000000000000142 ) ) ;
#36875 = EDGE_CURVE ( 'NONE', #7547, #16814, #1783, .T. ) ;
#36876 = CARTESIAN_POINT ( 'NONE',  ( 22.69295089195473025, 45.31600496604705341, 7.455576670931136185 ) ) ;
#36877 = ORIENTED_EDGE ( 'NONE', *, *, #5123, .F. ) ;
#36878 = LINE ( 'NONE', #9894, #25650 ) ;
#36879 = ADVANCED_FACE ( 'NONE', ( #5619 ), #32591, .F. ) ;
#36880 = EDGE_CURVE ( 'NONE', #3051, #21391, #48924, .T. ) ;
#36881 = DIRECTION ( 'NONE',  ( 0.000000000000000000, 0.000000000000000000, 1.000000000000000000 ) ) ;
#36882 = CARTESIAN_POINT ( 'NONE',  ( 113.3040265531850537, 0.000000000000000000, 165.0000000000000000 ) ) ;
#36883 = CARTESIAN_POINT ( 'NONE',  ( -127.7210997126620242, 1.749999999999996891, -40.20683870891911482 ) ) ;
#36884 = DIRECTION ( 'NONE',  ( -1.000000000000000000, -0.000000000000000000, -0.000000000000000000 ) ) ;
#36885 = ORIENTED_EDGE ( 'NONE', *, *, #35989, .F. ) ;
#36886 = CYLINDRICAL_SURFACE ( 'NONE', #6038, 4.000000000000003553 ) ;
#36887 = ORIENTED_EDGE ( 'NONE', *, *, #36620, .F. ) ;
#36888 = VECTOR ( 'NONE', #1020, 1000.000000000000000 ) ;
#36889 = LINE ( 'NONE', #6054, #28359 ) ;
#36890 = ADVANCED_FACE ( 'NONE', ( #48676 ), #44352, .T. ) ;
#36891 = CARTESIAN_POINT ( 'NONE',  ( 31.55402655318503236, 0.000000000000000000, -120.9317124430720725 ) ) ;
#36892 = VECTOR ( 'NONE', #4606, 1000.000000000000000 ) ;
#36893 = B_SPLINE_CURVE_WITH_KNOTS ( 'NONE', 3,
 ( #1259, #48146, #36157, #32813 ),
 .UNSPECIFIED., .F., .F.,
 ( 4, 4 ),
 ( 0.0001426870652665898870, 0.006281196370944869614 ),
 .UNSPECIFIED. ) ;
#36894 = ORIENTED_EDGE ( 'NONE', *, *, #12915, .T. ) ;
#36895 = CARTESIAN_POINT ( 'NONE',  ( -166.6959734468149463, 1.750000000000009992, -159.1817124430720298 ) ) ;
#36896 = PLANE ( 'NONE',  #5272 ) ;
#36897 = EDGE_LOOP ( 'NONE', ( #3674, #31595, #651, #32749 ) ) ;
#36898 = ORIENTED_EDGE ( 'NONE', *, *, #49926, .F. ) ;
#36899 = VECTOR ( 'NONE', #15665, 1000.000000000000114 ) ;
#36900 = EDGE_CURVE ( 'NONE', #27168, #31470, #47686, .T. ) ;
#36901 = DIRECTION ( 'NONE',  ( 1.000000000000000000, 0.000000000000000000, 0.000000000000000000 ) ) ;
#36902 = CYLINDRICAL_SURFACE ( 'NONE', #29145, 1.750000000000015543 ) ;
#36903 = CYLINDRICAL_SURFACE ( 'NONE', #5404, 1.750000000000015543 ) ;
#36904 = AXIS2_PLACEMENT_3D ( 'NONE', #4852, #16660, #20265 ) ;
#36905 = ORIENTED_EDGE ( 'NONE', *, *, #21401, .F. ) ;
#36906 = DIRECTION ( 'NONE',  ( 0.000000000000000000, -1.000000000000000000, 0.000000000000000000 ) ) ;
#36907 = DIRECTION ( 'NONE',  ( -1.000000000000000000, 0.000000000000000000, 0.000000000000000000 ) ) ;
#36908 = EDGE_LOOP ( 'NONE', ( #33171, #25375, #39866, #48304, #37744, #27236 ) ) ;
#36909 = ADVANCED_FACE ( 'NONE', ( #48429 ), #9472, .T. ) ;
#36910 = VERTEX_POINT ( 'NONE', #33345 ) ;
#36911 = ORIENTED_EDGE ( 'NONE', *, *, #32781, .T. ) ;
#36912 = CARTESIAN_POINT ( 'NONE',  ( 1.011271242968694084, -0.7347315653655782652, 10.00000000000000000 ) ) ;
#36913 = CARTESIAN_POINT ( 'NONE',  ( 185.0000000000000000, -164.9999999999999432, 343.9999999999998863 ) ) ;
#36914 = ORIENTED_EDGE ( 'NONE', *, *, #39314, .F. ) ;
#36915 = CARTESIAN_POINT ( 'NONE',  ( -44.94597344681493922, -1.025126265847089435, 122.5682875569280128 ) ) ;
#36916 = CARTESIAN_POINT ( 'NONE',  ( -206.6959734468149463, 0.000000000000000000, -165.0000000000000000 ) ) ;
#36917 = ADVANCED_FACE ( 'NONE', ( #40038 ), #47930, .T. ) ;
#36918 = CARTESIAN_POINT ( 'NONE',  ( 9.185112145816566098, 0.000000000000000000, 0.000000000000000000 ) ) ;
#36919 = DIRECTION ( 'NONE',  ( 1.000000000000000000, 1.156482317317870492E-16, -0.000000000000000000 ) ) ;
#36920 = EDGE_CURVE ( 'NONE', #28510, #16010, #21540, .T. ) ;
#36921 = CARTESIAN_POINT ( 'NONE',  ( 4.999999999999999112, 175.0000000000000284, 350.0000000000002274 ) ) ;
#36922 = DIRECTION ( 'NONE',  ( 0.000000000000000000, -0.000000000000000000, -1.000000000000000000 ) ) ;
#36923 = DIRECTION ( 'NONE',  ( 0.000000000000000000, 0.000000000000000000, 1.000000000000000000 ) ) ;
#36924 = EDGE_CURVE ( 'NONE', #2086, #14979, #46092, .T. ) ;
#36925 = DIRECTION ( 'NONE',  ( -1.000000000000000000, -0.000000000000000000, -0.000000000000000000 ) ) ;
#36926 = CARTESIAN_POINT ( 'NONE',  ( 16.15814872688565984, 4.048305257546810587, -2.870787844569587133 ) ) ;
#36927 = AXIS2_PLACEMENT_3D ( 'NONE', #23552, #461, #11747 ) ;
#36928 = EDGE_CURVE ( 'NONE', #40248, #27664, #41776, .T. ) ;
#36929 = EDGE_CURVE ( 'NONE', #22371, #22111, #41532, .T. ) ;
#36930 = CARTESIAN_POINT ( 'NONE',  ( -1.011271242968683426, -0.7347315653655928092, 3.333333333333333481 ) ) ;
#36931 = VECTOR ( 'NONE', #30043, 1000.000000000000000 ) ;
#36932 = LINE ( 'NONE', #9439, #23248 ) ;
#36933 = EDGE_LOOP ( 'NONE', ( #2579, #30467, #4568, #41323 ) ) ;
#36934 = VECTOR ( 'NONE', #39483, 1000.000000000000000 ) ;
#36935 = CARTESIAN_POINT ( 'NONE',  ( -206.6959734468149463, -1.750000000000010658, 80.81828755692798438 ) ) ;
#36936 = AXIS2_PLACEMENT_3D ( 'NONE', #3292, #22799, #7670 ) ;
#36937 = DIRECTION ( 'NONE',  ( -1.000000000000000000, 0.000000000000000000, 0.000000000000000000 ) ) ;
#36938 = CARTESIAN_POINT ( 'NONE',  ( -4.339432828817248122, -37.24807810779213213, -8.192531242611266862 ) ) ;
#36939 = CARTESIAN_POINT ( 'NONE',  ( 356.0000000000000000, -165.0000000000001137, -340.0000000000002842 ) ) ;
#36940 = ORIENTED_EDGE ( 'NONE', *, *, #8693, .T. ) ;
#36941 = CARTESIAN_POINT ( 'NONE',  ( 85.00000000000123634, 17.00000000000000000, 5.000000000000004441 ) ) ;
#36942 = ADVANCED_FACE ( 'NONE', ( #30236 ), #34104, .T. ) ;
#36943 = CARTESIAN_POINT ( 'NONE',  ( 181.0000000000000000, -272.4999999999999432, -343.9999999999999432 ) ) ;
#36944 = EDGE_LOOP ( 'NONE', ( #37882, #12117, #22185, #41888 ) ) ;
#36945 = CARTESIAN_POINT ( 'NONE',  ( -11.54386348672375107, -12.18274641659808211, -9.233365092205394475 ) ) ;
#36946 = DIRECTION ( 'NONE',  ( -0.000000000000000000, -0.000000000000000000, -1.000000000000000000 ) ) ;
#36947 = LINE ( 'NONE', #29715, #46267 ) ;
#36948 = VERTEX_POINT ( 'NONE', #30488 ) ;
#36949 = CARTESIAN_POINT ( 'NONE',  ( 151.5540265531850537, 0.000000000000000000, 122.5682875569279702 ) ) ;
#36950 = ORIENTED_EDGE ( 'NONE', *, *, #14848, .F. ) ;
#36951 = VERTEX_POINT ( 'NONE', #41273 ) ;
#36952 = DIRECTION ( 'NONE',  ( 1.000000000000000000, 0.000000000000000000, 0.000000000000000000 ) ) ;
#36953 = EDGE_LOOP ( 'NONE', ( #43299, #29878, #10219, #16598 ) ) ;
#36954 = CARTESIAN_POINT ( 'NONE',  ( -14.49999999999999822, 12.98684210526315930, 19.37312575500900280 ) ) ;
#36955 = CARTESIAN_POINT ( 'NONE',  ( -22.69295089195507487, -45.31600496604688999, 7.455576670931136185 ) ) ;
#36956 = ORIENTED_EDGE ( 'NONE', *, *, #2704, .F. ) ;
#36957 = CARTESIAN_POINT ( 'NONE',  ( -0.1287570809895658697, 0.3962735484563123523, 10.00000000000000000 ) ) ;
#36958 = CARTESIAN_POINT ( 'NONE',  ( -44.94597344681493922, 2.143131898507880377E-16, -120.9317124430720725 ) ) ;
#36959 = FACE_OUTER_BOUND ( 'NONE', #37986, .T. ) ;
#36960 = DIRECTION ( 'NONE',  ( -1.000000000000000000, 0.000000000000000000, 0.000000000000000000 ) ) ;
#36961 = VERTEX_POINT ( 'NONE', #10988 ) ;
#36962 = CARTESIAN_POINT ( 'NONE',  ( 350.0000000000000000, -168.9999999999999432, -360.0000000000002274 ) ) ;
#36963 = VECTOR ( 'NONE', #8154, 1000.000000000000227 ) ;
#36964 = VECTOR ( 'NONE', #24119, 1000.000000000000227 ) ;
#36965 = ORIENTED_EDGE ( 'NONE', *, *, #31688, .T. ) ;
#36966 = CARTESIAN_POINT ( 'NONE',  ( -64.99999999999940314, 17.00000000000000000, -30.00000000000000000 ) ) ;
#36967 = FACE_OUTER_BOUND ( 'NONE', #23769, .T. ) ;
#36968 = VERTEX_POINT ( 'NONE', #49928 ) ;
#36969 = VERTEX_POINT ( 'NONE', #25637 ) ;
#36970 = ORIENTED_EDGE ( 'NONE', *, *, #19577, .T. ) ;
#36971 = DIRECTION ( 'NONE',  ( 0.000000000000000000, 0.000000000000000000, 1.000000000000000000 ) ) ;
#36972 = CARTESIAN_POINT ( 'NONE',  ( 210.0000000000000568, 0.000000000000000000, -79.18171244307201562 ) ) ;
#36973 = AXIS2_PLACEMENT_3D ( 'NONE', #9193, #28948, #9447 ) ;
#36974 = VERTEX_POINT ( 'NONE', #6630 ) ;
#36975 = CYLINDRICAL_SURFACE ( 'NONE', #19178, 1.750000000000008438 ) ;
#36976 = CARTESIAN_POINT ( 'NONE',  ( 1.275994128725544741, -0.1230186051320594776, 9.948547179989619238 ) ) ;
#36977 = PLANE ( 'NONE',  #49288 ) ;
#36978 = EDGE_CURVE ( 'NONE', #48741, #8469, #22530, .T. ) ;
#36979 = EDGE_CURVE ( 'NONE', #1481, #11106, #26385, .T. ) ;
#36980 = ORIENTED_EDGE ( 'NONE', *, *, #45375, .F. ) ;
#36981 = DIRECTION ( 'NONE',  ( -1.000000000000000000, -0.000000000000000000, -0.000000000000000000 ) ) ;
#36982 = EDGE_CURVE ( 'NONE', #16242, #49685, #1885, .T. ) ;
#36983 = CARTESIAN_POINT ( 'NONE',  ( 0.3862712429686894766, -1.188820645368940276, 10.00000000000000000 ) ) ;
#36984 = EDGE_LOOP ( 'NONE', ( #25715, #50524, #31442, #28792 ) ) ;
#36985 = ORIENTED_EDGE ( 'NONE', *, *, #19540, .T. ) ;
#36986 = EDGE_CURVE ( 'NONE', #37443, #25256, #22341, .T. ) ;
#36987 = SHAPE_DEFINITION_REPRESENTATION ( #9731, #35275 ) ;
#36988 = ADVANCED_FACE ( 'NONE', ( #33593 ), #38215, .F. ) ;
#36989 = CARTESIAN_POINT ( 'NONE',  ( 210.0000000000000568, 0.000000000000000000, -157.4317124430720298 ) ) ;
#36990 =( BOUNDED_CURVE ( )  B_SPLINE_CURVE ( 3, ( #15583, #689, #4540, #11991 ),
 .UNSPECIFIED., .F., .F. ) 
 B_SPLINE_CURVE_WITH_KNOTS ( ( 4, 4 ),
 ( 4.712388980384689674, 6.283185307179586232 ),
 .UNSPECIFIED. ) 
 CURVE ( )  GEOMETRIC_REPRESENTATION_ITEM ( )  RATIONAL_B_SPLINE_CURVE ( ( 1.000000000000000000, 0.8047378541243649375, 0.8047378541243649375, 1.000000000000000000 ) ) 
 REPRESENTATION_ITEM ( '' )  );
#36991 = DIRECTION ( 'NONE',  ( 0.000000000000000000, -1.000000000000000000, 0.000000000000000000 ) ) ;
#36992 = CARTESIAN_POINT ( 'NONE',  ( -23.29043492822808759, 24.10797434788186067, 1.847720168420772691 ) ) ;
#36993 = CARTESIAN_POINT ( 'NONE',  ( -64.99999999999815259, 16.00000000000000000, 65.00000000000000000 ) ) ;
#36994 = ORIENTED_EDGE ( 'NONE', *, *, #40212, .T. ) ;
#36995 = DIRECTION ( 'NONE',  ( -0.000000000000000000, -0.000000000000000000, -1.000000000000000000 ) ) ;
#36996 = LINE ( 'NONE', #26170, #31200 ) ;
#36997 =( BOUNDED_CURVE ( )  B_SPLINE_CURVE ( 3, ( #13854, #22078, #45142, #41580 ),
 .UNSPECIFIED., .F., .F. ) 
 B_SPLINE_CURVE_WITH_KNOTS ( ( 4, 4 ),
 ( 0.000000000000000000, 1.570796326794896558 ),
 .UNSPECIFIED. ) 
 CURVE ( )  GEOMETRIC_REPRESENTATION_ITEM ( )  RATIONAL_B_SPLINE_CURVE ( ( 1.000000000000000000, 0.8047378541243649375, 0.8047378541243649375, 1.000000000000000000 ) ) 
 REPRESENTATION_ITEM ( '' )  );
#36998 = EDGE_CURVE ( 'NONE', #5426, #7866, #33850, .T. ) ;
#36999 = CARTESIAN_POINT ( 'NONE',  ( 154.1026953830863420, 70.03596893647589638, -94.69675437945477370 ) ) ;
#37000 = DIRECTION ( 'NONE',  ( -0.000000000000000000, -0.000000000000000000, -1.000000000000000000 ) ) ;
#37001 = CARTESIAN_POINT ( 'NONE',  ( 181.0000000000000000, 165.0000000000000000, -356.0000000000001705 ) ) ;
#37002 = CIRCLE ( 'NONE', #14835, 3.749999999999975575 ) ;
#37003 = ORIENTED_EDGE ( 'NONE', *, *, #23533, .F. ) ;
#37004 = CARTESIAN_POINT ( 'NONE',  ( 0.2773062244624638351, -1.251557370488896481, 9.948547179989619238 ) ) ;
#37005 = ORIENTED_EDGE ( 'NONE', *, *, #3586, .F. ) ;
#37006 = DIRECTION ( 'NONE',  ( 0.000000000000000000, 0.000000000000000000, -1.000000000000000000 ) ) ;
#37007 = ORIENTED_EDGE ( 'NONE', *, *, #41420, .F. ) ;
#37008 = CARTESIAN_POINT ( 'NONE',  ( 75.05402655318509630, 1.025126265847089435, -157.4317124430720582 ) ) ;
#37009 = VECTOR ( 'NONE', #1590, 1000.000000000000000 ) ;
#37010 = DIRECTION ( 'NONE',  ( 0.000000000000000000, 0.000000000000000000, 1.000000000000000000 ) ) ;
#37011 =( BOUNDED_CURVE ( )  B_SPLINE_CURVE ( 3, ( #48647, #24852, #29208, #39759 ),
 .UNSPECIFIED., .F., .F. ) 
 B_SPLINE_CURVE_WITH_KNOTS ( ( 4, 4 ),
 ( 1.570796326794896558, 3.141592653589793116 ),
 .UNSPECIFIED. ) 
 CURVE ( )  GEOMETRIC_REPRESENTATION_ITEM ( )  RATIONAL_B_SPLINE_CURVE ( ( 1.000000000000000000, 0.8047378541243649375, 0.8047378541243649375, 1.000000000000000000 ) ) 
 REPRESENTATION_ITEM ( '' )  );
#37012 = EDGE_LOOP ( 'NONE', ( #15314, #37656, #5914, #14825 ) ) ;
#37013 = CARTESIAN_POINT ( 'NONE',  ( 169.0000000000000000, -174.9999999999999716, -99.00000000000014211 ) ) ;
#37014 = ORIENTED_EDGE ( 'NONE', *, *, #22515, .T. ) ;
#37015 = CARTESIAN_POINT ( 'NONE',  ( 73.30402655318508209, 1.750000000000009992, -159.1817124430720298 ) ) ;
#37016 = DIRECTION ( 'NONE',  ( 0.2130880182788259525, 0.000000000000000000, -0.9770330068457272477 ) ) ;
#37017 = DIRECTION ( 'NONE',  ( -1.000000000000000000, -0.000000000000000000, -0.000000000000000000 ) ) ;
#37018 = CARTESIAN_POINT ( 'NONE',  ( 74.32915281903215998, -1.750000000000009326, 159.7931612910809065 ) ) ;
#37019 = DIRECTION ( 'NONE',  ( 0.000000000000000000, -2.537652627714643577E-15, -1.000000000000000000 ) ) ;
#37020 = ORIENTED_EDGE ( 'NONE', *, *, #38475, .F. ) ;
#37021 = ORIENTED_EDGE ( 'NONE', *, *, #16957, .T. ) ;
#37022 = CARTESIAN_POINT ( 'NONE',  ( 6.646097924774390542, -4.355953743237533260, 9.432811472610147518 ) ) ;
#37023 = ADVANCED_FACE ( 'NONE', ( #2528 ), #28569, .T. ) ;
#37024 = ORIENTED_EDGE ( 'NONE', *, *, #37397, .T. ) ;
#37025 = DIRECTION ( 'NONE',  ( 1.000000000000000000, 0.000000000000000000, 0.000000000000000000 ) ) ;
#37026 = CARTESIAN_POINT ( 'NONE',  ( 210.0000000000000568, 0.000000000000000000, -117.4317124430720298 ) ) ;
#37027 = ORIENTED_EDGE ( 'NONE', *, *, #17326, .F. ) ;
#37028 = LINE ( 'NONE', #12627, #16386 ) ;
#37029 = VECTOR ( 'NONE', #37404, 1000.000000000000000 ) ;
#37030 = CARTESIAN_POINT ( 'NONE',  ( 168.9999999999999716, -252.4999999999999432, -349.9999999999999432 ) ) ;
#37031 = ORIENTED_EDGE ( 'NONE', *, *, #7749, .F. ) ;
#37032 = CARTESIAN_POINT ( 'NONE',  ( 1.249999999999999778, 0.000000000000000000, 9.972675548442463622 ) ) ;
#37033 = B_SPLINE_CURVE_WITH_KNOTS ( 'NONE', 3,
 ( #30757, #37704, #46366, #2533 ),
 .UNSPECIFIED., .F., .F.,
 ( 4, 4 ),
 ( 1.409296014025916843E-17, 0.009404495247862340590 ),
 .UNSPECIFIED. ) ;
#37034 = CARTESIAN_POINT ( 'NONE',  ( 168.9999999999999716, 175.0000000000000284, -340.0000000000001137 ) ) ;
#37035 = DIRECTION ( 'NONE',  ( 0.000000000000000000, -0.9749645535258953943, 0.2223603367690637489 ) ) ;
#37036 = ORIENTED_EDGE ( 'NONE', *, *, #36630, .T. ) ;
#37037 = ORIENTED_EDGE ( 'NONE', *, *, #8552, .F. ) ;
#37038 = CARTESIAN_POINT ( 'NONE',  ( 164.9999999999999716, 17.00000000000000000, 4.999999999999990230 ) ) ;
#37039 = LINE ( 'NONE', #25206, #46767 ) ;
#37040 = CARTESIAN_POINT ( 'NONE',  ( 339.9999999999999432, 181.0000000000000284, -358.0000000000002274 ) ) ;
#37041 = CARTESIAN_POINT ( 'NONE',  ( 0.6440276692615888310, 16.64212148744554298, -9.683996418299976483 ) ) ;
#37042 = AXIS2_PLACEMENT_3D ( 'NONE', #26001, #33949, #41641 ) ;
#37043 = ORIENTED_EDGE ( 'NONE', *, *, #2483, .T. ) ;
#37044 = DIRECTION ( 'NONE',  ( -1.000000000000000000, -0.000000000000000000, -0.000000000000000000 ) ) ;
#37045 = ORIENTED_EDGE ( 'NONE', *, *, #19286, .T. ) ;
#37046 = DIRECTION ( 'NONE',  ( -1.000000000000000000, -0.000000000000000000, -0.000000000000000000 ) ) ;
#37047 = CARTESIAN_POINT ( 'NONE',  ( -215.0000000000000568, 164.9999999999999716, 497.2965085865002379 ) ) ;
#37048 = CARTESIAN_POINT ( 'NONE',  ( 154.3291528190321458, -1.750000000000009326, -158.1565861772249377 ) ) ;
#37049 = CYLINDRICAL_SURFACE ( 'NONE', #16013, 1.750000000000015543 ) ;
#37050 = CARTESIAN_POINT ( 'NONE',  ( 113.3040265531850537, 1.749999999999997335, 120.8182875569279702 ) ) ;
#37051 = CARTESIAN_POINT ( 'NONE',  ( -225.0000000000000568, -175.0000000000000000, 0.000000000000000000 ) ) ;
#37052 = VERTEX_POINT ( 'NONE', #19847 ) ;
#37053 = EDGE_CURVE ( 'NONE', #6217, #50559, #47767, .T. ) ;
#37054 = PLANE ( 'NONE',  #23928 ) ;
#37055 = CARTESIAN_POINT ( 'NONE',  ( 210.0000000000000568, 0.000000000000000000, 160.8182875569279702 ) ) ;
#37056 = LINE ( 'NONE', #1882, #39744 ) ;
#37057 = CARTESIAN_POINT ( 'NONE',  ( 50.11058929355270664, -7.578863168071591438, 7.455576670931136185 ) ) ;
#37058 = VERTEX_POINT ( 'NONE', #23712 ) ;
#37059 = PLANE ( 'NONE',  #47442 ) ;
#37060 = EDGE_LOOP ( 'NONE', ( #2316, #26428, #17116 ) ) ;
#37061 = CARTESIAN_POINT ( 'NONE',  ( 73.30402655318508209, -1.750000000000010658, -79.18171244307201562 ) ) ;
#37062 = VECTOR ( 'NONE', #22043, 1000.000000000000000 ) ;
#37063 = LINE ( 'NONE', #9336, #6151 ) ;
#37064 = DIRECTION ( 'NONE',  ( -0.000000000000000000, -1.000000000000000000, -0.000000000000000000 ) ) ;
#37065 = ORIENTED_EDGE ( 'NONE', *, *, #39511, .F. ) ;
#37066 = ORIENTED_EDGE ( 'NONE', *, *, #1148, .T. ) ;
#37067 = CIRCLE ( 'NONE', #15721, 4.000000000000003553 ) ;
#37068 = CARTESIAN_POINT ( 'NONE',  ( 85.00000000000090949, 16.00000000000000000, -24.99999999999999289 ) ) ;
#37069 = CARTESIAN_POINT ( 'NONE',  ( 7.749480817862238524, 14.85497772329518895, 9.403735324607438884 ) ) ;
#37070 = DIRECTION ( 'NONE',  ( -0.2599384441937671042, 0.8000082703740934997, 0.5407575913134970991 ) ) ;
#37071 = CARTESIAN_POINT ( 'NONE',  ( -164.9459734468149463, 2.143131898507880377E-16, 82.56828755692798438 ) ) ;
#37072 = ORIENTED_EDGE ( 'NONE', *, *, #32149, .T. ) ;
#37073 = ORIENTED_EDGE ( 'NONE', *, *, #16472, .F. ) ;
#37074 = CARTESIAN_POINT ( 'NONE',  ( -46.69597344681494633, 0.000000000000000000, 165.0000000000000000 ) ) ;
#37075 = CARTESIAN_POINT ( 'NONE',  ( 164.9999999999999716, 17.00000000000000000, 90.00000000000000000 ) ) ;
#37076 = EDGE_CURVE ( 'NONE', #47178, #12553, #31683, .T. ) ;
#37077 = ORIENTED_EDGE ( 'NONE', *, *, #4482, .F. ) ;
#37078 = ORIENTED_EDGE ( 'NONE', *, *, #46290, .F. ) ;
#37079 = DIRECTION ( 'NONE',  ( -1.000000000000000000, 0.000000000000000000, 0.000000000000000000 ) ) ;
#37080 = CARTESIAN_POINT ( 'NONE',  ( 34.32915281903212446, 1.750000000000009548, 41.84341382277508359 ) ) ;
#37081 = LINE ( 'NONE', #23433, #7909 ) ;
#37082 = LINE ( 'NONE', #1910, #11672 ) ;
#37083 = VERTEX_POINT ( 'NONE', #12654 ) ;
#37084 = EDGE_LOOP ( 'NONE', ( #21698, #11407, #37155 ) ) ;
#37085 = ORIENTED_EDGE ( 'NONE', *, *, #17474, .F. ) ;
#37086 = VECTOR ( 'NONE', #48051, 1000.000000000000000 ) ;
#37087 = CARTESIAN_POINT ( 'NONE',  ( -8.445973446814964092, -1.025126265847097207, -40.93171244307204404 ) ) ;
#37088 = DIRECTION ( 'NONE',  ( -1.000000000000000000, -0.000000000000000000, -0.000000000000000000 ) ) ;
#37089 = ORIENTED_EDGE ( 'NONE', *, *, #18398, .T. ) ;
#37090 =( GEOMETRIC_REPRESENTATION_CONTEXT ( 3 ) GLOBAL_UNCERTAINTY_ASSIGNED_CONTEXT ( ( #37392 ) ) GLOBAL_UNIT_ASSIGNED_CONTEXT ( ( #15317, #42242, #46557 ) ) REPRESENTATION_CONTEXT ( 'NONE', 'WORKASPACE' ) );
#37091 = ORIENTED_EDGE ( 'NONE', *, *, #8393, .F. ) ;
#37092 = CARTESIAN_POINT ( 'NONE',  ( 0.000000000000000000, 17.00000000000000000, 0.000000000000000000 ) ) ;
#37093 = AXIS2_PLACEMENT_3D ( 'NONE', #50463, #15370, #31283 ) ;
#37094 = CARTESIAN_POINT ( 'NONE',  ( -20.00000000000003197, 17.00000000000000000, -90.00000000000000000 ) ) ;
#37095 = ORIENTED_EDGE ( 'NONE', *, *, #16831, .T. ) ;
#37096 = ORIENTED_EDGE ( 'NONE', *, *, #30711, .T. ) ;
#37097 = COLOUR_RGB ( '',0.7921568627450980005, 0.8196078431372548767, 0.9333333333333333481 ) ;
#37098 = FACE_OUTER_BOUND ( 'NONE', #6140, .T. ) ;
#37099 = CYLINDRICAL_SURFACE ( 'NONE', #22301, 1.750000000000008438 ) ;
#37100 = ORIENTED_EDGE ( 'NONE', *, *, #47411, .T. ) ;
#37101 = DIRECTION ( 'NONE',  ( 1.000000000000000000, 0.000000000000000000, 0.000000000000000000 ) ) ;
#37102 = CARTESIAN_POINT ( 'NONE',  ( -204.9459734468149463, 2.143131898507880377E-16, 165.0000000000000000 ) ) ;
#37103 = CARTESIAN_POINT ( 'NONE',  ( 50.11058929355269953, -7.578863168071589662, 7.455576670931136185 ) ) ;
#37104 = DIRECTION ( 'NONE',  ( 0.000000000000000000, 0.2791762785758810650, -0.9602398687205827565 ) ) ;
#37105 = AXIS2_PLACEMENT_3D ( 'NONE', #20896, #44473, #23996 ) ;
#37106 = CARTESIAN_POINT ( 'NONE',  ( 185.0000000000000000, -174.9999999999999716, -340.0000000000001137 ) ) ;
#37107 = ORIENTED_EDGE ( 'NONE', *, *, #30281, .F. ) ;
#37108 = EDGE_CURVE ( 'NONE', #45829, #829, #8803, .T. ) ;
#37109 = FACE_OUTER_BOUND ( 'NONE', #20212, .T. ) ;
#37110 = FACE_OUTER_BOUND ( 'NONE', #49802, .T. ) ;
#37111 = DIRECTION ( 'NONE',  ( 0.8411784753765545464, 0.000000000000000000, 0.5407575913134972101 ) ) ;
#37112 = CARTESIAN_POINT ( 'NONE',  ( -36.80807479611529942, 7.357694319819784390, 1.982731392810406668 ) ) ;
#37113 = FACE_BOUND ( 'NONE', #43038, .T. ) ;
#37114 = FACE_OUTER_BOUND ( 'NONE', #34596, .T. ) ;
#37115 = CARTESIAN_POINT ( 'NONE',  ( 111.5540265531850537, 1.025126265847081886, 119.0682875569279702 ) ) ;
#37116 = EDGE_CURVE ( 'NONE', #37058, #14195, #27268, .T. ) ;
#37117 = DIRECTION ( 'NONE',  ( -1.121065046350011585E-16, -0.7071067811865475727, -0.7071067811865474617 ) ) ;
#37118 = VECTOR ( 'NONE', #7475, 1000.000000000000000 ) ;
#37119 = EDGE_CURVE ( 'NONE', #26888, #9206, #32428, .T. ) ;
#37120 = LINE ( 'NONE', #5792, #4205 ) ;
#37121 = EDGE_CURVE ( 'NONE', #16638, #25367, #12162, .T. ) ;
#37122 = ORIENTED_EDGE ( 'NONE', *, *, #41613, .F. ) ;
#37123 = CARTESIAN_POINT ( 'NONE',  ( -7.129058724845069861, -15.30620660340479766, 9.178419661560148768 ) ) ;
#37124 = DIRECTION ( 'NONE',  ( 0.9908916497796512735, -0.000000000000000000, 0.1346615698592613375 ) ) ;
#37125 = AXIS2_PLACEMENT_3D ( 'NONE', #43895, #24423, #4405 ) ;
#37126 = CARTESIAN_POINT ( 'NONE',  ( 1.401228687704787257, -0.7134216605332859285, 9.945241992664895392 ) ) ;
#37127 = CARTESIAN_POINT ( 'NONE',  ( 360.0000000000001137, 169.0000000000000000, 349.9999999999998295 ) ) ;
#37128 = VECTOR ( 'NONE', #43882, 999.9999999999998863 ) ;
#37129 = VERTEX_POINT ( 'NONE', #4719 ) ;
#37130 = DIRECTION ( 'NONE',  ( -0.000000000000000000, -0.000000000000000000, -1.000000000000000000 ) ) ;
#37131 = EDGE_CURVE ( 'NONE', #3587, #49828, #373, .T. ) ;
#37133 = ORIENTED_EDGE ( 'NONE', *, *, #47160, .F. ) ;
#37132 = ADVANCED_FACE ( 'NONE', ( #31930 ), #20357, .F. ) ;
#37134 = CARTESIAN_POINT ( 'NONE',  ( 210.0000000000000568, 0.000000000000000000, 0.8182875569279768335 ) ) ;
#37135 = AXIS2_PLACEMENT_3D ( 'NONE', #26367, #45818, #18901 ) ;
#37136 = CARTESIAN_POINT ( 'NONE',  ( -2.735100745861921201, 5.294958516888076616, 6.606856988583542645E-16 ) ) ;
#37137 = EDGE_CURVE ( 'NONE', #32721, #18711, #118, .T. ) ;
#37138 = EDGE_CURVE ( 'NONE', #31922, #31313, #28348, .T. ) ;
#37139 = EDGE_LOOP ( 'NONE', ( #5690, #12410, #30949, #42722 ) ) ;
#37140 = CARTESIAN_POINT ( 'NONE',  ( 8.277096487746778308, -33.14818118907697198, 7.455576670931136185 ) ) ;
#37141 = DIRECTION ( 'NONE',  ( 1.000000000000000000, 0.000000000000000000, 0.000000000000000000 ) ) ;
#37142 = ORIENTED_EDGE ( 'NONE', *, *, #16208, .T. ) ;
#37143 = ORIENTED_EDGE ( 'NONE', *, *, #7544, .F. ) ;
#37144 = ADVANCED_FACE ( 'NONE', ( #28317 ), #3097, .T. ) ;
#37145 =( BOUNDED_CURVE ( )  B_SPLINE_CURVE ( 3, ( #45463, #10359, #44961, #2155 ),
 .UNSPECIFIED., .F., .F. ) 
 B_SPLINE_CURVE_WITH_KNOTS ( ( 4, 4 ),
 ( 3.141592653589793116, 4.712388980384689674 ),
 .UNSPECIFIED. ) 
 CURVE ( )  GEOMETRIC_REPRESENTATION_ITEM ( )  RATIONAL_B_SPLINE_CURVE ( ( 1.000000000000000000, 0.8047378541243649375, 0.8047378541243649375, 1.000000000000000000 ) ) 
 REPRESENTATION_ITEM ( '' )  );
#37146 = CARTESIAN_POINT ( 'NONE',  ( 191.5540265531851105, 0.000000000000000000, 122.5682875569279702 ) ) ;
#37147 = CARTESIAN_POINT ( 'NONE',  ( 185.0000000000000000, 175.0000000000000284, -356.0000000000001705 ) ) ;
#37148 = CARTESIAN_POINT ( 'NONE',  ( -1.011271242968693862, 0.7347315653655780432, 10.00000000000000000 ) ) ;
#37149 = VERTEX_POINT ( 'NONE', #32672 ) ;
#37150 = LINE ( 'NONE', #975, #12837 ) ;
#37151 = PLANE ( 'NONE',  #6660 ) ;
#37152 = SURFACE_SIDE_STYLE ('',( #48622 ) ) ;
#37153 = ORIENTED_EDGE ( 'NONE', *, *, #30487, .F. ) ;
#37154 = ORIENTED_EDGE ( 'NONE', *, *, #42405, .T. ) ;
#37155 = ORIENTED_EDGE ( 'NONE', *, *, #42341, .F. ) ;
#37156 = CARTESIAN_POINT ( 'NONE',  ( 0.000000000000000000, 185.0000000000000284, 343.9999999999997726 ) ) ;
#37157 = DIRECTION ( 'NONE',  ( 1.333906992743555050E-23, -1.000000000000000000, 0.000000000000000000 ) ) ;
#37158 = ORIENTED_EDGE ( 'NONE', *, *, #12225, .F. ) ;
#37159 = EDGE_CURVE ( 'NONE', #46544, #49245, #50157, .T. ) ;
#37160 = FACE_OUTER_BOUND ( 'NONE', #15307, .T. ) ;
#37161 = EDGE_CURVE ( 'NONE', #1515, #17667, #36795, .T. ) ;
#37162 = FACE_OUTER_BOUND ( 'NONE', #24574, .T. ) ;
#37163 = CARTESIAN_POINT ( 'NONE',  ( 135.0000000000003411, 17.00000000000000000, -84.99999999999998579 ) ) ;
#37164 = EDGE_CURVE ( 'NONE', #27926, #31866, #3842, .T. ) ;
#37165 = VECTOR ( 'NONE', #25361, 1000.000000000000000 ) ;
#37166 = APPLICATION_CONTEXT ( 'automotive_design' ) ;
#37167 = PLANE ( 'NONE',  #24138 ) ;
#37168 = CARTESIAN_POINT ( 'NONE',  ( 194.3291528190321742, 1.750000000000009548, 1.843413822775065825 ) ) ;
#37169 = EDGE_CURVE ( 'NONE', #11965, #44183, #9811, .T. ) ;
#37170 = AXIS2_PLACEMENT_3D ( 'NONE', #14225, #41436, #14488 ) ;
#37171 = DIRECTION ( 'NONE',  ( 1.000000000000000000, 0.000000000000000000, -0.000000000000000000 ) ) ;
#37172 = DIRECTION ( 'NONE',  ( -1.000000000000000000, 0.000000000000000000, -0.000000000000000000 ) ) ;
#37173 = DIRECTION ( 'NONE',  ( 1.000000000000000000, 0.000000000000000000, 0.000000000000000000 ) ) ;
#37174 = AXIS2_PLACEMENT_3D ( 'NONE', #33397, #49487, #25686 ) ;
#37175 = ADVANCED_FACE ( 'NONE', ( #37551 ), #25988, .T. ) ;
#37176 = CARTESIAN_POINT ( 'NONE',  ( 0.3862712429686727678, 1.188820645368945605, 3.333333333333333481 ) ) ;
#37177 = CIRCLE ( 'NONE', #28943, 4.000000000000003553 ) ;
#37178 = CARTESIAN_POINT ( 'NONE',  ( -8.843309649387274263, 14.11631751497152720, -2.870787844569587133 ) ) ;
#37179 = ORIENTED_EDGE ( 'NONE', *, *, #31142, .T. ) ;
#37180 = LINE ( 'NONE', #25106, #4840 ) ;
#37181 = DIRECTION ( 'NONE',  ( -0.000000000000000000, -1.000000000000000000, -0.000000000000000000 ) ) ;
#37182 = B_SPLINE_CURVE_WITH_KNOTS ( 'NONE', 3,
 ( #20497, #48157, #36166, #1012 ),
 .UNSPECIFIED., .F., .F.,
 ( 4, 4 ),
 ( 0.9811748202683102660, 0.9878904167554125593 ),
 .UNSPECIFIED. ) ;
#37183 = LINE ( 'NONE', #44080, #26284 ) ;
#37184 = EDGE_LOOP ( 'NONE', ( #48850, #49696, #23006, #7523 ) ) ;
#37185 = CARTESIAN_POINT ( 'NONE',  ( -87.72109971266203843, 1.750000000000010436, -120.2068387089191219 ) ) ;
#37186 = VECTOR ( 'NONE', #31149, 1000.000000000000000 ) ;
#37187 = DIRECTION ( 'NONE',  ( 0.000000000000000000, 0.000000000000000000, -1.000000000000000000 ) ) ;
#37188 = EDGE_CURVE ( 'NONE', #1277, #32004, #13165, .T. ) ;
#37189 = ORIENTED_EDGE ( 'NONE', *, *, #31638, .F. ) ;
#37190 = CARTESIAN_POINT ( 'NONE',  ( 0.000000000000000000, 169.0000000000000000, -358.0000000000002274 ) ) ;
#37191 = LINE ( 'NONE', #2755, #48716 ) ;
#37192 = VERTEX_POINT ( 'NONE', #40630 ) ;
#37193 = CARTESIAN_POINT ( 'NONE',  ( 181.0000000000000284, -174.9999999999999716, -97.00000000000014211 ) ) ;
#37195 = VERTEX_POINT ( 'NONE', #48781 ) ;
#37194 = EDGE_CURVE ( 'NONE', #15096, #6217, #28821, .T. ) ;
#37196 = VERTEX_POINT ( 'NONE', #44936 ) ;
#37197 = CARTESIAN_POINT ( 'NONE',  ( -7.216980890441389462, 6.922079660550276792, 0.000000000000000000 ) ) ;
#37198 = EDGE_CURVE ( 'NONE', #20525, #8314, #13903, .T. ) ;
#37199 = EDGE_CURVE ( 'NONE', #34173, #15322, #5464, .T. ) ;
#37200 = ORIENTED_EDGE ( 'NONE', *, *, #8618, .F. ) ;
#37201 = DIRECTION ( 'NONE',  ( -1.000000000000000000, -0.000000000000000000, -0.000000000000000000 ) ) ;
#37202 = CARTESIAN_POINT ( 'NONE',  ( -6.695973446814940111, -1.750000000000024203, -79.18171244307201562 ) ) ;
#37203 = AXIS2_PLACEMENT_3D ( 'NONE', #36705, #17669, #16930 ) ;
#37204 = VERTEX_POINT ( 'NONE', #41120 ) ;
#37205 = CARTESIAN_POINT ( 'NONE',  ( 357.1715728752537302, 183.0000000000002558, -358.0000000000003979 ) ) ;
#37206 = PLANE ( 'NONE',  #39855 ) ;
#37207 = EDGE_CURVE ( 'NONE', #4486, #43884, #41900, .T. ) ;
#37208 = AXIS2_PLACEMENT_3D ( 'NONE', #6097, #17644, #32810 ) ;
#37209 = FACE_OUTER_BOUND ( 'NONE', #42287, .T. ) ;
#37210 = EDGE_CURVE ( 'NONE', #30152, #16044, #44442, .T. ) ;
#37211 = PLANE ( 'NONE',  #35820 ) ;
#37212 = ORIENTED_EDGE ( 'NONE', *, *, #3999, .F. ) ;
#37213 = AXIS2_PLACEMENT_3D ( 'NONE', #42019, #3509, #3784 ) ;
#37214 = DIRECTION ( 'NONE',  ( 0.000000000000000000, 1.000000000000000000, -1.822804496942679766E-16 ) ) ;
#37215 = CIRCLE ( 'NONE', #2776, 1.750000000000036193 ) ;
#37216 = ORIENTED_EDGE ( 'NONE', *, *, #10202, .T. ) ;
#37217 = CYLINDRICAL_SURFACE ( 'NONE', #14483, 2.000000000000001776 ) ;
#37218 = CARTESIAN_POINT ( 'NONE',  ( -164.9459734468149463, 2.143131898507880377E-16, -37.43171244307205825 ) ) ;
#37219 = ORIENTED_EDGE ( 'NONE', *, *, #50522, .F. ) ;
#37220 = ORIENTED_EDGE ( 'NONE', *, *, #29078, .T. ) ;
#37221 = VERTEX_POINT ( 'NONE', #6234 ) ;
#37222 = CARTESIAN_POINT ( 'NONE',  ( 339.9999999999999432, -182.9999999999999716, -344.0000000000001705 ) ) ;
#37223 = CARTESIAN_POINT ( 'NONE',  ( 210.0000000000000568, 0.000000000000000000, 122.5682875569279844 ) ) ;
#37224 = B_SPLINE_SURFACE_WITH_KNOTS ( 'NONE', 3, 3, ( 
 ( #22295, #14083, #37973, #26397 ),
 ( #25909, #23826, #15613, #7669 ),
 ( #12026, #22798, #7422, #11264 ),
 ( #43051, #38480, #3291, #30767 ) ),
 .UNSPECIFIED., .F., .F., .F.,
 ( 4, 4 ),
 ( 4, 4 ),
 ( 0.000000000000000000, 1.000000000000000000 ),
 ( 0.000000000000000000, 1.000000000000000000 ),
 .UNSPECIFIED. ) ;
#37225 = ORIENTED_EDGE ( 'NONE', *, *, #19223, .T. ) ;
#37226 = DIRECTION ( 'NONE',  ( 0.000000000000000000, 0.000000000000000000, 1.000000000000000000 ) ) ;
#37227 = DIRECTION ( 'NONE',  ( -0.000000000000000000, -0.000000000000000000, -1.000000000000000000 ) ) ;
#37228 = CARTESIAN_POINT ( 'NONE',  ( 169.0000000000000000, -9.999999999999953815, -97.00000000000014211 ) ) ;
#37229 = FACE_OUTER_BOUND ( 'NONE', #14079, .T. ) ;
#37230 = EDGE_CURVE ( 'NONE', #32429, #32609, #17328, .T. ) ;
#37231 = ORIENTED_EDGE ( 'NONE', *, *, #12100, .T. ) ;
#37232 =( BOUNDED_CURVE ( )  B_SPLINE_CURVE ( 3, ( #16657, #23603, #39525, #27712 ),
 .UNSPECIFIED., .F., .F. ) 
 B_SPLINE_CURVE_WITH_KNOTS ( ( 4, 4 ),
 ( 3.141592653589793116, 4.712388980384689674 ),
 .UNSPECIFIED. ) 
 CURVE ( )  GEOMETRIC_REPRESENTATION_ITEM ( )  RATIONAL_B_SPLINE_CURVE ( ( 1.000000000000000000, 0.8047378541243649375, 0.8047378541243649375, 1.000000000000000000 ) ) 
 REPRESENTATION_ITEM ( '' )  );
#37233 = CARTESIAN_POINT ( 'NONE',  ( 181.0000000000000000, -272.4999999999999432, -355.9999999999999432 ) ) ;
#37234 = DIRECTION ( 'NONE',  ( -0.000000000000000000, -0.000000000000000000, -1.000000000000000000 ) ) ;
#37235 = CARTESIAN_POINT ( 'NONE',  ( 151.5540265531850537, 0.000000000000000000, 162.5682875569279702 ) ) ;
#37236 = ORIENTED_EDGE ( 'NONE', *, *, #39456, .F. ) ;
#37237 = CARTESIAN_POINT ( 'NONE',  ( 71.55402655318505367, 0.000000000000000000, -77.43171244307198720 ) ) ;
#37238 = CARTESIAN_POINT ( 'NONE',  ( 8.843309649387377291, -14.11631751497145792, -2.870787844569587133 ) ) ;
#37239 = AXIS2_PLACEMENT_3D ( 'NONE', #21517, #16935, #25134 ) ;
#37240 = VECTOR ( 'NONE', #10163, 1000.000000000000000 ) ;
#37241 = CARTESIAN_POINT ( 'NONE',  ( -45.21167770612412085, -22.65616271077779942, 7.906207997025717304 ) ) ;
#37242 = CARTESIAN_POINT ( 'NONE',  ( -32.36066692128246558, 7.813306791043033606, 3.199614146704519602 ) ) ;
#37243 = VERTEX_POINT ( 'NONE', #37308 ) ;
#37244 = CARTESIAN_POINT ( 'NONE',  ( -8.445973446814976526, 0.000000000000000000, 122.5682875569279986 ) ) ;
#37245 = AXIS2_PLACEMENT_3D ( 'NONE', #6935, #3070, #2816 ) ;
#37246 = EDGE_CURVE ( 'NONE', #33102, #45555, #1628, .T. ) ;
#37247 = CARTESIAN_POINT ( 'NONE',  ( -164.4973046169135955, 103.0380105690400683, -17.46817021067766973 ) ) ;
#37248 = CYLINDRICAL_SURFACE ( 'NONE', #28581, 1.750000000000015543 ) ;
#37249 = FACE_OUTER_BOUND ( 'NONE', #33714, .T. ) ;
#37250 = VECTOR ( 'NONE', #41520, 1000.000000000000000 ) ;
#37251 = CYLINDRICAL_SURFACE ( 'NONE', #885, 5.000000000000000000 ) ;
#37252 = ORIENTED_EDGE ( 'NONE', *, *, #31784, .F. ) ;
#37253 = CARTESIAN_POINT ( 'NONE',  ( -168.4459734468149747, 1.025126265847088991, 2.568287556927986159 ) ) ;
#37254 = VERTEX_POINT ( 'NONE', #45188 ) ;
#37255 = CARTESIAN_POINT ( 'NONE',  ( -7.576114424932982594, 33.14742743729794938, 7.906207997025717304 ) ) ;
#37256 = EDGE_CURVE ( 'NONE', #40596, #20412, #32943, .T. ) ;
#37257 = ORIENTED_EDGE ( 'NONE', *, *, #44118, .F. ) ;
#37258 = DIRECTION ( 'NONE',  ( -1.000000000000000000, 0.000000000000000000, -0.000000000000000000 ) ) ;
#37259 = CARTESIAN_POINT ( 'NONE',  ( 360.0000000000001137, 169.0000000000000000, 343.9999999999998295 ) ) ;
#37260 = DIRECTION ( 'NONE',  ( -0.000000000000000000, -1.000000000000000000, -0.000000000000000000 ) ) ;
#37261 = ORIENTED_EDGE ( 'NONE', *, *, #34809, .F. ) ;
#37262 = EDGE_CURVE ( 'NONE', #5959, #15096, #29075, .T. ) ;
#37263 = VECTOR ( 'NONE', #13407, 1000.000000000000000 ) ;
#37264 = CARTESIAN_POINT ( 'NONE',  ( 7.499999999999944045, -224.9999999999999716, -224.9999999999999716 ) ) ;
#37265 = EDGE_CURVE ( 'NONE', #46038, #18302, #47405, .T. ) ;
#37266 = ORIENTED_EDGE ( 'NONE', *, *, #4042, .F. ) ;
#37267 = DIRECTION ( 'NONE',  ( 0.000000000000000000, 0.000000000000000000, -1.000000000000000000 ) ) ;
#37268 = LINE ( 'NONE', #17738, #6849 ) ;
#37269 = CARTESIAN_POINT ( 'NONE',  ( -164.9459734468149463, 1.025126265847089879, -77.43171244307200141 ) ) ;
#37270 = DIRECTION ( 'NONE',  ( -0.000000000000000000, -1.000000000000000000, -0.000000000000000000 ) ) ;
#37271 = FACE_OUTER_BOUND ( 'NONE', #36534, .T. ) ;
#37272 = VERTEX_POINT ( 'NONE', #25732 ) ;
#37273 = ADVANCED_FACE ( 'NONE', ( #42116 ), #18766, .F. ) ;
#37274 = ORIENTED_EDGE ( 'NONE', *, *, #49465, .T. ) ;
#37275 = CARTESIAN_POINT ( 'NONE',  ( 357.9999999999999432, -177.9999999999999147, -353.0000000000001705 ) ) ;
#37276 = EDGE_CURVE ( 'NONE', #30495, #27396, #50533, .T. ) ;
#37277 = ADVANCED_FACE ( 'NONE', ( #19276 ), #34968, .T. ) ;
#37278 = ORIENTED_EDGE ( 'NONE', *, *, #29967, .F. ) ;
#37279 = DIRECTION ( 'NONE',  ( 1.000000000000000000, 0.000000000000000000, -0.000000000000000000 ) ) ;
#37280 = VECTOR ( 'NONE', #29604, 1000.000000000000000 ) ;
#37281 = CARTESIAN_POINT ( 'NONE',  ( -1.769963848780949478, 9.842115015280430868, 0.000000000000000000 ) ) ;
#37282 = ORIENTED_EDGE ( 'NONE', *, *, #26230, .T. ) ;
#37283 = ADVANCED_FACE ( 'NONE', ( #10569 ), #49526, .F. ) ;
#37284 = CARTESIAN_POINT ( 'NONE',  ( 185.0000000000000000, -93.50000000000005684, -340.0000000000001137 ) ) ;
#37285 = EDGE_LOOP ( 'NONE', ( #26423, #20291, #27011, #26914 ) ) ;
#37286 = VECTOR ( 'NONE', #10055, 1000.000000000000000 ) ;
#37287 = CARTESIAN_POINT ( 'NONE',  ( 3.996390545799824334, -16.57371371864897469, 8.953103998512858652 ) ) ;
#37288 = DIRECTION ( 'NONE',  ( -1.000000000000000000, -0.000000000000000000, -0.000000000000000000 ) ) ;
#37289 = CARTESIAN_POINT ( 'NONE',  ( -88.44597344681497475, 0.000000000000000000, 79.06828755692795596 ) ) ;
#37290 =( BOUNDED_CURVE ( )  B_SPLINE_CURVE ( 3, ( #19100, #31949, #46770, #30938 ),
 .UNSPECIFIED., .F., .F. ) 
 B_SPLINE_CURVE_WITH_KNOTS ( ( 4, 4 ),
 ( 3.141592653589793116, 4.712388980384689674 ),
 .UNSPECIFIED. ) 
 CURVE ( )  GEOMETRIC_REPRESENTATION_ITEM ( )  RATIONAL_B_SPLINE_CURVE ( ( 1.000000000000000000, 0.8047378541243649375, 0.8047378541243649375, 1.000000000000000000 ) ) 
 REPRESENTATION_ITEM ( '' )  );
#37291 = LINE ( 'NONE', #3102, #29663 ) ;
#37292 = ORIENTED_EDGE ( 'NONE', *, *, #2087, .T. ) ;
#37293 = VERTEX_POINT ( 'NONE', #6981 ) ;
#37294 = DIRECTION ( 'NONE',  ( 0.000000000000000000, 0.000000000000000000, 1.000000000000000000 ) ) ;
#37295 = CARTESIAN_POINT ( 'NONE',  ( -47.72109971266203132, 1.750000000000009548, 41.84341382277508359 ) ) ;
#37296 = CARTESIAN_POINT ( 'NONE',  ( -46.69597344681494633, 1.750000000000010658, 80.81828755692798438 ) ) ;
#37297 =( BOUNDED_CURVE ( )  B_SPLINE_CURVE ( 3, ( #20309, #4902, #8781, #44639 ),
 .UNSPECIFIED., .F., .F. ) 
 B_SPLINE_CURVE_WITH_KNOTS ( ( 4, 4 ),
 ( 0.000000000000000000, 1.570796326794896558 ),
 .UNSPECIFIED. ) 
 CURVE ( )  GEOMETRIC_REPRESENTATION_ITEM ( )  RATIONAL_B_SPLINE_CURVE ( ( 1.000000000000000000, 0.8047378541243649375, 0.8047378541243649375, 1.000000000000000000 ) ) 
 REPRESENTATION_ITEM ( '' )  );
#37298 = DIRECTION ( 'NONE',  ( 0.000000000000000000, 0.000000000000000000, 1.000000000000000000 ) ) ;
#37299 = CARTESIAN_POINT ( 'NONE',  ( -45.67084718096785423, 1.750000000000010214, -80.20683870891910772 ) ) ;
#37300 = VERTEX_POINT ( 'NONE', #26233 ) ;
#37301 = CARTESIAN_POINT ( 'NONE',  ( 194.9999999999999432, 173.0000000000000000, 112.0000000000000000 ) ) ;
#37302 = ORIENTED_EDGE ( 'NONE', *, *, #42133, .F. ) ;
#37303 = CARTESIAN_POINT ( 'NONE',  ( 193.3040265531851105, -1.750000000000010658, -119.1817124430720440 ) ) ;
#37304 = DIRECTION ( 'NONE',  ( -0.000000000000000000, -0.000000000000000000, -1.000000000000000000 ) ) ;
#37305 = CARTESIAN_POINT ( 'NONE',  ( 193.3040265531851105, 0.000000000000000000, 165.0000000000000000 ) ) ;
#37306 = DIRECTION ( 'NONE',  ( 0.000000000000000000, 0.000000000000000000, 1.000000000000000000 ) ) ;
#37307 = DIRECTION ( 'NONE',  ( 0.000000000000000000, 0.000000000000000000, 1.000000000000000000 ) ) ;
#37308 = CARTESIAN_POINT ( 'NONE',  ( 339.9999999999998863, -166.9999999999999432, 343.9999999999997726 ) ) ;
#37309 = ORIENTED_EDGE ( 'NONE', *, *, #31638, .T. ) ;
#37310 = CARTESIAN_POINT ( 'NONE',  ( 195.0540265531851105, -1.025126265847089435, -40.93171244307204404 ) ) ;
#37311 = DIRECTION ( 'NONE',  ( -1.000000000000000000, 0.000000000000000000, 0.000000000000000000 ) ) ;
#37312 = CARTESIAN_POINT ( 'NONE',  ( 80.00000000000122213, 16.00000000000000000, 5.000000000000004441 ) ) ;
#37313 = EDGE_CURVE ( 'NONE', #16019, #36974, #6723, .T. ) ;
#37314 = CARTESIAN_POINT ( 'NONE',  ( 339.9999999999998863, -180.9999999999999716, 343.9999999999997726 ) ) ;
#37315 = EDGE_LOOP ( 'NONE', ( #6326, #11804, #44576, #27004, #8357, #38264 ) ) ;
#37316 = VECTOR ( 'NONE', #6248, 1000.000000000000000 ) ;
#37317 = DIRECTION ( 'NONE',  ( 1.000000000000000000, 0.000000000000000000, 0.000000000000000000 ) ) ;
#37318 = ORIENTED_EDGE ( 'NONE', *, *, #44118, .T. ) ;
#37319 = CARTESIAN_POINT ( 'NONE',  ( -9.281355226777547429, 3.722424633806451943, 0.000000000000000000 ) ) ;
#37320 = CARTESIAN_POINT ( 'NONE',  ( 0.8603719846014596939, -1.073163306097343783, 9.972175347158279024 ) ) ;
#37321 = CARTESIAN_POINT ( 'NONE',  ( 26.20171990995799760, -42.76673505352026439, -8.466730184410787174 ) ) ;
#37322 = VECTOR ( 'NONE', #22740, 1000.000000000000000 ) ;
#37323 = EDGE_CURVE ( 'NONE', #35256, #36058, #15438, .T. ) ;
#37324 = EDGE_CURVE ( 'NONE', #45368, #39651, #22126, .T. ) ;
#37325 = CARTESIAN_POINT ( 'NONE',  ( 7.129058724844953510, 15.30620660340485095, 9.178419661560148768 ) ) ;
#37326 = CARTESIAN_POINT ( 'NONE',  ( -165.3973046169136012, 54.43801056904003133, -17.65743994998275213 ) ) ;
#37327 = CARTESIAN_POINT ( 'NONE',  ( 177.5000000000000284, 102.5000000000000142, -8.474599139414886295 ) ) ;
#37328 = CARTESIAN_POINT ( 'NONE',  ( 17.23491422248386584, -0.5912720620000816441, 8.727788335465566760 ) ) ;
#37329 = ORIENTED_EDGE ( 'NONE', *, *, #16412, .T. ) ;
#37330 = ORIENTED_EDGE ( 'NONE', *, *, #18676, .T. ) ;
#37331 = CARTESIAN_POINT ( 'NONE',  ( -0.8738110990267208278, -1.684976543153730244, 9.900811091504552408 ) ) ;
#37332 = CARTESIAN_POINT ( 'NONE',  ( 31.28234235046230793, 11.28615439405779064, -3.760136334089591248 ) ) ;
#37333 = ADVANCED_FACE ( 'NONE', ( #50023 ), #23129, .F. ) ;
#37334 = EDGE_CURVE ( 'NONE', #49333, #38434, #37799, .T. ) ;
#37335 = VECTOR ( 'NONE', #16092, 1000.000000000000000 ) ;
#37336 = ORIENTED_EDGE ( 'NONE', *, *, #41208, .T. ) ;
#37337 = ORIENTED_EDGE ( 'NONE', *, *, #1859, .T. ) ;
#37338 = CARTESIAN_POINT ( 'NONE',  ( 155.0540265531850537, 1.025126265847089879, -77.43171244307200141 ) ) ;
#37339 = DIRECTION ( 'NONE',  ( 0.000000000000000000, -1.580451535867971417E-48, 1.000000000000000000 ) ) ;
#37340 = CARTESIAN_POINT ( 'NONE',  ( 210.0000000000000568, 0.000000000000000000, -37.43171244307202272 ) ) ;
#37341 = DIRECTION ( 'NONE',  ( -0.000000000000000000, -1.000000000000000000, -0.000000000000000000 ) ) ;
#37342 = VECTOR ( 'NONE', #6101, 1000.000000000000000 ) ;
#37343 = VERTEX_POINT ( 'NONE', #26480 ) ;
#37344 = EDGE_CURVE ( 'NONE', #20584, #18366, #23172, .T. ) ;
#37345 = VERTEX_POINT ( 'NONE', #14428 ) ;
#37346 = AXIS2_PLACEMENT_3D ( 'NONE', #27746, #7746, #4395 ) ;
#37347 = DIRECTION ( 'NONE',  ( 0.000000000000000000, 1.000000000000000000, 0.000000000000000000 ) ) ;
#37349 = VECTOR ( 'NONE', #9809, 1000.000000000000000 ) ;
#37348 = CYLINDRICAL_SURFACE ( 'NONE', #30666, 3.749999999999975575 ) ;
#37350 = VECTOR ( 'NONE', #37101, 1000.000000000000000 ) ;
#37351 = ORIENTED_EDGE ( 'NONE', *, *, #31803, .F. ) ;
#37352 = VECTOR ( 'NONE', #1735, 1000.000000000000000 ) ;
#37353 = EDGE_LOOP ( 'NONE', ( #13757, #12494, #28960, #10518 ) ) ;
#37354 = PLANE ( 'NONE',  #42316 ) ;
#37355 = CARTESIAN_POINT ( 'NONE',  ( 169.0000000000000284, 175.0000000000000284, 355.9999999999998863 ) ) ;
#37356 = PRODUCT_DEFINITION_FORMATION_WITH_SPECIFIED_SOURCE ( 'ANY', '', #44939, .NOT_KNOWN. ) ;
#37357 = EDGE_LOOP ( 'NONE', ( #35798, #26346, #856, #16045 ) ) ;
#37358 = ORIENTED_EDGE ( 'NONE', *, *, #13591, .F. ) ;
#37359 = AXIS2_PLACEMENT_3D ( 'NONE', #16134, #31290, #19724 ) ;
#37360 = CARTESIAN_POINT ( 'NONE',  ( -3.888415560953798700, -9.227494953140025657, 3.092310436554650543 ) ) ;
#37361 = CARTESIAN_POINT ( 'NONE',  ( -15.62858259096117841, 5.755205073598719245, -9.683996418299976483 ) ) ;
#37362 = ORIENTED_EDGE ( 'NONE', *, *, #20797, .F. ) ;
#37363 = CARTESIAN_POINT ( 'NONE',  ( 85.00000000000056843, 16.00000000000000000, -30.00000000000000000 ) ) ;
#37364 = CARTESIAN_POINT ( 'NONE',  ( 181.0000000000000000, -180.9999999999999716, -350.0000000000001705 ) ) ;
#37365 = PLANE ( 'NONE',  #10661 ) ;
#37366 = CARTESIAN_POINT ( 'NONE',  ( 115.0540265531850395, 2.143131898507847836E-16, 165.0000000000000000 ) ) ;
#37367 = ORIENTED_EDGE ( 'NONE', *, *, #32789, .T. ) ;
#37368 = LINE ( 'NONE', #2191, #34559 ) ;
#37369 = LINE ( 'NONE', #1939, #43296 ) ;
#37370 = CARTESIAN_POINT ( 'NONE',  ( 358.3431457505075741, -185.0000000000001421, -360.0000000000003411 ) ) ;
#37371 = EDGE_CURVE ( 'NONE', #27608, #43697, #30090, .T. ) ;
#37372 = VECTOR ( 'NONE', #12364, 999.9999999999998863 ) ;
#37373 = CARTESIAN_POINT ( 'NONE',  ( 166.9999999999999716, 175.0000000000000284, -356.0000000000001705 ) ) ;
#37374 = VECTOR ( 'NONE', #20905, 1000.000000000000000 ) ;
#37375 = CARTESIAN_POINT ( 'NONE',  ( 1.448406091252584238, -0.9360325558322883932, 9.928159647716132241 ) ) ;
#37376 = CARTESIAN_POINT ( 'NONE',  ( -1.448406091252275818, 0.9360325558308429938, 9.928159647716187308 ) ) ;
#37377 = VECTOR ( 'NONE', #5529, 1000.000000000000000 ) ;
#37378 = DIRECTION ( 'NONE',  ( -0.1191452206184307472, 0.000000000000000000, 0.9928768384869219865 ) ) ;
#37379 = ORIENTED_EDGE ( 'NONE', *, *, #31834, .T. ) ;
#37380 = CARTESIAN_POINT ( 'NONE',  ( 111.5540265531850537, 1.025126265847081664, 122.5682875569279702 ) ) ;
#37381 = VECTOR ( 'NONE', #46443, 1000.000000000000000 ) ;
#37382 = DIRECTION ( 'NONE',  ( 0.9928768384869219865, 0.000000000000000000, 0.1191452206184307749 ) ) ;
#37383 = B_SPLINE_CURVE_WITH_KNOTS ( 'NONE', 3,
 ( #32606, #30017, #14348, #25401 ),
 .UNSPECIFIED., .F., .F.,
 ( 4, 4 ),
 ( 0.7998230999345287140, 0.9869080488566185361 ),
 .UNSPECIFIED. ) ;
#37384 = AXIS2_PLACEMENT_3D ( 'NONE', #30580, #50013, #19006 ) ;
#37385 = CARTESIAN_POINT ( 'NONE',  ( -1.553324196727134954, 1.431239106454489152, 9.890170120223999106 ) ) ;
#37386 = DIRECTION ( 'NONE',  ( 0.000000000000000000, 1.000000000000000000, 0.000000000000000000 ) ) ;
#37387 = LINE ( 'NONE', #17346, #13522 ) ;
#37388 = EDGE_LOOP ( 'NONE', ( #4299, #48876, #21755, #35267, #8376, #3899 ) ) ;
#37389 = ORIENTED_EDGE ( 'NONE', *, *, #13260, .T. ) ;
#37390 = CARTESIAN_POINT ( 'NONE',  ( -167.7210997126620384, 1.750000000000009548, -38.15658617722494483 ) ) ;
#37391 = CARTESIAN_POINT ( 'NONE',  ( -165.0000000000000284, 16.00000000000000000, 115.0000000000000142 ) ) ;
#37392 = UNCERTAINTY_MEASURE_WITH_UNIT (LENGTH_MEASURE( 1.000000000000000082E-05 ), #15317, 'distance_accuracy_value', 'NONE');
#37393 = VERTEX_POINT ( 'NONE', #3118 ) ;
#37394 = DIRECTION ( 'NONE',  ( -0.000000000000000000, -1.000000000000000000, 2.537652627714643577E-15 ) ) ;
#37395 = EDGE_LOOP ( 'NONE', ( #33599, #17351, #20189 ) ) ;
#37396 = EDGE_LOOP ( 'NONE', ( #9219, #44478, #44290, #15861 ) ) ;
#37397 = EDGE_CURVE ( 'NONE', #50570, #45549, #49774, .T. ) ;
#37398 = ORIENTED_EDGE ( 'NONE', *, *, #40106, .T. ) ;
#37399 = LINE ( 'NONE', #33288, #22509 ) ;
#37400 = CARTESIAN_POINT ( 'NONE',  ( 49.89397392339123627, -8.245536726716670373, 7.906207997025717304 ) ) ;
#37401 = CARTESIAN_POINT ( 'NONE',  ( -16.71930270649968620, -33.57409379679878469, 8.506357886886739550 ) ) ;
#37402 = ORIENTED_EDGE ( 'NONE', *, *, #34475, .F. ) ;
#37403 = CARTESIAN_POINT ( 'NONE',  ( 85.00000000000123634, 17.00000000000000000, 5.000000000000004441 ) ) ;
#37404 = DIRECTION ( 'NONE',  ( -1.000000000000000000, -0.000000000000000000, -0.000000000000000000 ) ) ;
#37405 = CARTESIAN_POINT ( 'NONE',  ( 13.92102703536701114, 30.85732372859822803, 8.356839323120299312 ) ) ;
#37406 = EDGE_LOOP ( 'NONE', ( #38794, #34318, #7533, #8454, #26762, #27124 ) ) ;
#37407 = VECTOR ( 'NONE', #20339, 1000.000000000000000 ) ;
#37408 = ORIENTED_EDGE ( 'NONE', *, *, #32558, .F. ) ;
#37409 = DIRECTION ( 'NONE',  ( 1.612977847700450206E-50, 0.000000000000000000, 1.000000000000000000 ) ) ;
#37410 = CARTESIAN_POINT ( 'NONE',  ( 111.5540265531850679, 0.000000000000000000, 122.5682875569279560 ) ) ;
#37411 = ORIENTED_EDGE ( 'NONE', *, *, #49136, .T. ) ;
#37412 = CARTESIAN_POINT ( 'NONE',  ( -164.9459734468149463, 2.143131898507890731E-16, 165.0000000000000000 ) ) ;
#37413 = CARTESIAN_POINT ( 'NONE',  ( -69.99999999999816680, 17.00000000000000000, 65.00000000000000000 ) ) ;
#37414 = VECTOR ( 'NONE', #17987, 1000.000000000000000 ) ;
#37415 = CARTESIAN_POINT ( 'NONE',  ( 2.052570692346796122, -0.2041439924650269022, 9.889206917020301191 ) ) ;
#37416 = AXIS2_PLACEMENT_3D ( 'NONE', #20730, #6088, #28683 ) ;
#37417 = CARTESIAN_POINT ( 'NONE',  ( -14.99999999999845812, 16.00000000000000000, 60.00000000000000000 ) ) ;
#37418 = FACE_OUTER_BOUND ( 'NONE', #46796, .T. ) ;
#37419 = LINE ( 'NONE', #26091, #22599 ) ;
#37420 = CARTESIAN_POINT ( 'NONE',  ( -239.0000000000000853, -165.6999999999999602, 254.8599999999999852 ) ) ;
#37421 = FACE_OUTER_BOUND ( 'NONE', #47622, .T. ) ;
#37422 = VECTOR ( 'NONE', #29538, 1000.000000000000000 ) ;
#37423 = DIRECTION ( 'NONE',  ( -0.000000000000000000, -0.000000000000000000, -1.000000000000000000 ) ) ;
#37424 =( BOUNDED_CURVE ( )  B_SPLINE_CURVE ( 3, ( #48384, #41491, #6342, #2982 ),
 .UNSPECIFIED., .F., .F. ) 
 B_SPLINE_CURVE_WITH_KNOTS ( ( 4, 4 ),
 ( 3.141592653589793116, 4.712388980384689674 ),
 .UNSPECIFIED. ) 
 CURVE ( )  GEOMETRIC_REPRESENTATION_ITEM ( )  RATIONAL_B_SPLINE_CURVE ( ( 1.000000000000000000, 0.8047378541243649375, 0.8047378541243649375, 1.000000000000000000 ) ) 
 REPRESENTATION_ITEM ( '' )  );
#37425 = CARTESIAN_POINT ( 'NONE',  ( 85.00000000000152056, 17.00000000000000000, 35.00000000000000000 ) ) ;
#37426 = ORIENTED_EDGE ( 'NONE', *, *, #14179, .F. ) ;
#37427 = DIRECTION ( 'NONE',  ( 0.000000000000000000, -0.000000000000000000, -1.000000000000000000 ) ) ;
#37428 = CARTESIAN_POINT ( 'NONE',  ( -37.19569680397831490, 4.820783179364701354, 8.100132398494512387 ) ) ;
#37429 = CARTESIAN_POINT ( 'NONE',  ( -85.67084718096784002, 1.750000000000009548, -158.1565861772249377 ) ) ;
#37430 = ORIENTED_EDGE ( 'NONE', *, *, #30288, .F. ) ;
#37431 = DIRECTION ( 'NONE',  ( 1.000000000000000000, 0.000000000000000000, -1.224646799147353207E-16 ) ) ;
#37432 = AXIS2_PLACEMENT_3D ( 'NONE', #5819, #33033, #40976 ) ;
#37433 = CARTESIAN_POINT ( 'NONE',  ( 193.3040265531851105, 0.000000000000000000, 165.0000000000000000 ) ) ;
#37434 = VECTOR ( 'NONE', #29368, 1000.000000000000000 ) ;
#37435 = ORIENTED_EDGE ( 'NONE', *, *, #46995, .T. ) ;
#37436 = CARTESIAN_POINT ( 'NONE',  ( 1.424123654779712922, 0.3625862473308184009, 9.958264684458541183 ) ) ;
#37437 = CARTESIAN_POINT ( 'NONE',  ( -8.445973446814964092, -1.025126265847097429, 119.0682875569279133 ) ) ;
#37438 = CARTESIAN_POINT ( 'NONE',  ( -126.6959734468149321, 1.749999999999996891, 0.8182875569279768335 ) ) ;
#37439 = LINE ( 'NONE', #48657, #21690 ) ;
#37440 =( BOUNDED_CURVE ( )  B_SPLINE_CURVE ( 3, ( #13219, #1684, #44757, #25277 ),
 .UNSPECIFIED., .F., .F. ) 
 B_SPLINE_CURVE_WITH_KNOTS ( ( 4, 4 ),
 ( 1.570796326794896558, 3.141592653589793116 ),
 .UNSPECIFIED. ) 
 CURVE ( )  GEOMETRIC_REPRESENTATION_ITEM ( )  RATIONAL_B_SPLINE_CURVE ( ( 1.000000000000000000, 0.8047378541243649375, 0.8047378541243649375, 1.000000000000000000 ) ) 
 REPRESENTATION_ITEM ( '' )  );
#37441 = ORIENTED_EDGE ( 'NONE', *, *, #23360, .F. ) ;
#37442 = DIRECTION ( 'NONE',  ( -1.000000000000000000, -0.000000000000000000, -0.000000000000000000 ) ) ;
#37443 = VERTEX_POINT ( 'NONE', #34705 ) ;
#37444 = ORIENTED_EDGE ( 'NONE', *, *, #15214, .F. ) ;
#37445 = CARTESIAN_POINT ( 'NONE',  ( -86.69597344681494633, -1.750000000000010214, -39.18171244307202983 ) ) ;
#37446 = ADVANCED_FACE ( 'NONE', ( #7236 ), #28985, .T. ) ;
#37447 = VERTEX_POINT ( 'NONE', #811 ) ;
#37448 = CARTESIAN_POINT ( 'NONE',  ( -119.9999999999997158, 17.00000000000000000, -84.99999999999998579 ) ) ;
#37449 = CARTESIAN_POINT ( 'NONE',  ( -88.44597344681494633, 1.025126265847089435, 122.5682875569280128 ) ) ;
#37450 = ORIENTED_EDGE ( 'NONE', *, *, #39438, .T. ) ;
#37451 = FACE_OUTER_BOUND ( 'NONE', #46407, .T. ) ;
#37452 = EDGE_CURVE ( 'NONE', #23796, #35947, #31865, .T. ) ;
#37453 = LINE ( 'NONE', #5365, #43758 ) ;
#37454 = CARTESIAN_POINT ( 'NONE',  ( 0.000000000000000000, -168.9999999999999432, -344.0000000000001705 ) ) ;
#37455 = ORIENTED_EDGE ( 'NONE', *, *, #33389, .T. ) ;
#37456 = EDGE_CURVE ( 'NONE', #14077, #28486, #40064, .T. ) ;
#37457 = CIRCLE ( 'NONE', #23528, 10.00000000000000000 ) ;
#37458 = DIRECTION ( 'NONE',  ( 0.000000000000000000, 0.000000000000000000, 1.000000000000000000 ) ) ;
#37459 = DIRECTION ( 'NONE',  ( -0.000000000000000000, -0.000000000000000000, -1.000000000000000000 ) ) ;
#37460 = EDGE_CURVE ( 'NONE', #16730, #48110, #33024, .T. ) ;
#37461 = CARTESIAN_POINT ( 'NONE',  ( -5.000000000000000000, 165.2000000000000171, -359.8000000000002387 ) ) ;
#37462 = VERTEX_POINT ( 'NONE', #32361 ) ;
#37463 = LINE ( 'NONE', #1289, #27581 ) ;
#37464 = CYLINDRICAL_SURFACE ( 'NONE', #17942, 2.000000000000001776 ) ;
#37465 = ORIENTED_EDGE ( 'NONE', *, *, #17538, .F. ) ;
#37466 = VERTEX_POINT ( 'NONE', #16693 ) ;
#37467 = ORIENTED_EDGE ( 'NONE', *, *, #5814, .F. ) ;
#37468 = DIRECTION ( 'NONE',  ( -0.000000000000000000, -1.000000000000000000, -0.000000000000000000 ) ) ;
#37469 = CARTESIAN_POINT ( 'NONE',  ( 36.08557433729230013, -35.58569447144767395, 7.455576670931136185 ) ) ;
#37470 = VERTEX_POINT ( 'NONE', #43891 ) ;
#37471 = CARTESIAN_POINT ( 'NONE',  ( -207.7210997126620384, 1.750000000000009548, -0.2068387089191121020 ) ) ;
#37472 = CARTESIAN_POINT ( 'NONE',  ( 2.945500763482279627, 16.64098165802040086, -9.008049429158100807 ) ) ;
#37473 = CARTESIAN_POINT ( 'NONE',  ( 370.7621192902014968, 69.44873401059479079, -93.79675437945473959 ) ) ;
#37474 = CARTESIAN_POINT ( 'NONE',  ( 193.3040265531851105, -1.750000000000010658, 80.81828755692798438 ) ) ;
#37475 = AXIS2_PLACEMENT_3D ( 'NONE', #30014, #9736, #41297 ) ;
#37476 = VERTEX_POINT ( 'NONE', #35730 ) ;
#37477 = DIRECTION ( 'NONE',  ( -1.586032892321652236E-16, -1.000000000000000000, -6.853681917100419162E-49 ) ) ;
#37478 = CARTESIAN_POINT ( 'NONE',  ( -86.69597344681494633, 1.750000000000010658, -79.18171244307201562 ) ) ;
#37479 = CARTESIAN_POINT ( 'NONE',  ( 0.3862712429686894766, -1.188820645368940276, -10.00000000000000000 ) ) ;
#37480 = EDGE_CURVE ( 'NONE', #7928, #16503, #37177, .T. ) ;
#37481 = EDGE_CURVE ( 'NONE', #7355, #22572, #12678, .T. ) ;
#37482 = ADVANCED_BREP_SHAPE_REPRESENTATION ( '', ( #5787, #45486 ), #43870 ) ;
#37483 = VERTEX_POINT ( 'NONE', #20551 ) ;
#37484 = CONTEXT_DEPENDENT_SHAPE_REPRESENTATION ( #16169, #15522 ) ;
#37485 = FACE_OUTER_BOUND ( 'NONE', #43965, .T. ) ;
#37486 = CARTESIAN_POINT ( 'NONE',  ( -2.089000987151039102, -7.666878472664052424, 9.432811472610138637 ) ) ;
#37487 = EDGE_CURVE ( 'NONE', #42500, #1045, #46113, .T. ) ;
#37488 = EDGE_CURVE ( 'NONE', #31049, #29572, #27994, .T. ) ;
#37489 = DIRECTION ( 'NONE',  ( -3.469446951953611231E-16, -0.000000000000000000, -1.000000000000000000 ) ) ;
#37490 = CARTESIAN_POINT ( 'NONE',  ( 210.0000000000000568, 0.000000000000000000, -119.1817124430720440 ) ) ;
#37491 = ORIENTED_EDGE ( 'NONE', *, *, #34484, .T. ) ;
#37492 = EDGE_CURVE ( 'NONE', #25713, #38146, #12092, .T. ) ;
#37493 = LINE ( 'NONE', #2306, #41097 ) ;
#37494 = FACE_OUTER_BOUND ( 'NONE', #41259, .T. ) ;
#37495 = ADVANCED_FACE ( 'NONE', ( #24418 ), #36220, .F. ) ;
#37496 = DIRECTION ( 'NONE',  ( 0.000000000000000000, 0.000000000000000000, 1.000000000000000000 ) ) ;
#37497 = DIRECTION ( 'NONE',  ( -1.000000000000000000, -0.000000000000000000, -0.000000000000000000 ) ) ;
#37498 = EDGE_LOOP ( 'NONE', ( #19128, #47048, #20503, #8776, #28714, #26697 ) ) ;
#37499 = DIRECTION ( 'NONE',  ( -0.000000000000000000, -0.000000000000000000, -1.000000000000000000 ) ) ;
#37500 = ORIENTED_EDGE ( 'NONE', *, *, #6058, .T. ) ;
#37501 = CARTESIAN_POINT ( 'NONE',  ( -4.945973446814903696, 2.143131898507912917E-16, 42.56828755692802702 ) ) ;
#37502 = EDGE_LOOP ( 'NONE', ( #38925, #1679, #20439, #35617, #3571 ) ) ;
#37503 = DIRECTION ( 'NONE',  ( -0.000000000000000000, -0.000000000000000000, -1.000000000000000000 ) ) ;
#37504 = FACE_OUTER_BOUND ( 'NONE', #37315, .T. ) ;
#37505 = SURFACE_SIDE_STYLE ('',( #21839 ) ) ;
#37506 = EDGE_CURVE ( 'NONE', #3572, #50585, #31418, .T. ) ;
#37507 = VERTEX_POINT ( 'NONE', #27501 ) ;
#37508 = EDGE_CURVE ( 'NONE', #37300, #13105, #22789, .T. ) ;
#37509 = CARTESIAN_POINT ( 'NONE',  ( 196.8526953830863135, -154.8119894309599260, 472.8425600500171981 ) ) ;
#37510 = EDGE_CURVE ( 'NONE', #339, #47355, #49000, .T. ) ;
#37511 = ORIENTED_EDGE ( 'NONE', *, *, #32922, .F. ) ;
#37512 = CARTESIAN_POINT ( 'NONE',  ( 194.3291528190321742, 1.750000000000009326, 161.8434138227750907 ) ) ;
#37513 = CARTESIAN_POINT ( 'NONE',  ( 210.0000000000000568, 0.000000000000000000, 2.568287556927987048 ) ) ;
#37514 = CARTESIAN_POINT ( 'NONE',  ( -48.44597344681495343, 0.000000000000000000, -40.93171244307205825 ) ) ;
#37515 = DIRECTION ( 'NONE',  ( -1.000000000000000000, 0.000000000000000000, 0.000000000000000000 ) ) ;
#37516 = VERTEX_POINT ( 'NONE', #47206 ) ;
#37517 = VERTEX_POINT ( 'NONE', #312 ) ;
#37518 = VERTEX_POINT ( 'NONE', #23897 ) ;
#37519 = DIRECTION ( 'NONE',  ( 0.000000000000000000, 0.000000000000000000, 1.000000000000000000 ) ) ;
#37520 = CARTESIAN_POINT ( 'NONE',  ( 0.05286079371170563507, -1.230216489825521009, 9.975326647350893694 ) ) ;
#37521 =( BOUNDED_CURVE ( )  B_SPLINE_CURVE ( 3, ( #43030, #19698, #28162, #27146 ),
 .UNSPECIFIED., .F., .F. ) 
 B_SPLINE_CURVE_WITH_KNOTS ( ( 4, 4 ),
 ( 0.000000000000000000, 1.570796326794896558 ),
 .UNSPECIFIED. ) 
 CURVE ( )  GEOMETRIC_REPRESENTATION_ITEM ( )  RATIONAL_B_SPLINE_CURVE ( ( 1.000000000000000000, 0.8047378541243649375, 0.8047378541243649375, 1.000000000000000000 ) ) 
 REPRESENTATION_ITEM ( '' )  );
#37522 = VERTEX_POINT ( 'NONE', #39562 ) ;
#37523 = DIRECTION ( 'NONE',  ( -0.000000000000000000, -0.000000000000000000, -1.000000000000000000 ) ) ;
#37524 = ADVANCED_FACE ( 'NONE', ( #48948 ), #33515, .T. ) ;
#37525 = CARTESIAN_POINT ( 'NONE',  ( 356.0000000000000568, 165.0000000000000000, -94.00000000000019895 ) ) ;
#37526 = B_SPLINE_SURFACE_WITH_KNOTS ( 'NONE', 3, 3, ( 
 ( #49998, #38278, #18228, #5931 ),
 ( #14901, #26444, #2336, #48981 ),
 ( #49241, #38014, #34171, #37766 ),
 ( #45410, #14644, #45913, #10792 ) ),
 .UNSPECIFIED., .F., .F., .F.,
 ( 4, 4 ),
 ( 4, 4 ),
 ( 0.000000000000000000, 1.000000000000000000 ),
 ( 0.000000000000000000, 1.000000000000000000 ),
 .UNSPECIFIED. ) ;
#37527 = VERTEX_POINT ( 'NONE', #41060 ) ;
#37528 = CARTESIAN_POINT ( 'NONE',  ( 1.212058190970869198, 0.1697289529807369801, 9.966990782790126957 ) ) ;
#37529 = CARTESIAN_POINT ( 'NONE',  ( 210.0000000000000568, 0.000000000000000000, 120.8182875569279702 ) ) ;
#37530 = CARTESIAN_POINT ( 'NONE',  ( 8.277096487746778308, -50.00000000000000000, 7.455576670931136185 ) ) ;
#37531 = CARTESIAN_POINT ( 'NONE',  ( -206.6959734468149463, 1.750000000000009992, 160.8182875569279702 ) ) ;
#37532 = CARTESIAN_POINT ( 'NONE',  ( 210.0000000000000568, 2.143131898507881856E-16, -120.9317124430720582 ) ) ;
#37533 = ORIENTED_EDGE ( 'NONE', *, *, #42158, .F. ) ;
#37534 = VERTEX_POINT ( 'NONE', #1563 ) ;
#37535 = EDGE_CURVE ( 'NONE', #9801, #8676, #33380, .T. ) ;
#37536 = ORIENTED_EDGE ( 'NONE', *, *, #1733, .T. ) ;
#37537 = CARTESIAN_POINT ( 'NONE',  ( -119.9999999999994174, 16.00000000000000000, -54.99999999999999289 ) ) ;
#37538 = FACE_OUTER_BOUND ( 'NONE', #33959, .T. ) ;
#37539 = LINE ( 'NONE', #33433, #29701 ) ;
#37540 = EDGE_LOOP ( 'NONE', ( #34047, #7250, #9274, #32342 ) ) ;
#37541 = CARTESIAN_POINT ( 'NONE',  ( 113.3040265531850537, 1.749999999999997113, 40.81828755692798438 ) ) ;
#37542 = VERTEX_POINT ( 'NONE', #24662 ) ;
#37543 = CARTESIAN_POINT ( 'NONE',  ( 75.05402655318509630, 2.143131898507880377E-16, -160.9317124430720582 ) ) ;
#37544 = DIRECTION ( 'NONE',  ( -1.000000000000000000, -0.000000000000000000, -0.000000000000000000 ) ) ;
#37545 = CARTESIAN_POINT ( 'NONE',  ( 153.3040265531850537, 1.750000000000009992, 0.8182875569279768335 ) ) ;
#37546 = EDGE_CURVE ( 'NONE', #42631, #44556, #14099, .T. ) ;
#37547 = EDGE_CURVE ( 'NONE', #17736, #26366, #22565, .T. ) ;
#37548 = AXIS2_PLACEMENT_3D ( 'NONE', #12525, #29201, #20235 ) ;
#37549 = CARTESIAN_POINT ( 'NONE',  ( 210.0000000000000568, 0.000000000000000000, -79.18171244307201562 ) ) ;
#37550 = DIRECTION ( 'NONE',  ( -0.000000000000000000, -0.000000000000000000, -1.000000000000000000 ) ) ;
#37551 = FACE_OUTER_BOUND ( 'NONE', #44155, .T. ) ;
#37552 = ORIENTED_EDGE ( 'NONE', *, *, #4482, .T. ) ;
#37553 = DIRECTION ( 'NONE',  ( 1.000000000000000000, 0.000000000000000000, -1.860490536778032451E-50 ) ) ;
#37554 = ADVANCED_FACE ( 'NONE', ( #17456 ), #9748, .T. ) ;
#37555 = CARTESIAN_POINT ( 'NONE',  ( 115.0540265531850395, 2.143131898507847836E-16, -37.43171244307205825 ) ) ;
#37556 = CARTESIAN_POINT ( 'NONE',  ( -1.460157059060481544, 1.483633425177112164, 9.888808121373916293 ) ) ;
#37557 = ADVANCED_FACE ( 'NONE', ( #9499 ), #1814, .T. ) ;
#37558 = ADVANCED_FACE ( 'NONE', ( #2064 ), #44874, .T. ) ;
#37559 = CARTESIAN_POINT ( 'NONE',  ( 166.9999999999999716, -168.9999999999999432, -350.0000000000001705 ) ) ;
#37560 = EDGE_LOOP ( 'NONE', ( #12507, #7967, #10174, #25949 ) ) ;
#37561 = DIRECTION ( 'NONE',  ( 0.000000000000000000, -1.000000000000000000, -0.000000000000000000 ) ) ;
#37562 = ORIENTED_EDGE ( 'NONE', *, *, #2894, .F. ) ;
#37563 = CARTESIAN_POINT ( 'NONE',  ( -225.0000000000000568, 175.0000000000000000, 500.0000000000000000 ) ) ;
#37564 = LINE ( 'NONE', #48284, #27475 ) ;
#37565 = EDGE_CURVE ( 'NONE', #8207, #45606, #49213, .T. ) ;
#37566 = CARTESIAN_POINT ( 'NONE',  ( -208.4459734468149463, 0.000000000000000000, -77.43171244307204404 ) ) ;
#37567 = ORIENTED_EDGE ( 'NONE', *, *, #32201, .T. ) ;
#37568 = ADVANCED_FACE ( 'NONE', ( #41311 ), #21054, .T. ) ;
#37569 = CARTESIAN_POINT ( 'NONE',  ( 1.011271242968694084, -0.7347315653655782652, 10.00000000000000000 ) ) ;
#37570 = EDGE_LOOP ( 'NONE', ( #36306, #29537, #14203, #45284 ) ) ;
#37571 = CARTESIAN_POINT ( 'NONE',  ( 195.0540265531851105, 2.143131898507880377E-16, 159.0682875569279702 ) ) ;
#37572 = DIRECTION ( 'NONE',  ( -0.000000000000000000, -1.000000000000000000, -0.000000000000000000 ) ) ;
#37573 = ORIENTED_EDGE ( 'NONE', *, *, #3061, .F. ) ;
#37574 = ORIENTED_EDGE ( 'NONE', *, *, #35127, .F. ) ;
#37575 = LINE ( 'NONE', #14453, #12784 ) ;
#37576 = DIRECTION ( 'NONE',  ( 0.000000000000000000, 0.000000000000000000, -1.000000000000000000 ) ) ;
#37577 =( BOUNDED_CURVE ( )  B_SPLINE_CURVE ( 3, ( #29693, #45315, #13779, #9437 ),
 .UNSPECIFIED., .F., .F. ) 
 B_SPLINE_CURVE_WITH_KNOTS ( ( 4, 4 ),
 ( 4.712388980384689674, 6.283185307179586232 ),
 .UNSPECIFIED. ) 
 CURVE ( )  GEOMETRIC_REPRESENTATION_ITEM ( )  RATIONAL_B_SPLINE_CURVE ( ( 1.000000000000000000, 0.8047378541243649375, 0.8047378541243649375, 1.000000000000000000 ) ) 
 REPRESENTATION_ITEM ( '' )  );
#37578 = AXIS2_PLACEMENT_3D ( 'NONE', #43702, #35533, #16268 ) ;
#37579 = ORIENTED_EDGE ( 'NONE', *, *, #21460, .T. ) ;
#37580 = EDGE_LOOP ( 'NONE', ( #25145, #31316, #16593, #27403, #38579, #50491, #24206, #50326 ) ) ;
#37581 = DIRECTION ( 'NONE',  ( -1.000000000000000000, 0.000000000000000000, 0.000000000000000000 ) ) ;
#37582 = CARTESIAN_POINT ( 'NONE',  ( -46.69597344681494633, 1.750000000000010658, -119.1817124430720440 ) ) ;
#37583 = PLANE ( 'NONE',  #12470 ) ;
#37584 = ORIENTED_EDGE ( 'NONE', *, *, #5322, .T. ) ;
#37585 = CARTESIAN_POINT ( 'NONE',  ( 2.536646476037169418, 2.794100479408543780, 9.865049507598756762 ) ) ;
#37586 = VERTEX_POINT ( 'NONE', #5143 ) ;
#37587 =( BOUNDED_CURVE ( )  B_SPLINE_CURVE ( 3, ( #13281, #26306, #33062, #6797 ),
 .UNSPECIFIED., .F., .F. ) 
 B_SPLINE_CURVE_WITH_KNOTS ( ( 4, 4 ),
 ( 3.141592653589793116, 4.712388980384689674 ),
 .UNSPECIFIED. ) 
 CURVE ( )  GEOMETRIC_REPRESENTATION_ITEM ( )  RATIONAL_B_SPLINE_CURVE ( ( 1.000000000000000000, 0.8047378541243649375, 0.8047378541243649375, 1.000000000000000000 ) ) 
 REPRESENTATION_ITEM ( '' )  );
#37588 = CARTESIAN_POINT ( 'NONE',  ( 181.0000000000000000, -184.9999999999999716, -344.0000000000001137 ) ) ;
#37589 = FACE_OUTER_BOUND ( 'NONE', #31894, .T. ) ;
#37590 = ORIENTED_EDGE ( 'NONE', *, *, #20285, .F. ) ;
#37591 = EDGE_LOOP ( 'NONE', ( #33329, #41121, #34945, #33032, #3533, #50301 ) ) ;
#37592 = CARTESIAN_POINT ( 'NONE',  ( -47.72109971266203132, -1.750000000000009548, -38.15658617722494483 ) ) ;
#37593 = DIRECTION ( 'NONE',  ( -1.000000000000000000, -0.000000000000000000, -0.000000000000000000 ) ) ;
#37594 = ORIENTED_EDGE ( 'NONE', *, *, #29899, .F. ) ;
#37595 = DIRECTION ( 'NONE',  ( 0.000000000000000000, 0.000000000000000000, 1.000000000000000000 ) ) ;
#37596 = ORIENTED_EDGE ( 'NONE', *, *, #31869, .F. ) ;
#37597 = CARTESIAN_POINT ( 'NONE',  ( -48.44597344681495343, 0.000000000000000000, 165.0000000000000000 ) ) ;
#37598 = ORIENTED_EDGE ( 'NONE', *, *, #10583, .F. ) ;
#37599 = LINE ( 'NONE', #18820, #14560 ) ;
#37600 = CARTESIAN_POINT ( 'NONE',  ( 115.0540265531850395, 2.143131898507847836E-16, -80.93171244307201562 ) ) ;
#37601 = CARTESIAN_POINT ( 'NONE',  ( -128.4459734468149179, 0.000000000000000000, 165.0000000000000000 ) ) ;
#37602 = EDGE_CURVE ( 'NONE', #49709, #21399, #20794, .T. ) ;
#37603 = ADVANCED_FACE ( 'NONE', ( #9255 ), #16961, .T. ) ;
#37604 = CARTESIAN_POINT ( 'NONE',  ( 135.0000000000003411, 17.00000000000000000, -60.00000000000000000 ) ) ;
#37605 = ORIENTED_EDGE ( 'NONE', *, *, #25600, .F. ) ;
#37606 = DIRECTION ( 'NONE',  ( 0.000000000000000000, 0.2981428420003837121, 0.9545212652235329776 ) ) ;
#37607 = DIRECTION ( 'NONE',  ( 0.000000000000000000, 0.000000000000000000, 1.000000000000000000 ) ) ;
#37608 = ADVANCED_FACE ( 'NONE', ( #49717 ), #41562, .F. ) ;
#37609 = CARTESIAN_POINT ( 'NONE',  ( -46.69597344681494633, 1.750000000000010658, -119.1817124430720440 ) ) ;
#37610 = DIRECTION ( 'NONE',  ( 1.000000000000000000, 0.000000000000000000, 0.000000000000000000 ) ) ;
#37611 = EDGE_CURVE ( 'NONE', #24770, #16975, #26171, .T. ) ;
#37612 = CIRCLE ( 'NONE', #7298, 50.00000000000000000 ) ;
#37613 = EDGE_CURVE ( 'NONE', #2601, #27411, #7175, .T. ) ;
#37614 = AXIS2_PLACEMENT_3D ( 'NONE', #28067, #40383, #24480 ) ;
#37615 = CARTESIAN_POINT ( 'NONE',  ( 210.0000000000000568, 0.000000000000000000, 40.81828755692798438 ) ) ;
#37616 = DIRECTION ( 'NONE',  ( -0.000000000000000000, -0.000000000000000000, -1.000000000000000000 ) ) ;
#37617 = EDGE_CURVE ( 'NONE', #1912, #12326, #6268, .T. ) ;
#37618 = DIRECTION ( 'NONE',  ( 0.000000000000000000, 2.969158215481698263E-48, -1.000000000000000000 ) ) ;
#37619 = PLANE ( 'NONE',  #48277 ) ;
#37620 = EDGE_CURVE ( 'NONE', #25767, #15550, #50210, .T. ) ;
#37621 = CLOSED_SHELL ( 'NONE', ( #50261, #41365, #33164, #10496, #9698, #17560, #1795, #47419 ) ) ;
#37622 = CARTESIAN_POINT ( 'NONE',  ( 0.3862712429686978033, -1.188820645368937834, 3.333333333333333481 ) ) ;
#37623 = ORIENTED_EDGE ( 'NONE', *, *, #23723, .T. ) ;
#37624 = CARTESIAN_POINT ( 'NONE',  ( -19.99999999999940670, 17.00000000000000000, -30.00000000000000000 ) ) ;
#37625 = AXIS2_PLACEMENT_3D ( 'NONE', #31114, #3651, #7252 ) ;
#37626 = CARTESIAN_POINT ( 'NONE',  ( -46.75893035013464072, -17.89420872045582200, 3.199614146704519602 ) ) ;
#37627 = CARTESIAN_POINT ( 'NONE',  ( -6.508636631827791064, -15.75743548351446854, 8.953103998512858652 ) ) ;
#37628 = CARTESIAN_POINT ( 'NONE',  ( -14.99999999999876366, 16.00000000000000000, 5.000000000000004441 ) ) ;
#37629 = DIRECTION ( 'NONE',  ( 0.000000000000000000, 0.000000000000000000, 1.000000000000000000 ) ) ;
#37630 = ORIENTED_EDGE ( 'NONE', *, *, #18145, .T. ) ;
#37631 = PRODUCT ( 'MAT-058', 'MAT-058', '', ( #49 ) ) ;
#37632 = ORIENTED_EDGE ( 'NONE', *, *, #17964, .F. ) ;
#37633 = DIRECTION ( 'NONE',  ( -0.000000000000000000, 1.000000000000000000, 0.000000000000000000 ) ) ;
#37634 = FACE_OUTER_BOUND ( 'NONE', #48434, .T. ) ;
#37635 = ORIENTED_EDGE ( 'NONE', *, *, #43073, .F. ) ;
#37636 = DIRECTION ( 'NONE',  ( -0.000000000000000000, 0.000000000000000000, 1.000000000000000000 ) ) ;
#37637 = CARTESIAN_POINT ( 'NONE',  ( 135.0000000000009663, 17.00000000000000000, 0.000000000000000000 ) ) ;
#37638 = ORIENTED_EDGE ( 'NONE', *, *, #49676, .F. ) ;
#37639 = ORIENTED_EDGE ( 'NONE', *, *, #28836, .F. ) ;
#37640 = EDGE_LOOP ( 'NONE', ( #35021, #35849, #45011, #48653 ) ) ;
#37641 = EDGE_CURVE ( 'NONE', #35337, #20217, #3547, .T. ) ;
#37642 = CARTESIAN_POINT ( 'NONE',  ( -87.72109971266203843, -1.750000000000009548, 1.843413822775065825 ) ) ;
#37643 = AXIS2_PLACEMENT_3D ( 'NONE', #5662, #4900, #9512 ) ;
#37644 = DIRECTION ( 'NONE',  ( -1.000000000000000000, -0.000000000000000000, -0.000000000000000000 ) ) ;
#37645 = ORIENTED_EDGE ( 'NONE', *, *, #29143, .T. ) ;
#37646 = AXIS2_PLACEMENT_3D ( 'NONE', #6414, #21307, #9754 ) ;
#37647 = FACE_OUTER_BOUND ( 'NONE', #38822, .T. ) ;
#37648 = DIRECTION ( 'NONE',  ( 0.000000000000000000, 1.000000000000000000, 0.000000000000000000 ) ) ;
#37649 = LINE ( 'NONE', #2477, #41842 ) ;
#37650 = VERTEX_POINT ( 'NONE', #49468 ) ;
#37651 = VERTEX_POINT ( 'NONE', #42060 ) ;
#37652 = DIRECTION ( 'NONE',  ( 0.000000000000000000, 0.000000000000000000, -1.000000000000000000 ) ) ;
#37653 = AXIS2_PLACEMENT_3D ( 'NONE', #25142, #36718, #45104 ) ;
#37654 = CARTESIAN_POINT ( 'NONE',  ( -47.88254548617756967, 14.43607691413558669, -3.760136334089591248 ) ) ;
#37655 = CARTESIAN_POINT ( 'NONE',  ( 210.0000000000000568, 2.143131898507881116E-16, -40.93171244307203693 ) ) ;
#37656 = ORIENTED_EDGE ( 'NONE', *, *, #16440, .T. ) ;
#37657 = CARTESIAN_POINT ( 'NONE',  ( -33.57695195286787282, -16.69845195084869616, 8.914903342594564961 ) ) ;
#37658 = PRESENTATION_STYLE_ASSIGNMENT (( #34055 ) ) ;
#37659 = CIRCLE ( 'NONE', #38464, 2.000000000000001776 ) ;
#37660 = DIRECTION ( 'NONE',  ( 0.000000000000000000, 0.000000000000000000, 1.000000000000000000 ) ) ;
#37661 = DIRECTION ( 'NONE',  ( 0.000000000000000000, 0.000000000000000000, 1.000000000000000000 ) ) ;
#37662 = FACE_OUTER_BOUND ( 'NONE', #5045, .T. ) ;
#37663 = SURFACE_STYLE_FILL_AREA ( #45567 ) ;
#37664 = CARTESIAN_POINT ( 'NONE',  ( 24.39427009665985224, 44.07992421011656603, 8.807470649214879543 ) ) ;
#37665 = CARTESIAN_POINT ( 'NONE',  ( 35.00000000000028422, 16.00000000000000000, -60.00000000000000000 ) ) ;
#37666 = CARTESIAN_POINT ( 'NONE',  ( -64.99999999999877787, 17.00000000000000000, 5.000000000000004441 ) ) ;
#37667 = B_SPLINE_CURVE_WITH_KNOTS ( 'NONE', 3,
 ( #23277, #15848, #39716, #50697 ),
 .UNSPECIFIED., .F., .F.,
 ( 4, 4 ),
 ( 0.000000000000000000, 0.2562577668812813791 ),
 .UNSPECIFIED. ) ;
#37668 = CARTESIAN_POINT ( 'NONE',  ( 0.3862712429686727678, 1.188820645368945605, 10.00000000000000000 ) ) ;
#37669 = DIRECTION ( 'NONE',  ( 0.2130880182788259525, 0.000000000000000000, -0.9770330068457272477 ) ) ;
#37670 = VERTEX_POINT ( 'NONE', #34898 ) ;
#37671 = ADVANCED_FACE ( 'NONE', ( #46392 ), #6817, .T. ) ;
#37672 = LINE ( 'NONE', #18143, #2888 ) ;
#37673 = VECTOR ( 'NONE', #47919, 1000.000000000000000 ) ;
#37674 = CYLINDRICAL_SURFACE ( 'NONE', #12396, 2.000000000000001776 ) ;
#37675 = AXIS2_PLACEMENT_3D ( 'NONE', #35103, #7381, #23008 ) ;
#37676 = ORIENTED_EDGE ( 'NONE', *, *, #45374, .F. ) ;
#37677 = FILL_AREA_STYLE_COLOUR ( '', #37972 ) ;
#37678 = VECTOR ( 'NONE', #36682, 1000.000000000000000 ) ;
#37679 = CARTESIAN_POINT ( 'NONE',  ( 155.0540265531850537, 1.025126265847089657, -37.43171244307202272 ) ) ;
#37680 = ORIENTED_EDGE ( 'NONE', *, *, #5614, .F. ) ;
#37681 = CARTESIAN_POINT ( 'NONE',  ( -19.99999999999971223, 16.00000000000000000, -84.99999999999998579 ) ) ;
#37682 = CARTESIAN_POINT ( 'NONE',  ( -114.9999999999991047, 17.00000000000000000, -24.99999999999999289 ) ) ;
#37683 = AXIS2_PLACEMENT_3D ( 'NONE', #8802, #47994, #28293 ) ;
#37684 = PLANE ( 'NONE',  #16797 ) ;
#37685 = ORIENTED_EDGE ( 'NONE', *, *, #7417, .F. ) ;
#37686 = CARTESIAN_POINT ( 'NONE',  ( 210.0000000000000568, 2.143131898507880377E-16, -0.9317124430720331585 ) ) ;
#37687 = VERTEX_POINT ( 'NONE', #2555 ) ;
#37688 = VERTEX_POINT ( 'NONE', #14361 ) ;
#37689 = CARTESIAN_POINT ( 'NONE',  ( -5.000000000000000000, -175.0000000000000284, -346.2500000000002274 ) ) ;
#37690 = VECTOR ( 'NONE', #27387, 1000.000000000000000 ) ;
#37691 = EDGE_LOOP ( 'NONE', ( #35994, #22066, #22777, #112, #29910, #5371 ) ) ;
#37692 = DIRECTION ( 'NONE',  ( 0.000000000000000000, 0.000000000000000000, 1.000000000000000000 ) ) ;
#37693 = DIRECTION ( 'NONE',  ( -1.000000000000000000, 0.000000000000000000, 0.000000000000000000 ) ) ;
#37694 = CARTESIAN_POINT ( 'NONE',  ( 168.9999999999999716, 175.0000000000000284, -360.0000000000001705 ) ) ;
#37695 = CARTESIAN_POINT ( 'NONE',  ( -46.69597344681494633, -1.750000000000010658, 120.8182875569279702 ) ) ;
#37696 = DIRECTION ( 'NONE',  ( -0.000000000000000000, -0.000000000000000000, 1.000000000000000000 ) ) ;
#37697 = VERTEX_POINT ( 'NONE', #45634 ) ;
#37699 = EDGE_CURVE ( 'NONE', #6656, #26366, #15120, .T. ) ;
#37698 = DIRECTION ( 'NONE',  ( 0.000000000000000000, 0.000000000000000000, -1.000000000000000000 ) ) ;
#37700 = CARTESIAN_POINT ( 'NONE',  ( -165.0000000000000284, 16.00000000000000000, -54.99999999999999289 ) ) ;
#37701 = CARTESIAN_POINT ( 'NONE',  ( 35.00000000000122213, 16.00000000000000000, 5.000000000000004441 ) ) ;
#37702 = ORIENTED_EDGE ( 'NONE', *, *, #6207, .F. ) ;
#37703 = B_SPLINE_CURVE_WITH_KNOTS ( 'NONE', 3,
 ( #39975, #47356, #12496, #28661 ),
 .UNSPECIFIED., .F., .F.,
 ( 4, 4 ),
 ( 0.0002936521407534369954, 0.0006663369986142379710 ),
 .UNSPECIFIED. ) ;
#37704 = CARTESIAN_POINT ( 'NONE',  ( -8.294258456918070621, -5.607426633512162084, 6.185594734181537824 ) ) ;
#37705 = DIRECTION ( 'NONE',  ( 1.000000000000000000, -0.000000000000000000, -0.000000000000000000 ) ) ;
#37706 = ORIENTED_EDGE ( 'NONE', *, *, #39520, .T. ) ;
#37707 = ORIENTED_EDGE ( 'NONE', *, *, #21889, .T. ) ;
#37708 = VERTEX_POINT ( 'NONE', #23063 ) ;
#37709 = CARTESIAN_POINT ( 'NONE',  ( 50.24128791297869867, -41.04536285977715693, -5.000000000000000000 ) ) ;
#37710 = CYLINDRICAL_SURFACE ( 'NONE', #47935, 1.750000000000008438 ) ;
#37711 = ORIENTED_EDGE ( 'NONE', *, *, #20903, .F. ) ;
#37712 = CIRCLE ( 'NONE', #36927, 22.00000000000000000 ) ;
#37713 = VECTOR ( 'NONE', #20065, 1000.000000000000000 ) ;
#37714 = CARTESIAN_POINT ( 'NONE',  ( 33.30402655318503946, -1.750000000000009992, 160.8182875569279702 ) ) ;
#37715 = CARTESIAN_POINT ( 'NONE',  ( -2.569099690548740877, 50.00000000000000711, 3.199614146704519602 ) ) ;
#37716 =( BOUNDED_CURVE ( )  B_SPLINE_CURVE ( 3, ( #45335, #26112, #6877, #6118 ),
 .UNSPECIFIED., .F., .F. ) 
 B_SPLINE_CURVE_WITH_KNOTS ( ( 4, 4 ),
 ( 1.570796326794889675, 3.141592653589793116 ),
 .UNSPECIFIED. ) 
 CURVE ( )  GEOMETRIC_REPRESENTATION_ITEM ( )  RATIONAL_B_SPLINE_CURVE ( ( 1.000000000000000000, 0.8047378541243634942, 0.8047378541243634942, 1.000000000000000000 ) ) 
 REPRESENTATION_ITEM ( '' )  );
#37717 = CARTESIAN_POINT ( 'NONE',  ( -87.72109971266203843, -1.750000000000010214, 119.7931612910808781 ) ) ;
#37718 = AXIS2_PLACEMENT_3D ( 'NONE', #30932, #41697, #21946 ) ;
#37719 = CARTESIAN_POINT ( 'NONE',  ( -4.945973446814903696, 2.143131898507912917E-16, 82.56828755692801280 ) ) ;
#37720 = ORIENTED_EDGE ( 'NONE', *, *, #25238, .T. ) ;
#37721 = CARTESIAN_POINT ( 'NONE',  ( 34.32915281903212446, 1.750000000000009548, -0.2068387089191121020 ) ) ;
#37722 = DIRECTION ( 'NONE',  ( 1.000000000000000000, 0.000000000000000000, 0.000000000000000000 ) ) ;
#37723 = AXIS2_PLACEMENT_3D ( 'NONE', #34292, #23511, #3997 ) ;
#37724 =( BOUNDED_CURVE ( )  B_SPLINE_CURVE ( 3, ( #40487, #1738, #40230, #39736 ),
 .UNSPECIFIED., .F., .F. ) 
 B_SPLINE_CURVE_WITH_KNOTS ( ( 4, 4 ),
 ( 0.000000000000000000, 1.570796326794896558 ),
 .UNSPECIFIED. ) 
 CURVE ( )  GEOMETRIC_REPRESENTATION_ITEM ( )  RATIONAL_B_SPLINE_CURVE ( ( 1.000000000000000000, 0.8047378541243649375, 0.8047378541243649375, 1.000000000000000000 ) ) 
 REPRESENTATION_ITEM ( '' )  );
#37725 = CIRCLE ( 'NONE', #31168, 1.749999999999987566 ) ;
#37726 = LINE ( 'NONE', #42055, #2698 ) ;
#37727 = ORIENTED_EDGE ( 'NONE', *, *, #40714, .F. ) ;
#37728 = ITEM_DEFINED_TRANSFORMATION ( 'NONE', 'NONE', #19249,  #45486 ) ;
#37730 = CARTESIAN_POINT ( 'NONE',  ( 192.2789002873380184, -1.750000000000009548, -40.20683870891912193 ) ) ;
#37729 = AXIS2_PLACEMENT_3D ( 'NONE', #9772, #33646, #25693 ) ;
#37731 = CARTESIAN_POINT ( 'NONE',  ( -119.9999999999978400, 16.00000000000000000, 95.00000000000000000 ) ) ;
#37732 = DIRECTION ( 'NONE',  ( 0.000000000000000000, -2.265761274745217480E-16, 1.000000000000000000 ) ) ;
#37733 = EDGE_LOOP ( 'NONE', ( #31962, #26812, #36772, #31977 ) ) ;
#37734 = CARTESIAN_POINT ( 'NONE',  ( 193.3040265531851105, -1.750000000000010214, 40.81828755692798438 ) ) ;
#37735 = ADVANCED_FACE ( 'NONE', ( #38738 ), #50478, .T. ) ;
#37736 = FACE_OUTER_BOUND ( 'NONE', #50051, .T. ) ;
#37737 =( BOUNDED_CURVE ( )  B_SPLINE_CURVE ( 3, ( #48751, #45163, #20840, #2106 ),
 .UNSPECIFIED., .F., .F. ) 
 B_SPLINE_CURVE_WITH_KNOTS ( ( 4, 4 ),
 ( 4.712388980384689674, 6.283185307179586232 ),
 .UNSPECIFIED. ) 
 CURVE ( )  GEOMETRIC_REPRESENTATION_ITEM ( )  RATIONAL_B_SPLINE_CURVE ( ( 1.000000000000000000, 0.8047378541243649375, 0.8047378541243649375, 1.000000000000000000 ) ) 
 REPRESENTATION_ITEM ( '' )  );
#37738 = LINE ( 'NONE', #21556, #36004 ) ;
#37739 = DIRECTION ( 'NONE',  ( 0.000000000000000000, 0.000000000000000000, 1.000000000000000000 ) ) ;
#37740 = EDGE_CURVE ( 'NONE', #41718, #16324, #30520, .T. ) ;
#37741 = CARTESIAN_POINT ( 'NONE',  ( 112.2789002873379758, 1.749999999999996669, 81.84341382277506227 ) ) ;
#37742 = ORIENTED_EDGE ( 'NONE', *, *, #24341, .T. ) ;
#37743 = CARTESIAN_POINT ( 'NONE',  ( 3.566525152641073504, -1.569997364302916809, 9.741991644047246268 ) ) ;
#37744 = ORIENTED_EDGE ( 'NONE', *, *, #27216, .T. ) ;
#37745 = CARTESIAN_POINT ( 'NONE',  ( 181.0000000000000000, -184.9999999999999716, -356.0000000000001705 ) ) ;
#37746 = EDGE_LOOP ( 'NONE', ( #19239, #36985, #5713, #8556 ) ) ;
#37747 = DIRECTION ( 'NONE',  ( -0.000000000000000000, -1.000000000000000000, -0.000000000000000000 ) ) ;
#37749 = ADVANCED_FACE ( 'NONE', ( #34636 ), #18954, .T. ) ;
#37748 = CARTESIAN_POINT ( 'NONE',  ( -124.9459734468149321, -1.025126265847081664, 162.5682875569279133 ) ) ;
#37750 = EDGE_CURVE ( 'NONE', #11655, #1161, #50199, .T. ) ;
#37751 = ORIENTED_EDGE ( 'NONE', *, *, #28252, .F. ) ;
#37752 = AXIS2_PLACEMENT_3D ( 'NONE', #33582, #14567, #45595 ) ;
#37753 = EDGE_CURVE ( 'NONE', #48199, #7390, #38933, .T. ) ;
#37754 = AXIS2_PLACEMENT_3D ( 'NONE', #34650, #19222, #19480 ) ;
#37755 = CARTESIAN_POINT ( 'NONE',  ( -25.08868538179562435, 27.91927157928049752, 6.057468652304069501 ) ) ;
#37756 = ORIENTED_EDGE ( 'NONE', *, *, #36929, .T. ) ;
#37757 = CARTESIAN_POINT ( 'NONE',  ( 191.5540265531850537, -1.025126265847089657, -80.93171244307201562 ) ) ;
#37758 = PLANE ( 'NONE',  #8510 ) ;
#37759 = CARTESIAN_POINT ( 'NONE',  ( -36.08557433729205144, 35.58569447144795816, 7.455576670931136185 ) ) ;
#37760 = CARTESIAN_POINT ( 'NONE',  ( 167.0000000000000284, 165.0000000000000000, 343.9999999999998863 ) ) ;
#37761 = CARTESIAN_POINT ( 'NONE',  ( 80.00000000000028422, 16.00000000000000000, -60.00000000000000000 ) ) ;
#37762 = VECTOR ( 'NONE', #24011, 1000.000000000000000 ) ;
#37763 = EDGE_LOOP ( 'NONE', ( #17530, #6851, #4373, #12803 ) ) ;
#37765 = ORIENTED_EDGE ( 'NONE', *, *, #10442, .F. ) ;
#37764 = EDGE_CURVE ( 'NONE', #41270, #4446, #26165, .T. ) ;
#37766 = CARTESIAN_POINT ( 'NONE',  ( -0.1287570809895602630, -0.3962735484563142396, 10.00000000000000000 ) ) ;
#37767 = EDGE_CURVE ( 'NONE', #43082, #19505, #37985, .T. ) ;
#37768 = EDGE_CURVE ( 'NONE', #40868, #25327, #20239, .T. ) ;
#37769 = EDGE_CURVE ( 'NONE', #14566, #50334, #38626, .T. ) ;
#37770 = ORIENTED_EDGE ( 'NONE', *, *, #28619, .T. ) ;
#37771 = DIRECTION ( 'NONE',  ( 0.000000000000000000, 0.000000000000000000, -1.000000000000000000 ) ) ;
#37772 = CARTESIAN_POINT ( 'NONE',  ( 31.55402655318503236, 1.025126265847088991, -157.4317124430720582 ) ) ;
#37773 = ORIENTED_EDGE ( 'NONE', *, *, #22749, .T. ) ;
#37774 = CARTESIAN_POINT ( 'NONE',  ( 151.5540265531850537, 0.000000000000000000, -120.9317124430720156 ) ) ;
#37775 = EDGE_CURVE ( 'NONE', #30452, #22310, #43578, .T. ) ;
#37776 = LINE ( 'NONE', #10308, #1360 ) ;
#37777 = ORIENTED_EDGE ( 'NONE', *, *, #24881, .F. ) ;
#37778 = CARTESIAN_POINT ( 'NONE',  ( 194.9999999999999716, 164.9999999999999716, 132.0000000000001137 ) ) ;
#37779 = CARTESIAN_POINT ( 'NONE',  ( -6.695973446814940111, -1.750000000000023315, 160.8182875569279702 ) ) ;
#37780 = FACE_OUTER_BOUND ( 'NONE', #20979, .T. ) ;
#37781 = DIRECTION ( 'NONE',  ( -0.000000000000000000, -0.000000000000000000, -1.000000000000000000 ) ) ;
#37782 = EDGE_LOOP ( 'NONE', ( #29553, #8030, #25072, #37893, #21115 ) ) ;
#37783 = EDGE_LOOP ( 'NONE', ( #33874, #36970, #4291, #28759, #46962, #41428 ) ) ;
#37784 = CARTESIAN_POINT ( 'NONE',  ( 31.28977333267368621, -11.25592690310905652, -2.408242355805840784 ) ) ;
#37785 = CARTESIAN_POINT ( 'NONE',  ( 9.281355226777661116, -3.722424633806168615, 0.000000000000000000 ) ) ;
#37786 = ORIENTED_EDGE ( 'NONE', *, *, #31661, .F. ) ;
#37787 = EDGE_CURVE ( 'NONE', #47273, #12321, #33805, .T. ) ;
#37788 = CARTESIAN_POINT ( 'NONE',  ( 0.1265591857323814795, 1.213367045380162823, 9.963925895596176474 ) ) ;
#37790 = EDGE_LOOP ( 'NONE', ( #38748, #45498, #3195, #21032, #5748, #15999 ) ) ;
#37789 = CIRCLE ( 'NONE', #35349, 2.000000000000001776 ) ;
#37791 = CARTESIAN_POINT ( 'NONE',  ( 5.320787806771834383, -8.466948512617054945, 0.000000000000000000 ) ) ;
#37792 = FACE_OUTER_BOUND ( 'NONE', #5169, .T. ) ;
#37793 = DIRECTION ( 'NONE',  ( 1.000000000000000000, 0.000000000000000000, 0.000000000000000000 ) ) ;
#37794 = VECTOR ( 'NONE', #43655, 1000.000000000000000 ) ;
#37795 = EDGE_CURVE ( 'NONE', #45390, #48932, #12530, .T. ) ;
#37796 = EDGE_CURVE ( 'NONE', #29268, #42490, #14322, .T. ) ;
#37797 = DIRECTION ( 'NONE',  ( -0.000000000000000000, -0.000000000000000000, -1.000000000000000000 ) ) ;
#37798 = CARTESIAN_POINT ( 'NONE',  ( 210.0000000000000568, 0.000000000000000000, 80.81828755692798438 ) ) ;
#37799 = LINE ( 'NONE', #18519, #48531 ) ;
#37800 = ORIENTED_EDGE ( 'NONE', *, *, #43107, .T. ) ;
#37801 = CARTESIAN_POINT ( 'NONE',  ( -8.445973446814976526, 0.000000000000000000, 39.06828755692792754 ) ) ;
#37802 = ADVANCED_FACE ( 'NONE', ( #38996 ), #32052, .T. ) ;
#37804 = VECTOR ( 'NONE', #20179, 1000.000000000000114 ) ;
#37803 = CARTESIAN_POINT ( 'NONE',  ( 135.0000000000009663, 17.00000000000000000, 0.000000000000000000 ) ) ;
#37805 = PLANE ( 'NONE',  #25014 ) ;
#37806 = EDGE_CURVE ( 'NONE', #40331, #32574, #26421, .T. ) ;
#37807 = CARTESIAN_POINT ( 'NONE',  ( -165.3973046169136012, -62.56198943095993315, -17.65743994998275213 ) ) ;
#37808 = B_SPLINE_CURVE_WITH_KNOTS ( 'NONE', 3,
 ( #30944, #27330, #46530, #11423 ),
 .UNSPECIFIED., .F., .F.,
 ( 4, 4 ),
 ( 0.8097120833243713900, 0.9322955464062561148 ),
 .UNSPECIFIED. ) ;
#37809 = ORIENTED_EDGE ( 'NONE', *, *, #35008, .T. ) ;
#37810 = CARTESIAN_POINT ( 'NONE',  ( -33.14391172085785797, -37.72293746533095060, -8.016098858316199838 ) ) ;
#37811 = VERTEX_POINT ( 'NONE', #15887 ) ;
#37812 = CARTESIAN_POINT ( 'NONE',  ( -31.44259251615275019, -38.95901822126145220, -9.367992836599951190 ) ) ;
#37813 = CARTESIAN_POINT ( 'NONE',  ( -14.99999999999812594, 17.00000000000000000, 65.00000000000000000 ) ) ;
#37814 = CARTESIAN_POINT ( 'NONE',  ( -208.4459734468148611, -1.025126265847089879, -77.43171244307200141 ) ) ;
#37815 = ADVANCED_FACE ( 'NONE', ( #9387 ), #40697, .F. ) ;
#37816 = ORIENTED_EDGE ( 'NONE', *, *, #13704, .T. ) ;
#37817 = CARTESIAN_POINT ( 'NONE',  ( 4.999999999999999112, 175.0000000000000284, 353.7500000000001705 ) ) ;
#37818 = ORIENTED_EDGE ( 'NONE', *, *, #26308, .T. ) ;
#37819 = CARTESIAN_POINT ( 'NONE',  ( 168.9999999999999716, -5.999999999999950262, 339.9999999999998295 ) ) ;
#37820 =( BOUNDED_CURVE ( )  B_SPLINE_CURVE ( 3, ( #17444, #47944, #12836, #5129 ),
 .UNSPECIFIED., .F., .F. ) 
 B_SPLINE_CURVE_WITH_KNOTS ( ( 4, 4 ),
 ( 1.570796326794896558, 3.141592653589793116 ),
 .UNSPECIFIED. ) 
 CURVE ( )  GEOMETRIC_REPRESENTATION_ITEM ( )  RATIONAL_B_SPLINE_CURVE ( ( 1.000000000000000000, 0.8047378541243649375, 0.8047378541243649375, 1.000000000000000000 ) ) 
 REPRESENTATION_ITEM ( '' )  );
#37821 = EDGE_CURVE ( 'NONE', #40366, #34859, #15384, .T. ) ;
#37822 = CARTESIAN_POINT ( 'NONE',  ( 7.241383964640743187, 3.469446951953614189E-15, -5.000000000000000000 ) ) ;
#37823 = ORIENTED_EDGE ( 'NONE', *, *, #48630, .F. ) ;
#37824 = ORIENTED_EDGE ( 'NONE', *, *, #32920, .F. ) ;
#37825 = CARTESIAN_POINT ( 'NONE',  ( -175.0000000000000000, 15.00000000000000000, 122.5000000000000142 ) ) ;
#37826 = DIRECTION ( 'NONE',  ( 0.000000000000000000, -1.000000000000000000, 0.000000000000000000 ) ) ;
#37827 = VECTOR ( 'NONE', #36670, 1000.000000000000000 ) ;
#37828 = ADVANCED_FACE ( 'NONE', ( #27434 ), #42813, .T. ) ;
#37829 = EDGE_CURVE ( 'NONE', #49488, #35926, #45281, .T. ) ;
#37830 = EDGE_LOOP ( 'NONE', ( #46802, #8532, #22140, #25761, #30891, #15080, #25882, #31301 ) ) ;
#37831 = ORIENTED_EDGE ( 'NONE', *, *, #43377, .F. ) ;
#37832 = LINE ( 'NONE', #2648, #2010 ) ;
#37833 = FACE_OUTER_BOUND ( 'NONE', #9228, .T. ) ;
#37834 = DIRECTION ( 'NONE',  ( 1.000000000000000000, 0.000000000000000000, 0.000000000000000000 ) ) ;
#37835 = ORIENTED_EDGE ( 'NONE', *, *, #3926, .F. ) ;
#37836 = CARTESIAN_POINT ( 'NONE',  ( -14.99999999999876366, 16.00000000000000000, 5.000000000000004441 ) ) ;
#37837 = EDGE_CURVE ( 'NONE', #6277, #49960, #1362, .T. ) ;
#37838 = ORIENTED_EDGE ( 'NONE', *, *, #47195, .T. ) ;
#37839 = EDGE_CURVE ( 'NONE', #23935, #36821, #8484, .T. ) ;
#37840 = CIRCLE ( 'NONE', #1780, 0.5000000000000004441 ) ;
#37841 = EDGE_CURVE ( 'NONE', #13598, #30589, #8196, .T. ) ;
#37842 = FACE_OUTER_BOUND ( 'NONE', #42274, .T. ) ;
#37843 = DIRECTION ( 'NONE',  ( 1.000000000000000000, 0.000000000000000000, 0.000000000000000000 ) ) ;
#37844 = ORIENTED_EDGE ( 'NONE', *, *, #40998, .F. ) ;
#37845 = ORIENTED_EDGE ( 'NONE', *, *, #32788, .F. ) ;
#37846 = LINE ( 'NONE', #2416, #21859 ) ;
#37847 = CARTESIAN_POINT ( 'NONE',  ( 344.0000000000000568, 165.0000000000000000, -110.0000000000002132 ) ) ;
#37848 = VERTEX_POINT ( 'NONE', #504 ) ;
#37849 = DIRECTION ( 'NONE',  ( 0.000000000000000000, 1.000000000000000000, 0.000000000000000000 ) ) ;
#37850 = EDGE_LOOP ( 'NONE', ( #44598, #12718, #11589, #47617, #5881, #47430 ) ) ;
#37851 = CARTESIAN_POINT ( 'NONE',  ( 191.5540265531851105, 0.000000000000000000, -165.0000000000000000 ) ) ;
#37852 = LINE ( 'NONE', #26287, #48520 ) ;
#37853 = ORIENTED_EDGE ( 'NONE', *, *, #43989, .T. ) ;
#37854 = DIRECTION ( 'NONE',  ( -4.758098676964957447E-16, -1.000000000000000000, 7.143884938411937192E-48 ) ) ;
#37855 = CARTESIAN_POINT ( 'NONE',  ( 168.9999999999999716, -256.4999999999999432, -339.9999999999998863 ) ) ;
#37856 = CARTESIAN_POINT ( 'NONE',  ( 164.9999999999999716, 17.00000000000000000, 65.00000000000000000 ) ) ;
#37857 = CARTESIAN_POINT ( 'NONE',  ( 73.30402655318508209, 1.750000000000010658, 80.81828755692798438 ) ) ;
#37858 = EDGE_CURVE ( 'NONE', #16503, #17104, #16141, .T. ) ;
#37859 = DIRECTION ( 'NONE',  ( -0.000000000000000000, -1.000000000000000000, -0.000000000000000000 ) ) ;
#37860 = ORIENTED_EDGE ( 'NONE', *, *, #29637, .T. ) ;
#37861 = CARTESIAN_POINT ( 'NONE',  ( -23.79193388295331602, -28.98609808354994044, -9.422646554964178023 ) ) ;
#37862 = VECTOR ( 'NONE', #30075, 1000.000000000000000 ) ;
#37863 = CYLINDRICAL_SURFACE ( 'NONE', #30591, 1.749999999999987566 ) ;
#37864 = CARTESIAN_POINT ( 'NONE',  ( -167.7210997126620384, 1.750000000000009326, -158.1565861772249377 ) ) ;
#37865 = CARTESIAN_POINT ( 'NONE',  ( 0.3862712429686810944, 1.188820645368943607, 3.333333333333333481 ) ) ;
#37866 = CARTESIAN_POINT ( 'NONE',  ( -1.455748852897583268, -0.01196569884525386721, 9.938560165450793349 ) ) ;
#37867 = DIRECTION ( 'NONE',  ( -0.000000000000000000, -0.000000000000000000, -1.000000000000000000 ) ) ;
#37868 = AXIS2_PLACEMENT_3D ( 'NONE', #1132, #1382, #627 ) ;
#37869 = DIRECTION ( 'NONE',  ( 0.000000000000000000, 0.000000000000000000, 1.000000000000000000 ) ) ;
#37870 = EDGE_CURVE ( 'NONE', #13622, #45864, #13976, .T. ) ;
#37871 = CARTESIAN_POINT ( 'NONE',  ( 0.000000000000000000, 17.00000000000000000, 0.000000000000000000 ) ) ;
#37872 = LINE ( 'NONE', #29391, #28773 ) ;
#37873 = ORIENTED_EDGE ( 'NONE', *, *, #26864, .T. ) ;
#37874 = FACE_OUTER_BOUND ( 'NONE', #36537, .T. ) ;
#37875 =( BOUNDED_CURVE ( )  B_SPLINE_CURVE ( 3, ( #2271, #17908, #35314, #27338 ),
 .UNSPECIFIED., .F., .F. ) 
 B_SPLINE_CURVE_WITH_KNOTS ( ( 4, 4 ),
 ( 1.570796326794896558, 3.141592653589793116 ),
 .UNSPECIFIED. ) 
 CURVE ( )  GEOMETRIC_REPRESENTATION_ITEM ( )  RATIONAL_B_SPLINE_CURVE ( ( 1.000000000000000000, 0.8047378541243649375, 0.8047378541243649375, 1.000000000000000000 ) ) 
 REPRESENTATION_ITEM ( '' )  );
#37876 = DIRECTION ( 'NONE',  ( 0.000000000000000000, 0.000000000000000000, 1.000000000000000000 ) ) ;
#37877 = CARTESIAN_POINT ( 'NONE',  ( -23.26005729352344176, -44.90397804740339183, 7.906207997025717304 ) ) ;
#37878 = DIRECTION ( 'NONE',  ( 0.000000000000000000, -1.000000000000000000, 0.000000000000000000 ) ) ;
#37879 = DIRECTION ( 'NONE',  ( 0.000000000000000000, 0.000000000000000000, -1.000000000000000000 ) ) ;
#37880 =( BOUNDED_CURVE ( )  B_SPLINE_CURVE ( 3, ( #40086, #36245, #28530, #17479 ),
 .UNSPECIFIED., .F., .F. ) 
 B_SPLINE_CURVE_WITH_KNOTS ( ( 4, 4 ),
 ( 0.000000000000000000, 1.570796326794896780 ),
 .UNSPECIFIED. ) 
 CURVE ( )  GEOMETRIC_REPRESENTATION_ITEM ( )  RATIONAL_B_SPLINE_CURVE ( ( 1.000000000000000000, 0.8047378541243649375, 0.8047378541243649375, 1.000000000000000000 ) ) 
 REPRESENTATION_ITEM ( '' )  );
#37881 = ORIENTED_EDGE ( 'NONE', *, *, #27102, .F. ) ;
#37882 = ORIENTED_EDGE ( 'NONE', *, *, #16776, .T. ) ;
#37883 = PLANE ( 'NONE',  #5382 ) ;
#37884 = DIRECTION ( 'NONE',  ( -0.000000000000000000, -0.000000000000000000, -1.000000000000000000 ) ) ;
#37885 = EDGE_CURVE ( 'NONE', #48228, #23523, #33504, .T. ) ;
#37886 = EDGE_CURVE ( 'NONE', #15688, #48233, #6544, .T. ) ;
#37887 = EDGE_LOOP ( 'NONE', ( #34160, #36696, #42326, #1166 ) ) ;
#37888 = CARTESIAN_POINT ( 'NONE',  ( 168.9999999999999716, -272.5000000000000000, -114.9999999999999005 ) ) ;
#37889 = CARTESIAN_POINT ( 'NONE',  ( -208.4459734468149463, 0.000000000000000000, -117.4317124430720725 ) ) ;
#37890 = ORIENTED_EDGE ( 'NONE', *, *, #19543, .T. ) ;
#37891 = ORIENTED_EDGE ( 'NONE', *, *, #40983, .F. ) ;
#37892 = VECTOR ( 'NONE', #41793, 1000.000000000000000 ) ;
#37893 = ORIENTED_EDGE ( 'NONE', *, *, #12367, .F. ) ;
#37894 = EDGE_CURVE ( 'NONE', #12217, #6697, #3144, .T. ) ;
#37895 = ADVANCED_FACE ( 'NONE', ( #45757 ), #14228, .T. ) ;
#37896 = PRESENTATION_LAYER_ASSIGNMENT (  '', '', ( #11662 ) ) ;
#37898 = EDGE_CURVE ( 'NONE', #9479, #47807, #42847, .T. ) ;
#37897 = PLANE ( 'NONE',  #17609 ) ;
#37899 = CARTESIAN_POINT ( 'NONE',  ( 49.46074318306830975, -9.578883844006833570, 8.807470649214879543 ) ) ;
#37900 = EDGE_CURVE ( 'NONE', #46025, #26544, #1692, .T. ) ;
#37901 = CARTESIAN_POINT ( 'NONE',  ( -0.09523839817533703844, -1.466467394240187350, 9.958264684458541183 ) ) ;
#37902 = ORIENTED_EDGE ( 'NONE', *, *, #18925, .T. ) ;
#37903 = CARTESIAN_POINT ( 'NONE',  ( -206.6959734468149463, -1.750000000000010658, 80.81828755692798438 ) ) ;
#37904 = VECTOR ( 'NONE', #44847, 1000.000000000000000 ) ;
#37905 = PLANE ( 'NONE',  #26343 ) ;
#37906 = DIRECTION ( 'NONE',  ( -0.000000000000000000, -0.000000000000000000, -1.000000000000000000 ) ) ;
#37907 = EDGE_LOOP ( 'NONE', ( #47896, #42913, #43008, #2183 ) ) ;
#37908 = ORIENTED_EDGE ( 'NONE', *, *, #10848, .F. ) ;
#37909 = LINE ( 'NONE', #2725, #27049 ) ;
#37910 = CARTESIAN_POINT ( 'NONE',  ( -0.3862712429686895876, 1.188820645368940720, 10.00000000000000000 ) ) ;
#37911 = EDGE_CURVE ( 'NONE', #26328, #76, #17792, .T. ) ;
#37912 = VERTEX_POINT ( 'NONE', #33260 ) ;
#37913 = CARTESIAN_POINT ( 'NONE',  ( 192.2789002873380184, 1.750000000000009548, 41.84341382277508359 ) ) ;
#37914 = SURFACE_SIDE_STYLE ('',( #2485 ) ) ;
#37915 = CARTESIAN_POINT ( 'NONE',  ( 339.9999999999998863, -185.0000000000001421, -349.9999999999998863 ) ) ;
#37916 = FACE_OUTER_BOUND ( 'NONE', #20563, .T. ) ;
#37917 = CARTESIAN_POINT ( 'NONE',  ( 340.0000000000000568, 181.0000000000000284, 339.9999999999997726 ) ) ;
#37918 = EDGE_LOOP ( 'NONE', ( #20343, #2338, #38039, #37282, #42885, #29238 ) ) ;
#37919 = DIRECTION ( 'NONE',  ( 0.000000000000000000, -1.000000000000000000, 0.000000000000000000 ) ) ;
#37920 = DIRECTION ( 'NONE',  ( 0.000000000000000000, 0.000000000000000000, 1.000000000000000000 ) ) ;
#37921 = VECTOR ( 'NONE', #49683, 1000.000000000000000 ) ;
#37922 = CARTESIAN_POINT ( 'NONE',  ( -0.1265591857321690383, -1.213367045380180809, 9.963925895596192461 ) ) ;
#37923 = DIRECTION ( 'NONE',  ( 0.000000000000000000, -0.000000000000000000, -1.000000000000000000 ) ) ;
#37924 = CARTESIAN_POINT ( 'NONE',  ( -27.33593271309441519, 41.94268121623345991, -9.367992836599954742 ) ) ;
#37925 = CARTESIAN_POINT ( 'NONE',  ( -124.9459734468149463, 2.143131898507847836E-16, -120.9317124430720156 ) ) ;
#37926 = VECTOR ( 'NONE', #39313, 1000.000000000000000 ) ;
#37927 = ORIENTED_EDGE ( 'NONE', *, *, #36206, .F. ) ;
#37928 = DIRECTION ( 'NONE',  ( 0.000000000000000000, 0.000000000000000000, 1.000000000000000000 ) ) ;
#37929 = AXIS2_PLACEMENT_3D ( 'NONE', #40055, #301, #4880 ) ;
#37930 = CARTESIAN_POINT ( 'NONE',  ( 71.55402655318505367, 0.000000000000000000, -117.4317124430720156 ) ) ;
#37931 = CARTESIAN_POINT ( 'NONE',  ( 0.2778388845795309314, -1.251314014313100520, 9.976582533991681601 ) ) ;
#37933 = EDGE_CURVE ( 'NONE', #47156, #44725, #2444, .T. ) ;
#37932 = AXIS2_PLACEMENT_3D ( 'NONE', #28203, #23852, #27445 ) ;
#37934 = ORIENTED_EDGE ( 'NONE', *, *, #7078, .T. ) ;
#37935 = CARTESIAN_POINT ( 'NONE',  ( -168.4459734468149463, 0.000000000000000000, 119.0682875569279702 ) ) ;
#37936 = AXIS2_PLACEMENT_3D ( 'NONE', #6377, #42032, #37458 ) ;
#37937 = FACE_OUTER_BOUND ( 'NONE', #802, .T. ) ;
#37938 = ORIENTED_EDGE ( 'NONE', *, *, #25555, .T. ) ;
#37939 = DIRECTION ( 'NONE',  ( -0.000000000000000000, 0.000000000000000000, 1.000000000000000000 ) ) ;
#37940 = FACE_OUTER_BOUND ( 'NONE', #37943, .T. ) ;
#37941 = DIRECTION ( 'NONE',  ( 0.000000000000000000, 0.000000000000000000, -1.000000000000000000 ) ) ;
#37942 = CARTESIAN_POINT ( 'NONE',  ( 210.0000000000000568, 0.000000000000000000, 40.81828755692798438 ) ) ;
#37943 = EDGE_LOOP ( 'NONE', ( #7711, #47549, #31694, #13794 ) ) ;
#37944 = B_SPLINE_SURFACE_WITH_KNOTS ( 'NONE', 3, 3, ( 
 ( #7518, #23153, #38830, #28280 ),
 ( #29034, #40585, #5172, #28782 ),
 ( #40088, #20575, #16229, #12874 ),
 ( #21074, #36759, #12363, #4682 ) ),
 .UNSPECIFIED., .F., .F., .F.,
 ( 4, 4 ),
 ( 4, 4 ),
 ( 0.000000000000000000, 1.000000000000000000 ),
 ( 0.000000000000000000, 1.000000000000000000 ),
 .UNSPECIFIED. ) ;
#37945 = ORIENTED_EDGE ( 'NONE', *, *, #21525, .F. ) ;
#37946 = ORIENTED_EDGE ( 'NONE', *, *, #4805, .T. ) ;
#37947 = CARTESIAN_POINT ( 'NONE',  ( 181.0000000000000568, -164.9999999999999432, 339.9999999999997726 ) ) ;
#37948 = EDGE_CURVE ( 'NONE', #12326, #26155, #9252, .T. ) ;
#37949 = VERTEX_POINT ( 'NONE', #33756 ) ;
#37950 = CARTESIAN_POINT ( 'NONE',  ( 168.9999999999999716, -5.999999999999950262, -350.0000000000001705 ) ) ;
#37951 = CARTESIAN_POINT ( 'NONE',  ( 355.9999999999999432, -185.0000000000001421, -360.0000000000003411 ) ) ;
#37952 = CARTESIAN_POINT ( 'NONE',  ( 357.9999999999999432, 181.0000000000002558, -356.0000000000003411 ) ) ;
#37953 = DIRECTION ( 'NONE',  ( -0.5877852522924625900, -0.8090169943749551118, 0.000000000000000000 ) ) ;
#37954 = DIRECTION ( 'NONE',  ( -1.000000000000000000, 0.000000000000000000, 0.000000000000000000 ) ) ;
#37955 = EDGE_LOOP ( 'NONE', ( #22356, #37426, #43253, #12351, #41570, #37278 ) ) ;
#37956 = DIRECTION ( 'NONE',  ( -0.000000000000000000, -1.000000000000000000, -0.000000000000000000 ) ) ;
#37958 = ADVANCED_FACE ( 'NONE', ( #41690 ), #2686, .T. ) ;
#37957 = CYLINDRICAL_SURFACE ( 'NONE', #1256, 2.000000000000001776 ) ;
#37959 = ADVANCED_FACE ( 'NONE', ( #6795 ), #9885, .T. ) ;
#37960 = DIRECTION ( 'NONE',  ( 0.000000000000000000, 0.000000000000000000, 1.000000000000000000 ) ) ;
#37961 = ORIENTED_EDGE ( 'NONE', *, *, #27406, .T. ) ;
#37962 = FACE_OUTER_BOUND ( 'NONE', #20823, .T. ) ;
#37963 = DIRECTION ( 'NONE',  ( 1.000000000000000000, 0.000000000000000000, 0.000000000000000000 ) ) ;
#37964 = AXIS2_PLACEMENT_3D ( 'NONE', #41014, #33327, #17159 ) ;
#37965 = VERTEX_POINT ( 'NONE', #14492 ) ;
#37966 = ORIENTED_EDGE ( 'NONE', *, *, #24902, .F. ) ;
#37967 = ORIENTED_EDGE ( 'NONE', *, *, #47434, .T. ) ;
#37968 = CARTESIAN_POINT ( 'NONE',  ( 344.0000000000000000, 165.0000000000000000, -106.0000000000001990 ) ) ;
#37969 = ADVANCED_FACE ( 'NONE', ( #30147 ), #48843, .T. ) ;
#37970 = LINE ( 'NONE', #14337, #48735 ) ;
#37971 = ORIENTED_EDGE ( 'NONE', *, *, #4534, .F. ) ;
#37972 = COLOUR_RGB ( '',0.7921568627450980005, 0.8196078431372548767, 0.9333333333333333481 ) ;
#37973 = CARTESIAN_POINT ( 'NONE',  ( -4.763548243873389154, 16.57409059453848599, 8.727788335465566760 ) ) ;
#37974 = DIRECTION ( 'NONE',  ( 0.000000000000000000, 0.000000000000000000, 1.000000000000000000 ) ) ;
#37975 = LINE ( 'NONE', #2791, #27224 ) ;
#37976 = CARTESIAN_POINT ( 'NONE',  ( 115.0540265531850395, 1.025126265847081886, 119.0682875569279702 ) ) ;
#37977 = AXIS2_PLACEMENT_3D ( 'NONE', #30272, #18197, #38246 ) ;
#37978 = ORIENTED_EDGE ( 'NONE', *, *, #4229, .T. ) ;
#37979 = LINE ( 'NONE', #2053, #49838 ) ;
#37980 = SURFACE_STYLE_USAGE ( .BOTH. , #34888 ) ;
#37981 = DIRECTION ( 'NONE',  ( -0.000000000000000000, -1.000000000000000000, -0.000000000000000000 ) ) ;
#37982 = ORIENTED_EDGE ( 'NONE', *, *, #16414, .T. ) ;
#37983 = CARTESIAN_POINT ( 'NONE',  ( 181.0000000000000000, -272.5000000000000000, -114.9999999999999147 ) ) ;
#37984 = CARTESIAN_POINT ( 'NONE',  ( -164.9999999999990905, 17.00000000000000000, -24.99999999999999289 ) ) ;
#37985 = LINE ( 'NONE', #12281, #48567 ) ;
#37986 = EDGE_LOOP ( 'NONE', ( #33468, #35476, #31396, #4096 ) ) ;
#37987 = CARTESIAN_POINT ( 'NONE',  ( 339.9999999999998863, -180.9999999999999716, 343.9999999999997726 ) ) ;
#37988 = FACE_OUTER_BOUND ( 'NONE', #33950, .T. ) ;
#37989 = LINE ( 'NONE', #3830, #44132 ) ;
#37990 = CARTESIAN_POINT ( 'NONE',  ( 71.55402655318505367, 1.025126265847089213, 162.5682875569279133 ) ) ;
#37991 = CARTESIAN_POINT ( 'NONE',  ( -88.44597344681491791, 0.000000000000000000, 162.5682875569279702 ) ) ;
#37992 = ADVANCED_FACE ( 'NONE', ( #37113, #13732 ), #29387, .F. ) ;
#37993 = EDGE_LOOP ( 'NONE', ( #42382, #10386 ) ) ;
#37994 = CARTESIAN_POINT ( 'NONE',  ( 80.00000000000153477, 17.00000000000000000, 35.00000000000000000 ) ) ;
#37995 = VERTEX_POINT ( 'NONE', #17835 ) ;
#37996 = DIRECTION ( 'NONE',  ( 0.000000000000000000, 0.000000000000000000, 1.000000000000000000 ) ) ;
#37997 = AXIS2_PLACEMENT_3D ( 'NONE', #20574, #28279, #35234 ) ;
#37998 = ORIENTED_EDGE ( 'NONE', *, *, #15135, .T. ) ;
#37999 = VECTOR ( 'NONE', #33500, 1000.000000000000000 ) ;
#38000 = CARTESIAN_POINT ( 'NONE',  ( -1.011271242968683204, -0.7347315653655928092, 9.972675548442467175 ) ) ;
#38001 = ORIENTED_EDGE ( 'NONE', *, *, #44981, .F. ) ;
#38002 = CARTESIAN_POINT ( 'NONE',  ( 210.0000000000000568, 2.143131898507881116E-16, 39.06828755692797728 ) ) ;
#38003 = ORIENTED_EDGE ( 'NONE', *, *, #43450, .F. ) ;
#38004 = VECTOR ( 'NONE', #35171, 1000.000000000000000 ) ;
#38005 = ORIENTED_EDGE ( 'NONE', *, *, #12723, .F. ) ;
#38006 = CARTESIAN_POINT ( 'NONE',  ( 191.5540265531851105, 0.000000000000000000, -80.93171244307201562 ) ) ;
#38007 = DIRECTION ( 'NONE',  ( 0.000000000000000000, 0.000000000000000000, -1.000000000000000000 ) ) ;
#38008 = B_SPLINE_CURVE_WITH_KNOTS ( 'NONE', 3,
 ( #45743, #45996, #38356, #45244 ),
 .UNSPECIFIED., .F., .F.,
 ( 4, 4 ),
 ( 0.001937412222931627270, 0.003978261222106111578 ),
 .UNSPECIFIED. ) ;
#38009 = DIRECTION ( 'NONE',  ( 0.000000000000000000, -0.8962124318248270161, 0.4436251537532894806 ) ) ;
#38010 = CARTESIAN_POINT ( 'NONE',  ( -88.44597344681494633, -1.025126265847089879, -117.4317124430720156 ) ) ;
#38011 = CARTESIAN_POINT ( 'NONE',  ( -20.21530556545279111, 31.58467066308232063, -9.422646554964174470 ) ) ;
#38012 = EDGE_LOOP ( 'NONE', ( #43229, #47488, #44198, #26335 ) ) ;
#38013 = ORIENTED_EDGE ( 'NONE', *, *, #50683, .F. ) ;
#38014 = CARTESIAN_POINT ( 'NONE',  ( -33.86622497129646092, 3.037805405905158462, 7.906207997025717304 ) ) ;
#38015 =( BOUNDED_CURVE ( )  B_SPLINE_CURVE ( 3, ( #8984, #40289, #8744, #16426 ),
 .UNSPECIFIED., .F., .F. ) 
 B_SPLINE_CURVE_WITH_KNOTS ( ( 4, 4 ),
 ( 1.570796326794896558, 3.141592653589793116 ),
 .UNSPECIFIED. ) 
 CURVE ( )  GEOMETRIC_REPRESENTATION_ITEM ( )  RATIONAL_B_SPLINE_CURVE ( ( 1.000000000000000000, 0.8047378541243649375, 0.8047378541243649375, 1.000000000000000000 ) ) 
 REPRESENTATION_ITEM ( '' )  );
#38016 = VECTOR ( 'NONE', #48009, 1000.000000000000000 ) ;
#38017 = ORIENTED_EDGE ( 'NONE', *, *, #539, .F. ) ;
#38018 = FACE_OUTER_BOUND ( 'NONE', #37285, .T. ) ;
#38019 = DIRECTION ( 'NONE',  ( -1.586032892321652236E-16, -1.000000000000000000, -6.853681917100419162E-49 ) ) ;
#38020 = VERTEX_POINT ( 'NONE', #29638 ) ;
#38021 = CARTESIAN_POINT ( 'NONE',  ( 8.277096487746778308, -50.00000000000000000, 7.455576670931136185 ) ) ;
#38022 = EDGE_CURVE ( 'NONE', #42571, #43608, #10136, .T. ) ;
#38023 =( BOUNDED_CURVE ( )  B_SPLINE_CURVE ( 3, ( #45059, #42249, #41744, #18384 ),
 .UNSPECIFIED., .F., .F. ) 
 B_SPLINE_CURVE_WITH_KNOTS ( ( 4, 4 ),
 ( 1.570796326794896558, 3.141592653589793116 ),
 .UNSPECIFIED. ) 
 CURVE ( )  GEOMETRIC_REPRESENTATION_ITEM ( )  RATIONAL_B_SPLINE_CURVE ( ( 1.000000000000000000, 0.8047378541243649375, 0.8047378541243649375, 1.000000000000000000 ) ) 
 REPRESENTATION_ITEM ( '' )  );
#38024 = CYLINDRICAL_SURFACE ( 'NONE', #21017, 1.750000000000001554 ) ;
#38025 = VERTEX_POINT ( 'NONE', #50610 ) ;
#38026 = CARTESIAN_POINT ( 'NONE',  ( 34.95136153415558056, -36.40974830873469870, 8.356839323120299312 ) ) ;
#38027 = DIRECTION ( 'NONE',  ( -0.000000000000000000, -1.000000000000000000, -0.000000000000000000 ) ) ;
#38028 = CARTESIAN_POINT ( 'NONE',  ( -42.51732812238060433, -47.49695244670218841, -5.000000000000000000 ) ) ;
#38029 = VECTOR ( 'NONE', #1779, 1000.000000000000000 ) ;
#38030 = VERTEX_POINT ( 'NONE', #42946 ) ;
#38031 = AXIS2_PLACEMENT_3D ( 'NONE', #5811, #48864, #21204 ) ;
#38032 = ORIENTED_EDGE ( 'NONE', *, *, #36278, .F. ) ;
#38033 = FILL_AREA_STYLE ('',( #30837 ) ) ;
#38034 = VECTOR ( 'NONE', #37843, 1000.000000000000000 ) ;
#38035 =( BOUNDED_CURVE ( )  B_SPLINE_CURVE ( 3, ( #48628, #28925, #21471, #16620 ),
 .UNSPECIFIED., .F., .F. ) 
 B_SPLINE_CURVE_WITH_KNOTS ( ( 4, 4 ),
 ( 4.712388980384689674, 6.283185307179586232 ),
 .UNSPECIFIED. ) 
 CURVE ( )  GEOMETRIC_REPRESENTATION_ITEM ( )  RATIONAL_B_SPLINE_CURVE ( ( 1.000000000000000000, 0.8047378541243649375, 0.8047378541243649375, 1.000000000000000000 ) ) 
 REPRESENTATION_ITEM ( '' )  );
#38036 = CARTESIAN_POINT ( 'NONE',  ( 181.0000000000000000, -174.9999999999999716, -340.0000000000001137 ) ) ;
#38037 = ORIENTED_EDGE ( 'NONE', *, *, #41003, .F. ) ;
#38038 = AXIS2_PLACEMENT_3D ( 'NONE', #12982, #9651, #17348 ) ;
#38039 = ORIENTED_EDGE ( 'NONE', *, *, #43521, .F. ) ;
#38040 = CARTESIAN_POINT ( 'NONE',  ( 717.1787655628115772, 792.7343818612995392, 1344.137589624066550 ) ) ;
#38041 = CARTESIAN_POINT ( 'NONE',  ( -3.087186397306470820, -2.514307945609864259, -2.642742795433417058E-16 ) ) ;
#38042 = CARTESIAN_POINT ( 'NONE',  ( 30.00000000000062172, 17.00000000000000000, -54.99999999999999289 ) ) ;
#38043 = DIRECTION ( 'NONE',  ( -0.000000000000000000, -0.000000000000000000, -1.000000000000000000 ) ) ;
#38044 = DIRECTION ( 'NONE',  ( 0.1191452206184309970, 0.000000000000000000, -0.9928768384869220975 ) ) ;
#38045 = ORIENTED_EDGE ( 'NONE', *, *, #23979, .F. ) ;
#38046 = CARTESIAN_POINT ( 'NONE',  ( 73.30402655318508209, -1.750000000000010214, 40.81828755692798438 ) ) ;
#38047 = B_SPLINE_SURFACE_WITH_KNOTS ( 'NONE', 3, 3, ( 
 ( #788, #47683, #8747, #33114 ),
 ( #36725, #20779, #17191, #44365 ),
 ( #12572, #40793, #24402, #36202 ),
 ( #32348, #32861, #40048, #1041 ) ),
 .UNSPECIFIED., .F., .F., .F.,
 ( 4, 4 ),
 ( 4, 4 ),
 ( 0.000000000000000000, 1.000000000000000000 ),
 ( 0.000000000000000000, 1.000000000000000000 ),
 .UNSPECIFIED. ) ;
#38048 = CARTESIAN_POINT ( 'NONE',  ( -47.88254548617756967, 14.43607691413558669, -3.760136334089591248 ) ) ;
#38049 = LINE ( 'NONE', #6985, #47076 ) ;
#38050 = ADVANCED_FACE ( 'NONE', ( #38114 ), #42439, .F. ) ;
#38051 = ADVANCED_FACE ( 'NONE', ( #27054 ), #11000, .T. ) ;
#38052 = B_SPLINE_CURVE_WITH_KNOTS ( 'NONE', 3,
 ( #5594, #16645, #16394, #27950 ),
 .UNSPECIFIED., .F., .F.,
 ( 4, 4 ),
 ( 1.735570302229820823E-18, 2.647279941188451471E-05 ),
 .UNSPECIFIED. ) ;
#38053 = AXIS2_PLACEMENT_3D ( 'NONE', #6221, #45427, #41364 ) ;
#38054 = PRESENTATION_STYLE_ASSIGNMENT (( #22378 ) ) ;
#38055 = VERTEX_POINT ( 'NONE', #46760 ) ;
#38056 = CARTESIAN_POINT ( 'NONE',  ( 154.1026953830863420, -98.56198943095992604, -17.65743994998277699 ) ) ;
#38057 = ORIENTED_EDGE ( 'NONE', *, *, #11198, .F. ) ;
#38058 = DIRECTION ( 'NONE',  ( -0.000000000000000000, -0.000000000000000000, -1.000000000000000000 ) ) ;
#38059 = DIRECTION ( 'NONE',  ( 1.000000000000000000, -1.586032997072805650E-16, -4.759647537211363479E-16 ) ) ;
#38060 = LINE ( 'NONE', #21377, #22251 ) ;
#38061 = VERTEX_POINT ( 'NONE', #23472 ) ;
#38062 = CARTESIAN_POINT ( 'NONE',  ( -4.945973446814903696, 2.143131898507912917E-16, 165.0000000000000000 ) ) ;
#38063 = ORIENTED_EDGE ( 'NONE', *, *, #25263, .F. ) ;
#38064 = CARTESIAN_POINT ( 'NONE',  ( 44.99506233596247995, 23.32283626942318833, 7.455576670931136185 ) ) ;
#38065 = VECTOR ( 'NONE', #34226, 1000.000000000000000 ) ;
#38066 = LINE ( 'NONE', #41897, #49880 ) ;
#38067 = CARTESIAN_POINT ( 'NONE',  ( 0.000000000000000000, 167.0000000000000000, 343.9999999999997726 ) ) ;
#38068 = AXIS2_PLACEMENT_3D ( 'NONE', #18530, #45958, #3648 ) ;
#38069 = ORIENTED_EDGE ( 'NONE', *, *, #41930, .T. ) ;
#38070 = VERTEX_POINT ( 'NONE', #39134 ) ;
#38071 = DIRECTION ( 'NONE',  ( 1.000000000000000000, 0.000000000000000000, 0.000000000000000000 ) ) ;
#38072 = VECTOR ( 'NONE', #16436, 1000.000000000000000 ) ;
#38073 = CARTESIAN_POINT ( 'NONE',  ( 0.4430829022285069918, 1.527139474549929155, 9.933337522700155020 ) ) ;
#38074 = EDGE_CURVE ( 'NONE', #26042, #9263, #19604, .T. ) ;
#38075 = VERTEX_POINT ( 'NONE', #34258 ) ;
#38076 = EDGE_CURVE ( 'NONE', #9583, #15483, #46514, .T. ) ;
#38077 = ORIENTED_EDGE ( 'NONE', *, *, #9520, .T. ) ;
#38078 = CARTESIAN_POINT ( 'NONE',  ( 4.353119224256710496, 9.002796955358187247, 0.000000000000000000 ) ) ;
#38079 = DIRECTION ( 'NONE',  ( 0.000000000000000000, -2.537652627714643577E-15, -1.000000000000000000 ) ) ;
#38080 = CARTESIAN_POINT ( 'NONE',  ( -14.49999999999999822, 12.98684210526315930, -19.37312575500900280 ) ) ;
#38081 = ORIENTED_EDGE ( 'NONE', *, *, #12171, .F. ) ;
#38082 = CARTESIAN_POINT ( 'NONE',  ( 135.0000000000009663, 17.00000000000000000, 0.000000000000000000 ) ) ;
#38083 = EDGE_CURVE ( 'NONE', #12843, #19018, #35289, .T. ) ;
#38084 = ORIENTED_EDGE ( 'NONE', *, *, #17063, .F. ) ;
#38085 = EDGE_CURVE ( 'NONE', #43697, #20947, #3440, .T. ) ;
#38086 = CARTESIAN_POINT ( 'NONE',  ( -50.00000000000000000, 50.00000000000000000, 900.0000000000000000 ) ) ;
#38087 = LINE ( 'NONE', #19064, #10761 ) ;
#38088 = AXIS2_PLACEMENT_3D ( 'NONE', #36544, #1380, #21113 ) ;
#38089 = ORIENTED_EDGE ( 'NONE', *, *, #12037, .T. ) ;
#38090 = VERTEX_POINT ( 'NONE', #125 ) ;
#38091 = ORIENTED_EDGE ( 'NONE', *, *, #50390, .T. ) ;
#38092 = DIRECTION ( 'NONE',  ( 0.000000000000000000, -1.000000000000000000, -1.544785076050074834E-48 ) ) ;
#38093 = CYLINDRICAL_SURFACE ( 'NONE', #1961, 2.000000000000001776 ) ;
#38094 = ORIENTED_EDGE ( 'NONE', *, *, #28505, .T. ) ;
#38095 = CARTESIAN_POINT ( 'NONE',  ( -0.9599924130074112272, 0.8495346730527952861, 9.948547179989619238 ) ) ;
#38096 = VERTEX_POINT ( 'NONE', #47019 ) ;
#38097 = DIRECTION ( 'NONE',  ( -0.000000000000000000, -0.000000000000000000, -1.000000000000000000 ) ) ;
#38098 = FACE_OUTER_BOUND ( 'NONE', #13293, .T. ) ;
#38099 = EDGE_LOOP ( 'NONE', ( #26071, #864, #39291, #36365, #31722, #43557 ) ) ;
#38100 = PLANE ( 'NONE',  #43865 ) ;
#38101 = FACE_OUTER_BOUND ( 'NONE', #27248, .T. ) ;
#38102 = CARTESIAN_POINT ( 'NONE',  ( -47.88254548617756967, 14.43607691413558669, -3.760136334089591248 ) ) ;
#38103 = PLANE ( 'NONE',  #30223 ) ;
#38104 = AXIS2_PLACEMENT_3D ( 'NONE', #31521, #47358, #31265 ) ;
#38105 = ORIENTED_EDGE ( 'NONE', *, *, #11103, .F. ) ;
#38106 = CARTESIAN_POINT ( 'NONE',  ( 432.7825420346616170, 112.5000000000000000, -10.00000000000000178 ) ) ;
#38107 = CARTESIAN_POINT ( 'NONE',  ( 210.0000000000000568, 0.000000000000000000, -119.1817124430720440 ) ) ;
#38108 = LINE ( 'NONE', #17831, #1524 ) ;
#38109 = ADVANCED_FACE ( 'NONE', ( #11923 ), #38367, .T. ) ;
#38110 = ADVANCED_FACE ( 'NONE', ( #15268 ), #3706, .F. ) ;
#38111 = AXIS2_PLACEMENT_3D ( 'NONE', #24085, #20223, #724 ) ;
#38112 = EDGE_CURVE ( 'NONE', #9583, #35891, #38877, .T. ) ;
#38113 = EDGE_CURVE ( 'NONE', #13420, #23604, #7300, .T. ) ;
#38114 = FACE_OUTER_BOUND ( 'NONE', #33248, .T. ) ;
#38115 =( BOUNDED_CURVE ( )  B_SPLINE_CURVE ( 3, ( #30633, #33977, #49564, #38343 ),
 .UNSPECIFIED., .F., .F. ) 
 B_SPLINE_CURVE_WITH_KNOTS ( ( 4, 4 ),
 ( 0.000000000000000000, 1.570796326794896558 ),
 .UNSPECIFIED. ) 
 CURVE ( )  GEOMETRIC_REPRESENTATION_ITEM ( )  RATIONAL_B_SPLINE_CURVE ( ( 1.000000000000000000, 0.8047378541243649375, 0.8047378541243649375, 1.000000000000000000 ) ) 
 REPRESENTATION_ITEM ( '' )  );
#38116 = CARTESIAN_POINT ( 'NONE',  ( 113.3040265531850537, -1.749999999999996891, 0.8182875569279768335 ) ) ;
#38117 = EDGE_CURVE ( 'NONE', #43972, #32354, #20248, .T. ) ;
#38118 = PLANE ( 'NONE',  #6563 ) ;
#38119 = EDGE_CURVE ( 'NONE', #42669, #41952, #38622, .T. ) ;
#38120 = CARTESIAN_POINT ( 'NONE',  ( 224.9999999999999716, -164.9999999999999716, 444.9999999999998295 ) ) ;
#38121 = VERTEX_POINT ( 'NONE', #5222 ) ;
#38122 = CARTESIAN_POINT ( 'NONE',  ( 12.16428377685533313, 11.73151505502934810, -9.008049429158102583 ) ) ;
#38123 = VECTOR ( 'NONE', #34268, 1000.000000000000000 ) ;
#38124 = PLANE ( 'NONE',  #26 ) ;
#38125 = MANIFOLD_SOLID_BREP ( 'Square tube 20 X 20 X 2(1)[5]', #6458 ) ;
#38126 = APPLICATION_CONTEXT ( 'automotive_design' ) ;
#38127 = VECTOR ( 'NONE', #2504, 1000.000000000000000 ) ;
#38128 = CARTESIAN_POINT ( 'NONE',  ( -177.4999999999999716, 112.5000000000000000, 0.000000000000000000 ) ) ;
#38129 = CARTESIAN_POINT ( 'NONE',  ( 1.011271242968677653, 0.7347315653656002477, -3.333333333333333481 ) ) ;
#38130 = CARTESIAN_POINT ( 'NONE',  ( -0.7849184246622071814, 1.242376769534369041, 9.958264684458713489 ) ) ;
#38131 = VERTEX_POINT ( 'NONE', #20872 ) ;
#38132 = ORIENTED_EDGE ( 'NONE', *, *, #807, .T. ) ;
#38133 = ADVANCED_FACE ( 'NONE', ( #16271 ), #43461, .F. ) ;
#38134 = LINE ( 'NONE', #46023, #44701 ) ;
#38135 = CARTESIAN_POINT ( 'NONE',  ( -5.320787806781440921, 8.466948512633457824, -1.544988095791843818E-15 ) ) ;
#38136 = PRESENTATION_LAYER_ASSIGNMENT (  '', '', ( #9438 ) ) ;
#38137 = EDGE_CURVE ( 'NONE', #39319, #7126, #36554, .T. ) ;
#38138 = VERTEX_POINT ( 'NONE', #43958 ) ;
#38139 = EDGE_CURVE ( 'NONE', #16044, #24255, #32678, .T. ) ;
#38140 = CARTESIAN_POINT ( 'NONE',  ( 210.0000000000000568, 0.000000000000000000, -37.43171244307202272 ) ) ;
#38141 = DIRECTION ( 'NONE',  ( 0.000000000000000000, 0.000000000000000000, -1.000000000000000000 ) ) ;
#38142 = CARTESIAN_POINT ( 'NONE',  ( 195.0540265531851105, 2.143131898507880377E-16, -37.43171244307205825 ) ) ;
#38143 = VECTOR ( 'NONE', #27668, 1000.000000000000000 ) ;
#38144 = ORIENTED_EDGE ( 'NONE', *, *, #2473, .T. ) ;
#38145 = VERTEX_POINT ( 'NONE', #48278 ) ;
#38146 = VERTEX_POINT ( 'NONE', #4467 ) ;
#38147 =( GEOMETRIC_REPRESENTATION_CONTEXT ( 3 ) GLOBAL_UNCERTAINTY_ASSIGNED_CONTEXT ( ( #50562 ) ) GLOBAL_UNIT_ASSIGNED_CONTEXT ( ( #5960, #22622, #9804 ) ) REPRESENTATION_CONTEXT ( 'NONE', 'WORKASPACE' ) );
#38148 = AXIS2_PLACEMENT_3D ( 'NONE', #5840, #13023, #5069 ) ;
#38149 = DIRECTION ( 'NONE',  ( 1.000000000000000000, -4.996003610813203446E-16, 1.033975765691284410E-24 ) ) ;
#38150 = CARTESIAN_POINT ( 'NONE',  ( 111.5540265531850679, 0.000000000000000000, -37.43171244307205825 ) ) ;
#38151 = CARTESIAN_POINT ( 'NONE',  ( -17.34922095635781147, -33.24536858281880569, 8.914903342594564961 ) ) ;
#38152 = VERTEX_POINT ( 'NONE', #44449 ) ;
#38153 = FACE_OUTER_BOUND ( 'NONE', #20006, .T. ) ;
#38154 = DIRECTION ( 'NONE',  ( -0.000000000000000000, -0.000000000000000000, -1.000000000000000000 ) ) ;
#38155 = LINE ( 'NONE', #7344, #8160 ) ;
#38156 = ORIENTED_EDGE ( 'NONE', *, *, #13992, .T. ) ;
#38157 = ORIENTED_EDGE ( 'NONE', *, *, #20109, .F. ) ;
#38158 = FACE_OUTER_BOUND ( 'NONE', #23952, .T. ) ;
#38159 = ADVANCED_FACE ( 'NONE', ( #630 ), #40135, .T. ) ;
#38160 = LINE ( 'NONE', #12833, #20163 ) ;
#38161 = CARTESIAN_POINT ( 'NONE',  ( 2.089000987151460986, 7.666878472665119126, 9.432811472610055148 ) ) ;
#38162 = ORIENTED_EDGE ( 'NONE', *, *, #15905, .T. ) ;
#38163 = EDGE_LOOP ( 'NONE', ( #34036, #37685, #32786, #29511, #39543 ) ) ;
#38164 = DIRECTION ( 'NONE',  ( 0.000000000000000000, 1.000000000000000000, 0.000000000000000000 ) ) ;
#38165 = PLANE ( 'NONE',  #4290 ) ;
#38166 = VECTOR ( 'NONE', #5486, 1000.000000000000000 ) ;
#38167 = CARTESIAN_POINT ( 'NONE',  ( 210.0000000000000568, 0.000000000000000000, 40.81828755692798438 ) ) ;
#38168 = CARTESIAN_POINT ( 'NONE',  ( 339.9999999999998863, -168.9999999999999432, 357.9999999999997726 ) ) ;
#38169 = ADVANCED_FACE ( 'NONE', ( #23719 ), #24233, .F. ) ;
#38170 = LINE ( 'NONE', #49883, #49454 ) ;
#38171 = CIRCLE ( 'NONE', #29948, 1.750000000000001554 ) ;
#38172 = VERTEX_POINT ( 'NONE', #44207 ) ;
#38173 = DIRECTION ( 'NONE',  ( 1.000000000000000000, 0.000000000000000000, 0.000000000000000000 ) ) ;
#38174 = DIRECTION ( 'NONE',  ( 1.000000000000000000, 0.000000000000000000, 0.000000000000000000 ) ) ;
#38176 = CIRCLE ( 'NONE', #22579, 3.749999999999975575 ) ;
#38175 = CARTESIAN_POINT ( 'NONE',  ( -86.69597344681494633, -1.750000000000010658, -119.1817124430720440 ) ) ;
#38177 = CARTESIAN_POINT ( 'NONE',  ( -194.9999999999999432, -172.9999999999999716, 252.0000000000000568 ) ) ;
#38178 = CARTESIAN_POINT ( 'NONE',  ( 210.0000000000000568, 0.000000000000000000, -119.1817124430720440 ) ) ;
#38179 =( BOUNDED_CURVE ( )  B_SPLINE_CURVE ( 3, ( #46118, #7942, #12040, #46627 ),
 .UNSPECIFIED., .F., .F. ) 
 B_SPLINE_CURVE_WITH_KNOTS ( ( 4, 4 ),
 ( 3.141592653589793116, 4.712388980384689674 ),
 .UNSPECIFIED. ) 
 CURVE ( )  GEOMETRIC_REPRESENTATION_ITEM ( )  RATIONAL_B_SPLINE_CURVE ( ( 1.000000000000000000, 0.8047378541243649375, 0.8047378541243649375, 1.000000000000000000 ) ) 
 REPRESENTATION_ITEM ( '' )  );
#38180 = VECTOR ( 'NONE', #46605, 1000.000000000000114 ) ;
#38181 = ADVANCED_FACE ( 'NONE', ( #47280 ), #27825, .F. ) ;
#38182 = ADVANCED_FACE ( 'NONE', ( #24734 ), #40388, .F. ) ;
#38183 = CIRCLE ( 'NONE', #22589, 5.000000000000000888 ) ;
#38184 = ORIENTED_EDGE ( 'NONE', *, *, #38427, .T. ) ;
#38185 = CARTESIAN_POINT ( 'NONE',  ( 27.33593271309472073, -41.94268121623323964, -9.367992836599954742 ) ) ;
#38186 =( BOUNDED_CURVE ( )  B_SPLINE_CURVE ( 3, ( #12109, #569, #32617, #5147 ),
 .UNSPECIFIED., .F., .F. ) 
 B_SPLINE_CURVE_WITH_KNOTS ( ( 4, 4 ),
 ( 1.570796326794896558, 3.141592653589793116 ),
 .UNSPECIFIED. ) 
 CURVE ( )  GEOMETRIC_REPRESENTATION_ITEM ( )  RATIONAL_B_SPLINE_CURVE ( ( 1.000000000000000000, 0.8047378541243649375, 0.8047378541243649375, 1.000000000000000000 ) ) 
 REPRESENTATION_ITEM ( '' )  );
#38187 = ADVANCED_FACE ( 'NONE', ( #24482 ), #25737, .T. ) ;
#38188 = DIRECTION ( 'NONE',  ( -0.000000000000000000, -0.000000000000000000, -1.000000000000000000 ) ) ;
#38189 = CARTESIAN_POINT ( 'NONE',  ( -1.377509002708424468, 0.6027468487255034368, 9.927319414211229542 ) ) ;
#38190 = CIRCLE ( 'NONE', #497, 4.000000000000003553 ) ;
#38191 = VECTOR ( 'NONE', #13497, 1000.000000000000000 ) ;
#38192 = EDGE_CURVE ( 'NONE', #970, #13545, #14435, .T. ) ;
#38193 = EDGE_CURVE ( 'NONE', #15132, #26345, #44702, .T. ) ;
#38194 = EDGE_LOOP ( 'NONE', ( #35054, #23436, #9991, #41651, #50596, #14469 ) ) ;
#38195 = ORIENTED_EDGE ( 'NONE', *, *, #46586, .T. ) ;
#38196 = LINE ( 'NONE', #34580, #32111 ) ;
#38197 = DIRECTION ( 'NONE',  ( -1.000000000000000000, 0.000000000000000000, 0.000000000000000000 ) ) ;
#38198 = CARTESIAN_POINT ( 'NONE',  ( 165.0000000000000000, -5.999999999999950262, 339.9999999999998863 ) ) ;
#38199 = CARTESIAN_POINT ( 'NONE',  ( -88.44597344681497475, 0.000000000000000000, -40.93171244307205825 ) ) ;
#38200 = EDGE_CURVE ( 'NONE', #14294, #49029, #17154, .T. ) ;
#38201 = ORIENTED_EDGE ( 'NONE', *, *, #4264, .F. ) ;
#38202 = CYLINDRICAL_SURFACE ( 'NONE', #49437, 1.750000000000001554 ) ;
#38203 = ORIENTED_EDGE ( 'NONE', *, *, #6276, .F. ) ;
#38204 = ORIENTED_EDGE ( 'NONE', *, *, #49663, .T. ) ;
#38205 = FACE_OUTER_BOUND ( 'NONE', #18841, .T. ) ;
#38206 = CIRCLE ( 'NONE', #21812, 3.749999999999975575 ) ;
#38207 = ORIENTED_EDGE ( 'NONE', *, *, #1064, .T. ) ;
#38208 = CARTESIAN_POINT ( 'NONE',  ( -127.7210997126620242, 1.749999999999996891, 39.79316129108089228 ) ) ;
#38209 = CARTESIAN_POINT ( 'NONE',  ( -30.87089393895367095, 12.69923079256638587, -9.367992836599954742 ) ) ;
#38210 = VECTOR ( 'NONE', #46482, 1000.000000000000000 ) ;
#38211 = CARTESIAN_POINT ( 'NONE',  ( 210.0000000000000568, 0.000000000000000000, 42.56828755692799149 ) ) ;
#38212 = PLANE ( 'NONE',  #20683 ) ;
#38213 = CARTESIAN_POINT ( 'NONE',  ( 167.0000000000000284, 175.0000000000000284, 343.9999999999998863 ) ) ;
#38214 = ORIENTED_EDGE ( 'NONE', *, *, #4341, .F. ) ;
#38215 = CYLINDRICAL_SURFACE ( 'NONE', #28108, 2.000000000000001776 ) ;
#38216 = CARTESIAN_POINT ( 'NONE',  ( -88.44597344681494633, 1.025126265847089435, 82.56828755692798438 ) ) ;
#38217 = FACE_OUTER_BOUND ( 'NONE', #29876, .T. ) ;
#38218 = CARTESIAN_POINT ( 'NONE',  ( -14.99999999999906919, 16.00000000000000000, -24.99999999999999289 ) ) ;
#38219 = AXIS2_PLACEMENT_3D ( 'NONE', #25829, #1969, #41974 ) ;
#38220 = VERTEX_POINT ( 'NONE', #14164 ) ;
#38221 = CARTESIAN_POINT ( 'NONE',  ( -8.445973446814964092, -1.025126265847097429, 79.06828755692792754 ) ) ;
#38222 = CARTESIAN_POINT ( 'NONE',  ( -3.345242017215803276, 2.159124855890678596, -2.642742795433417058E-16 ) ) ;
#38223 = ORIENTED_EDGE ( 'NONE', *, *, #3704, .T. ) ;
#38224 = VECTOR ( 'NONE', #43062, 1000.000000000000000 ) ;
#38225 = ORIENTED_EDGE ( 'NONE', *, *, #49310, .T. ) ;
#38226 = EDGE_LOOP ( 'NONE', ( #1729, #46365, #48032, #18994, #40950, #48, #18618, #45323, #45801, #50544, #45960, #20595, #46809, #48609, #13446, #32016, #9312, #24367, #35987, #32338, #7370, #44037, #3805, #48568, #6948 ) ) ;
#38227 = DIRECTION ( 'NONE',  ( 0.000000000000000000, 1.000000000000000000, 0.000000000000000000 ) ) ;
#38228 = DIRECTION ( 'NONE',  ( 0.000000000000000000, 2.537652627714642000E-15, 1.000000000000000000 ) ) ;
#38229 = ORIENTED_EDGE ( 'NONE', *, *, #40577, .T. ) ;
#38230 = ADVANCED_FACE ( 'NONE', ( #21625 ), #17281, .T. ) ;
#38231 = VECTOR ( 'NONE', #35183, 1000.000000000000000 ) ;
#38232 = LINE ( 'NONE', #14593, #14275 ) ;
#38233 = FACE_BOUND ( 'NONE', #10067, .T. ) ;
#38234 = CARTESIAN_POINT ( 'NONE',  ( -46.69597344681494633, 1.750000000000010214, 40.81828755692798438 ) ) ;
#38235 = LINE ( 'NONE', #38485, #25822 ) ;
#38236 = CARTESIAN_POINT ( 'NONE',  ( 193.3040265531851105, 0.000000000000000000, 165.0000000000000000 ) ) ;
#38237 = DIRECTION ( 'NONE',  ( -0.000000000000000000, -0.000000000000000000, -1.000000000000000000 ) ) ;
#38238 = ORIENTED_EDGE ( 'NONE', *, *, #38410, .T. ) ;
#38239 = DIRECTION ( 'NONE',  ( 1.000000000000000000, 0.000000000000000000, 0.000000000000000000 ) ) ;
#38240 = CARTESIAN_POINT ( 'NONE',  ( 34.38425513258721367, -36.82177522737821107, 8.807470649214879543 ) ) ;
#38241 = ADVANCED_FACE ( 'NONE', ( #25994 ), #22136, .T. ) ;
#38242 = EDGE_CURVE ( 'NONE', #16517, #42175, #9330, .T. ) ;
#38243 = VECTOR ( 'NONE', #30622, 1000.000000000000000 ) ;
#38245 = AXIS2_PLACEMENT_3D ( 'NONE', #5191, #37288, #25708 ) ;
#38244 = LINE ( 'NONE', #30028, #30628 ) ;
#38246 = DIRECTION ( 'NONE',  ( 0.000000000000000000, 1.000000000000000000, 0.000000000000000000 ) ) ;
#38247 = ORIENTED_EDGE ( 'NONE', *, *, #32563, .T. ) ;
#38248 = CARTESIAN_POINT ( 'NONE',  ( -164.9459734468149463, 1.025126265847089657, 119.0682875569279560 ) ) ;
#38249 = CYLINDRICAL_SURFACE ( 'NONE', #36013, 2.000000000000001776 ) ;
#38250 = EDGE_CURVE ( 'NONE', #21405, #34922, #32138, .T. ) ;
#38251 = CARTESIAN_POINT ( 'NONE',  ( -1.401228687704686449, 0.7134216605328093097, 9.945241992664930919 ) ) ;
#38252 = DIRECTION ( 'NONE',  ( -0.000000000000000000, -0.000000000000000000, -1.000000000000000000 ) ) ;
#38253 = ADVANCED_FACE ( 'NONE', ( #41382 ), #25740, .T. ) ;
#38254 = EDGE_CURVE ( 'NONE', #38752, #50500, #22694, .T. ) ;
#38255 = VECTOR ( 'NONE', #24397, 1000.000000000000000 ) ;
#38256 = EDGE_LOOP ( 'NONE', ( #50511, #44051, #17506, #22002, #15977, #1343 ) ) ;
#38257 = ORIENTED_EDGE ( 'NONE', *, *, #11088, .F. ) ;
#38258 = CARTESIAN_POINT ( 'NONE',  ( -6.695973446814940111, 1.750000000000023315, 160.8182875569279702 ) ) ;
#38259 = VECTOR ( 'NONE', #33746, 1000.000000000000000 ) ;
#38260 = ORIENTED_EDGE ( 'NONE', *, *, #41993, .F. ) ;
#38261 = ADVANCED_FACE ( 'NONE', ( #33200, #29083 ), #13675, .T. ) ;
#38262 = LINE ( 'NONE', #33638, #30340 ) ;
#38263 = CYLINDRICAL_SURFACE ( 'NONE', #37245, 1.750000000000001554 ) ;
#38264 = ORIENTED_EDGE ( 'NONE', *, *, #7621, .F. ) ;
#38265 = CYLINDRICAL_SURFACE ( 'NONE', #28138, 1.750000000000015543 ) ;
#38266 = ORIENTED_EDGE ( 'NONE', *, *, #18323, .F. ) ;
#38267 = AXIS2_PLACEMENT_3D ( 'NONE', #41269, #49684, #45838 ) ;
#38268 = CARTESIAN_POINT ( 'NONE',  ( 339.9999999999999432, -168.9999999999999432, -342.0000000000001705 ) ) ;
#38269 = ORIENTED_EDGE ( 'NONE', *, *, #31515, .F. ) ;
#38270 = CARTESIAN_POINT ( 'NONE',  ( 71.55402655318505367, 0.000000000000000000, -37.43171244307200141 ) ) ;
#38271 = CARTESIAN_POINT ( 'NONE',  ( 341.9999999999999432, -165.0000000000001137, -106.0000000000001990 ) ) ;
#38272 = ORIENTED_EDGE ( 'NONE', *, *, #1101, .T. ) ;
#38273 = CARTESIAN_POINT ( 'NONE',  ( 194.9999999999999716, 164.9999999999999716, 500.0000000000000000 ) ) ;
#38274 = CARTESIAN_POINT ( 'NONE',  ( 3.087186397306452612, 2.514307945609885131, -2.642742795433417058E-16 ) ) ;
#38275 = CYLINDRICAL_SURFACE ( 'NONE', #48620, 1.750000000000001554 ) ;
#38276 = ORIENTED_EDGE ( 'NONE', *, *, #7117, .F. ) ;
#38277 = VERTEX_POINT ( 'NONE', #33448 ) ;
#38278 = CARTESIAN_POINT ( 'NONE',  ( -33.43156050989129824, 4.370686678976795747, 8.807470649214879543 ) ) ;
#38279 = CARTESIAN_POINT ( 'NONE',  ( -0.7139173712339883515, 1.401061409226810994, 9.927288994922816912 ) ) ;
#38280 = ORIENTED_EDGE ( 'NONE', *, *, #23609, .F. ) ;
#38281 = AXIS2_PLACEMENT_3D ( 'NONE', #22729, #17864, #15036 ) ;
#38282 = B_SPLINE_CURVE_WITH_KNOTS ( 'NONE', 3,
 ( #16482, #335, #39846, #46974 ),
 .UNSPECIFIED., .F., .F.,
 ( 4, 4 ),
 ( 0.8097120833243680593, 0.9322955464062561148 ),
 .UNSPECIFIED. ) ;
#38283 = DIRECTION ( 'NONE',  ( 0.000000000000000000, 1.000000000000000000, 0.000000000000000000 ) ) ;
#38284 = FACE_OUTER_BOUND ( 'NONE', #10854, .T. ) ;
#38285 = ORIENTED_EDGE ( 'NONE', *, *, #39131, .F. ) ;
#38286 = LINE ( 'NONE', #2342, #17985 ) ;
#38287 = EDGE_CURVE ( 'NONE', #40841, #41782, #12382, .T. ) ;
#38288 = CARTESIAN_POINT ( 'NONE',  ( -208.4459734468148611, 1.025126265847089435, -77.43171244307200141 ) ) ;
#38289 = VERTEX_POINT ( 'NONE', #29334 ) ;
#38290 = ADVANCED_FACE ( 'NONE', ( #41125 ), #13910, .F. ) ;
#38291 = CARTESIAN_POINT ( 'NONE',  ( -1.011271242968683426, -0.7347315653655928092, 10.00000000000000000 ) ) ;
#38292 = CARTESIAN_POINT ( 'NONE',  ( 26.18032376592674737, -21.95228666728361233, 7.455576670931136185 ) ) ;
#38293 = PLANE ( 'NONE',  #1707 ) ;
#38294 = LINE ( 'NONE', #6965, #12451 ) ;
#38295 = ORIENTED_EDGE ( 'NONE', *, *, #21373, .F. ) ;
#38296 = CARTESIAN_POINT ( 'NONE',  ( -13.35436367797847801, -31.26996044524040741, 7.906207997025717304 ) ) ;
#38297 = DIRECTION ( 'NONE',  ( 0.000000000000000000, 5.664403186863042467E-17, 1.000000000000000000 ) ) ;
#38298 = CARTESIAN_POINT ( 'NONE',  ( 1.011271242968677653, 0.7347315653656002477, 3.333333333333333481 ) ) ;
#38299 = ORIENTED_EDGE ( 'NONE', *, *, #49062, .F. ) ;
#38300 = AXIS2_PLACEMENT_3D ( 'NONE', #47499, #39102, #38846 ) ;
#38301 = EDGE_LOOP ( 'NONE', ( #1181, #45296, #12482, #785 ) ) ;
#38302 = SHAPE_REPRESENTATION_RELATIONSHIP ( 'NONE' , 'NONE' ,  #34661, #42356 ) ;
#38303 = DIRECTION ( 'NONE',  ( -1.000000000000000000, 0.000000000000000000, -7.793956916774525800E-48 ) ) ;
#38304 = FACE_OUTER_BOUND ( 'NONE', #777, .T. ) ;
#38305 = CARTESIAN_POINT ( 'NONE',  ( -40.00000000000000000, 0.000000000000000000, 790.0000000000000000 ) ) ;
#38306 = MANIFOLD_SOLID_BREP ( 'Cut-Extrude1[1]', #37621 ) ;
#38307 = LINE ( 'NONE', #11079, #15958 ) ;
#38308 = CARTESIAN_POINT ( 'NONE',  ( 342.0000000000000568, 172.0000000000000000, 346.9999999999998295 ) ) ;
#38309 = ORIENTED_EDGE ( 'NONE', *, *, #46224, .F. ) ;
#38310 = CARTESIAN_POINT ( 'NONE',  ( 46.11867747200574996, -19.86470446310233484, -8.016098858316199838 ) ) ;
#38311 = CARTESIAN_POINT ( 'NONE',  ( -19.99999999999878142, 17.00000000000000000, 5.000000000000004441 ) ) ;
#38312 = DIRECTION ( 'NONE',  ( -0.000000000000000000, -0.000000000000000000, -1.000000000000000000 ) ) ;
#38314 = ORIENTED_EDGE ( 'NONE', *, *, #23710, .T. ) ;
#38313 = AXIS2_PLACEMENT_3D ( 'NONE', #32296, #28930, #40742 ) ;
#38315 = CARTESIAN_POINT ( 'NONE',  ( -208.1473046169136580, -154.8119894309599260, 22.84256005001721945 ) ) ;
#38316 = EDGE_LOOP ( 'NONE', ( #43612, #21676, #22290, #19797, #41073, #22655 ) ) ;
#38317 = ADVANCED_FACE ( 'NONE', ( #10831 ), #14681, .T. ) ;
#38318 = DIRECTION ( 'NONE',  ( 0.000000000000000000, 0.000000000000000000, 1.000000000000000000 ) ) ;
#38319 = FACE_OUTER_BOUND ( 'NONE', #25687, .T. ) ;
#38320 = LINE ( 'NONE', #7249, #28000 ) ;
#38321 = ORIENTED_EDGE ( 'NONE', *, *, #6413, .T. ) ;
#38322 =( BOUNDED_CURVE ( )  B_SPLINE_CURVE ( 3, ( #1486, #28924, #35888, #20457 ),
 .UNSPECIFIED., .F., .F. ) 
 B_SPLINE_CURVE_WITH_KNOTS ( ( 4, 4 ),
 ( 3.141592653589793116, 4.712388980384689674 ),
 .UNSPECIFIED. ) 
 CURVE ( )  GEOMETRIC_REPRESENTATION_ITEM ( )  RATIONAL_B_SPLINE_CURVE ( ( 1.000000000000000000, 0.8047378541243649375, 0.8047378541243649375, 1.000000000000000000 ) ) 
 REPRESENTATION_ITEM ( '' )  );
#38323 = CARTESIAN_POINT ( 'NONE',  ( -1.133908876584336367, -0.5183204401656656968, 9.981352469109934233 ) ) ;
#38324 = ORIENTED_EDGE ( 'NONE', *, *, #35334, .T. ) ;
#38325 = CARTESIAN_POINT ( 'NONE',  ( 48.33712804702526000, 13.03701565032775456, -9.367992836599954742 ) ) ;
#38326 = CARTESIAN_POINT ( 'NONE',  ( 210.0000000000000568, 0.000000000000000000, -39.18171244307202983 ) ) ;
#38327 = DIRECTION ( 'NONE',  ( -1.000000000000000000, 0.000000000000000000, 0.000000000000000000 ) ) ;
#38328 =( BOUNDED_CURVE ( )  B_SPLINE_CURVE ( 3, ( #12323, #50516, #7483, #43123 ),
 .UNSPECIFIED., .F., .F. ) 
 B_SPLINE_CURVE_WITH_KNOTS ( ( 4, 4 ),
 ( 4.712388980384703885, 6.283185307179586232 ),
 .UNSPECIFIED. ) 
 CURVE ( )  GEOMETRIC_REPRESENTATION_ITEM ( )  RATIONAL_B_SPLINE_CURVE ( ( 1.000000000000000000, 0.8047378541243683792, 0.8047378541243683792, 1.000000000000000000 ) ) 
 REPRESENTATION_ITEM ( '' )  );
#38329 = ORIENTED_EDGE ( 'NONE', *, *, #41582, .F. ) ;
#38330 = ORIENTED_EDGE ( 'NONE', *, *, #16147, .T. ) ;
#38331 = CARTESIAN_POINT ( 'NONE',  ( -5.505322767148756569, 37.09368438467003415, 8.914903342594564961 ) ) ;
#38332 = CARTESIAN_POINT ( 'NONE',  ( 0.1425549192113746144, -1.238581250503543618, 9.981352469109934233 ) ) ;
#38333 = VERTEX_POINT ( 'NONE', #49780 ) ;
#38334 = EDGE_LOOP ( 'NONE', ( #40454, #9493, #34848, #20216, #40476, #10875, #7049, #33807 ) ) ;
#38335 = CARTESIAN_POINT ( 'NONE',  ( 34.32915281903212446, 1.750000000000010214, -120.2068387089191219 ) ) ;
#38336 = LINE ( 'NONE', #26270, #1347 ) ;
#38337 = CARTESIAN_POINT ( 'NONE',  ( -114.9999999999984652, 16.00000000000000000, 60.00000000000000000 ) ) ;
#38338 = ORIENTED_EDGE ( 'NONE', *, *, #36523, .T. ) ;
#38339 = LINE ( 'NONE', #7269, #36665 ) ;
#38340 = ORIENTED_EDGE ( 'NONE', *, *, #36436, .T. ) ;
#38341 =( BOUNDED_CURVE ( )  B_SPLINE_CURVE ( 3, ( #18869, #34550, #35329, #46306 ),
 .UNSPECIFIED., .F., .F. ) 
 B_SPLINE_CURVE_WITH_KNOTS ( ( 4, 4 ),
 ( 0.000000000000000000, 1.570796326794896558 ),
 .UNSPECIFIED. ) 
 CURVE ( )  GEOMETRIC_REPRESENTATION_ITEM ( )  RATIONAL_B_SPLINE_CURVE ( ( 1.000000000000000000, 0.8047378541243649375, 0.8047378541243649375, 1.000000000000000000 ) ) 
 REPRESENTATION_ITEM ( '' )  );
#38342 = LINE ( 'NONE', #35504, #1743 ) ;
#38343 = CARTESIAN_POINT ( 'NONE',  ( -46.69597344681494633, -1.750000000000010658, -119.1817124430720440 ) ) ;
#38344 = ORIENTED_EDGE ( 'NONE', *, *, #42799, .F. ) ;
#38345 = AXIS2_PLACEMENT_3D ( 'NONE', #29377, #48579, #36857 ) ;
#38346 = ORIENTED_EDGE ( 'NONE', *, *, #47904, .T. ) ;
#38347 = ORIENTED_EDGE ( 'NONE', *, *, #22132, .F. ) ;
#38348 = CARTESIAN_POINT ( 'NONE',  ( 340.0000000000000568, 181.0000000000000284, 355.9999999999998295 ) ) ;
#38349 = CARTESIAN_POINT ( 'NONE',  ( -28.96803024440907137, -18.11533787072017176, 7.455576670931136185 ) ) ;
#38350 = ORIENTED_EDGE ( 'NONE', *, *, #42108, .T. ) ;
#38351 = PLANE ( 'NONE',  #48483 ) ;
#38352 = ORIENTED_EDGE ( 'NONE', *, *, #26822, .F. ) ;
#38353 = CARTESIAN_POINT ( 'NONE',  ( 0.000000000000000000, 184.8000000000000114, 340.1999999999997044 ) ) ;
#38354 = ORIENTED_EDGE ( 'NONE', *, *, #44717, .F. ) ;
#38355 = CARTESIAN_POINT ( 'NONE',  ( -26.18032376592659105, 21.95228666728381128, 7.455576670931136185 ) ) ;
#38356 = CARTESIAN_POINT ( 'NONE',  ( 2.892039187330371242, -1.502206308778212929, 9.799352050262459812 ) ) ;
#38357 = CARTESIAN_POINT ( 'NONE',  ( -15.62858259096117841, 5.755205073598721910, -9.683996418299976483 ) ) ;
#38358 = DIRECTION ( 'NONE',  ( -0.000000000000000000, -0.000000000000000000, -1.000000000000000000 ) ) ;
#38359 = DIRECTION ( 'NONE',  ( -6.765175596986471882E-16, 0.9749645535258953943, 0.2223603367690637489 ) ) ;
#38360 = VERTEX_POINT ( 'NONE', #23404 ) ;
#38361 = FACE_OUTER_BOUND ( 'NONE', #3786, .T. ) ;
#38362 = VECTOR ( 'NONE', #38864, 1000.000000000000000 ) ;
#38363 = FACE_OUTER_BOUND ( 'NONE', #9624, .T. ) ;
#38364 = B_SPLINE_SURFACE_WITH_KNOTS ( 'NONE', 3, 3, ( 
 ( #2684, #7053, #38366, #34511 ),
 ( #50090, #29889, #45509, #22198 ),
 ( #10397, #15003, #46509, #37865 ),
 ( #46259, #11401, #11157, #18321 ) ),
 .UNSPECIFIED., .F., .F., .F.,
 ( 4, 4 ),
 ( 4, 4 ),
 ( 0.000000000000000000, 1.000000000000000000 ),
 ( 0.000000000000000000, 1.000000000000000000 ),
 .UNSPECIFIED. ) ;
#38365 = DIRECTION ( 'NONE',  ( 0.000000000000000000, 0.000000000000000000, 1.000000000000000000 ) ) ;
#38366 = CARTESIAN_POINT ( 'NONE',  ( -14.91630425054805187, 7.943683830272224355, -9.008049429158100807 ) ) ;
#38367 = SPHERICAL_SURFACE ( 'NONE', #26405, 0.5000000000000000000 ) ;
#38368 = DIRECTION ( 'NONE',  ( 1.612977847700450206E-50, 0.000000000000000000, 1.000000000000000000 ) ) ;
#38369 = EDGE_CURVE ( 'NONE', #37697, #40121, #39073, .T. ) ;
#38370 = CARTESIAN_POINT ( 'NONE',  ( -88.44597344681497475, 0.000000000000000000, 165.0000000000000000 ) ) ;
#38371 = CARTESIAN_POINT ( 'NONE',  ( 31.93002621080262671, 9.285431160462559674, -2.408242355805840784 ) ) ;
#38372 = ADVANCED_FACE ( 'NONE', ( #26489 ), #3376, .T. ) ;
#38373 = ORIENTED_EDGE ( 'NONE', *, *, #30351, .F. ) ;
#38374 = EDGE_CURVE ( 'NONE', #35246, #14478, #14942, .T. ) ;
#38375 = AXIS2_PLACEMENT_3D ( 'NONE', #34196, #35662, #15881 ) ;
#38376 = FACE_OUTER_BOUND ( 'NONE', #8466, .T. ) ;
#38377 = MANIFOLD_SOLID_BREP ( 'Square tube 20 X 20 X 2(1)[9]', #38423 ) ;
#38378 = CARTESIAN_POINT ( 'NONE',  ( -1.565984505217804967, 1.491012526244388070, 9.885585981620945262 ) ) ;
#38379 = FACE_OUTER_BOUND ( 'NONE', #30117, .T. ) ;
#38380 = EDGE_CURVE ( 'NONE', #11761, #35393, #5487, .T. ) ;
#38381 = ADVANCED_FACE ( 'NONE', ( #26746 ), #7504, .F. ) ;
#38382 = ORIENTED_EDGE ( 'NONE', *, *, #22038, .T. ) ;
#38383 = ORIENTED_EDGE ( 'NONE', *, *, #27069, .T. ) ;
#38384 = CARTESIAN_POINT ( 'NONE',  ( -0.5705203167777310735, -1.169354363542817854, 9.986087673579140400 ) ) ;
#38385 = EDGE_CURVE ( 'NONE', #26183, #36777, #27832, .T. ) ;
#38386 = ORIENTED_EDGE ( 'NONE', *, *, #20542, .T. ) ;
#38387 = ORIENTED_EDGE ( 'NONE', *, *, #48675, .T. ) ;
#38388 = CARTESIAN_POINT ( 'NONE',  ( -10.06660411345808548, 8.486842105263157521, 18.70408263333243681 ) ) ;
#38389 = DIRECTION ( 'NONE',  ( 0.000000000000000000, 0.000000000000000000, 1.000000000000000000 ) ) ;
#38390 = CARTESIAN_POINT ( 'NONE',  ( -7.576114424932982594, 33.14742743729794938, 7.906207997025717304 ) ) ;
#38391 = ORIENTED_EDGE ( 'NONE', *, *, #40873, .F. ) ;
#38392 = ORIENTED_EDGE ( 'NONE', *, *, #23811, .T. ) ;
#38393 = ORIENTED_EDGE ( 'NONE', *, *, #32612, .F. ) ;
#38394 = ADVANCED_FACE ( 'NONE', ( #9015 ), #16210, .F. ) ;
#38395 = ADVANCED_FACE ( 'NONE', ( #40319 ), #32370, .T. ) ;
#38396 = CARTESIAN_POINT ( 'NONE',  ( 2.500000000000001776, 214.9999999999999716, -234.7500000000000000 ) ) ;
#38397 = FACE_OUTER_BOUND ( 'NONE', #26896, .T. ) ;
#38398 = LINE ( 'NONE', #3990, #34961 ) ;
#38399 = EDGE_CURVE ( 'NONE', #5180, #13146, #31433, .T. ) ;
#38400 = ORIENTED_EDGE ( 'NONE', *, *, #22690, .F. ) ;
#38401 = EDGE_CURVE ( 'NONE', #31946, #21137, #28518, .T. ) ;
#38402 = LINE ( 'NONE', #25831, #43165 ) ;
#38403 = CARTESIAN_POINT ( 'NONE',  ( 113.3040265531850537, 0.000000000000000000, -165.0000000000000000 ) ) ;
#38404 = DIRECTION ( 'NONE',  ( -1.000000000000000000, 0.000000000000000000, 1.860490536778032451E-50 ) ) ;
#38405 = EDGE_LOOP ( 'NONE', ( #24009, #24459, #9963, #17996 ) ) ;
#38406 = VERTEX_POINT ( 'NONE', #20561 ) ;
#38407 = FACE_OUTER_BOUND ( 'NONE', #45047, .T. ) ;
#38408 = EDGE_CURVE ( 'NONE', #28669, #576, #1843, .T. ) ;
#38409 = CARTESIAN_POINT ( 'NONE',  ( -0.9870575514055066613, -1.980598328282574316, 9.881002359080278907 ) ) ;
#38410 = EDGE_CURVE ( 'NONE', #41166, #35123, #47101, .T. ) ;
#38411 = DIRECTION ( 'NONE',  ( 0.4740998230350172427, 0.3386427307392981256, -0.8127425537743157014 ) ) ;
#38412 = ORIENTED_EDGE ( 'NONE', *, *, #25887, .T. ) ;
#38413 = ORIENTED_EDGE ( 'NONE', *, *, #34684, .T. ) ;
#38414 = CARTESIAN_POINT ( 'NONE',  ( 31.28234235046230793, 11.28615439405779064, -3.760136334089591248 ) ) ;
#38415 = DIRECTION ( 'NONE',  ( -1.000000000000000000, 0.000000000000000000, -1.612977847700450206E-50 ) ) ;
#38416 = CARTESIAN_POINT ( 'NONE',  ( -164.9999999999987779, 17.00000000000000000, 30.00000000000000000 ) ) ;
#38417 = AXIS2_PLACEMENT_3D ( 'NONE', #45508, #41945, #30145 ) ;
#38418 = DIRECTION ( 'NONE',  ( -1.000000000000000000, -0.000000000000000000, -0.000000000000000000 ) ) ;
#38419 = EDGE_LOOP ( 'NONE', ( #46030, #44909, #19465, #36587 ) ) ;
#38420 = CARTESIAN_POINT ( 'NONE',  ( 111.5540265531850679, 0.000000000000000000, 165.0000000000000000 ) ) ;
#38421 = CARTESIAN_POINT ( 'NONE',  ( -114.9999999999997158, 16.00000000000000000, -84.99999999999998579 ) ) ;
#38422 = CARTESIAN_POINT ( 'NONE',  ( -2.134700047865557782, -5.564249483241940908, 1.036768327439263615E-15 ) ) ;
#38423 = CLOSED_SHELL ( 'NONE', ( #8303, #37132, #29173, #3640, #47079, #18589, #50232, #14929, #13775, #38182, #42200, #40626, #33303, #36650, #6958, #18909, #33339, #17155 ) ) ;
#38424 = EDGE_CURVE ( 'NONE', #7516, #16448, #49349, .T. ) ;
#38425 = CARTESIAN_POINT ( 'NONE',  ( 48.77035878734821495, 11.70366853303760379, -8.466730184410787174 ) ) ;
#38426 = EDGE_CURVE ( 'NONE', #43884, #13365, #8777, .T. ) ;
#38427 = EDGE_CURVE ( 'NONE', #29740, #13231, #39830, .T. ) ;
#38428 = CARTESIAN_POINT ( 'NONE',  ( 342.8284271247461561, -167.0000000000001137, 341.9999999999999432 ) ) ;
#38429 = ORIENTED_EDGE ( 'NONE', *, *, #24245, .T. ) ;
#38430 = DIRECTION ( 'NONE',  ( 0.000000000000000000, 0.000000000000000000, -1.000000000000000000 ) ) ;
#38431 = DIRECTION ( 'NONE',  ( -0.000000000000000000, -0.000000000000000000, -1.000000000000000000 ) ) ;
#38432 = DIRECTION ( 'NONE',  ( -1.000000000000000000, -0.000000000000000000, -0.000000000000000000 ) ) ;
#38433 = EDGE_CURVE ( 'NONE', #20298, #5511, #24425, .T. ) ;
#38434 = VERTEX_POINT ( 'NONE', #40072 ) ;
#38435 = CARTESIAN_POINT ( 'NONE',  ( -42.51732812238059722, -47.49695244670218131, 5.000000000000000000 ) ) ;
#38436 = FACE_OUTER_BOUND ( 'NONE', #9202, .T. ) ;
#38437 = ORIENTED_EDGE ( 'NONE', *, *, #40619, .T. ) ;
#38438 = CARTESIAN_POINT ( 'NONE',  ( -0.5391684635142623971, 1.495919383164612926, 9.933337522700158573 ) ) ;
#38439 = CARTESIAN_POINT ( 'NONE',  ( -7.721099712662037540, 1.750000000000022871, 159.7931612910808781 ) ) ;
#38440 = LINE ( 'NONE', #2513, #46100 ) ;
#38441 = CARTESIAN_POINT ( 'NONE',  ( 75.05402655318509630, 2.143131898507880377E-16, 2.568287556928006143 ) ) ;
#38442 = VERTEX_POINT ( 'NONE', #4158 ) ;
#38443 = LINE ( 'NONE', #14309, #19147 ) ;
#38444 = ORIENTED_EDGE ( 'NONE', *, *, #25960, .T. ) ;
#38446 = ORIENTED_EDGE ( 'NONE', *, *, #16569, .T. ) ;
#38445 = B_SPLINE_CURVE_WITH_KNOTS ( 'NONE', 3,
 ( #3961, #16275, #11926, #35293 ),
 .UNSPECIFIED., .F., .F.,
 ( 4, 4 ),
 ( 0.9811748202683098219, 0.9878904167554126703 ),
 .UNSPECIFIED. ) ;
#38447 = ADVANCED_FACE ( 'NONE', ( #15959 ), #8520, .T. ) ;
#38448 = DIRECTION ( 'NONE',  ( -1.612977847700450206E-50, 0.000000000000000000, -1.000000000000000000 ) ) ;
#38449 = VECTOR ( 'NONE', #36919, 1000.000000000000000 ) ;
#38450 = AXIS2_PLACEMENT_3D ( 'NONE', #23587, #31558, #47143 ) ;
#38451 = VERTEX_POINT ( 'NONE', #27758 ) ;
#38452 = LINE ( 'NONE', #46355, #18843 ) ;
#38453 = LINE ( 'NONE', #6881, #2768 ) ;
#38454 = ADVANCED_FACE ( 'NONE', ( #43391, #39569, #24172, #35977, #820, #16466 ), #32117, .T. ) ;
#38455 = CARTESIAN_POINT ( 'NONE',  ( -206.6959734468149463, 1.750000000000010658, -119.1817124430720440 ) ) ;
#38456 = CIRCLE ( 'NONE', #24528, 1.750000000000015543 ) ;
#38457 = AXIS2_PLACEMENT_3D ( 'NONE', #20017, #12078, #24392 ) ;
#38458 = CARTESIAN_POINT ( 'NONE',  ( -0.4548599190037587725, -1.225298710497772836, 9.945465957785113886 ) ) ;
#38459 = CIRCLE ( 'NONE', #30233, 4.000000000000003553 ) ;
#38460 = ORIENTED_EDGE ( 'NONE', *, *, #36636, .T. ) ;
#38461 = DIRECTION ( 'NONE',  ( 0.000000000000000000, 0.000000000000000000, 1.000000000000000000 ) ) ;
#38462 = CARTESIAN_POINT ( 'NONE',  ( 32.27890028733795447, 1.750000000000009548, 161.8434138227750907 ) ) ;
#38463 = PLANE ( 'NONE',  #3766 ) ;
#38464 = AXIS2_PLACEMENT_3D ( 'NONE', #30228, #11249, #46089 ) ;
#38465 = EDGE_CURVE ( 'NONE', #42661, #29738, #32623, .T. ) ;
#38466 = VERTEX_POINT ( 'NONE', #44633 ) ;
#38467 = EDGE_CURVE ( 'NONE', #19269, #40908, #2314, .T. ) ;
#38468 = DIRECTION ( 'NONE',  ( -0.000000000000000000, -3.186989995019654210E-49, -1.000000000000000000 ) ) ;
#38469 = DIRECTION ( 'NONE',  ( -1.000000000000000000, -0.000000000000000000, -0.000000000000000000 ) ) ;
#38470 = ORIENTED_EDGE ( 'NONE', *, *, #46575, .F. ) ;
#38471 = ORIENTED_EDGE ( 'NONE', *, *, #33976, .F. ) ;
#38472 = ORIENTED_EDGE ( 'NONE', *, *, #677, .T. ) ;
#38473 = CARTESIAN_POINT ( 'NONE',  ( 1.011271242968694084, -0.7347315653655782652, -3.333333333333333481 ) ) ;
#38474 = EDGE_CURVE ( 'NONE', #31155, #23256, #35535, .T. ) ;
#38475 = EDGE_CURVE ( 'NONE', #23653, #23447, #45763, .T. ) ;
#38476 = CARTESIAN_POINT ( 'NONE',  ( 15.73090589902275482, 29.60029367929053024, 1.847720168420772691 ) ) ;
#38477 = B_SPLINE_SURFACE_WITH_KNOTS ( 'NONE', 3, 3, ( 
 ( #48854, #26315, #45526, #22210 ),
 ( #34267, #9898, #22455, #13742 ),
 ( #2209, #45270, #41956, #38129 ),
 ( #6046, #14756, #2944, #18338 ) ),
 .UNSPECIFIED., .F., .F., .F.,
 ( 4, 4 ),
 ( 4, 4 ),
 ( 0.000000000000000000, 1.000000000000000000 ),
 ( 0.000000000000000000, 1.000000000000000000 ),
 .UNSPECIFIED. ) ;
#38478 = EDGE_LOOP ( 'NONE', ( #39366, #40291 ) ) ;
#38479 = EDGE_CURVE ( 'NONE', #24866, #14725, #33706, .T. ) ;
#38480 = CARTESIAN_POINT ( 'NONE',  ( 2.538055338523177440, 33.28424297489108596, -9.367992836599954742 ) ) ;
#38481 = SURFACE_STYLE_USAGE ( .BOTH. , #30504 ) ;
#38482 = FACE_BOUND ( 'NONE', #26497, .T. ) ;
#38483 = CARTESIAN_POINT ( 'NONE',  ( -8.277096487746778308, 50.00000000000000711, 7.455576670931136185 ) ) ;
#38484 = FACE_OUTER_BOUND ( 'NONE', #18426, .T. ) ;
#38485 = CARTESIAN_POINT ( 'NONE',  ( 181.0000000000000284, 2.775557561562891351E-14, -115.0000000000001563 ) ) ;
#38486 = DIRECTION ( 'NONE',  ( -1.000000000000000000, 0.000000000000000000, -0.000000000000000000 ) ) ;
#38487 = CARTESIAN_POINT ( 'NONE',  ( 8.843309649387377291, -14.11631751497145792, -2.870787844569587133 ) ) ;
#38488 =( BOUNDED_CURVE ( )  B_SPLINE_CURVE ( 3, ( #1971, #17618, #48873, #13759 ),
 .UNSPECIFIED., .F., .F. ) 
 B_SPLINE_CURVE_WITH_KNOTS ( ( 4, 4 ),
 ( 0.000000000000000000, 0.5599187270832621799 ),
 .UNSPECIFIED. ) 
 CURVE ( )  GEOMETRIC_REPRESENTATION_ITEM ( )  RATIONAL_B_SPLINE_CURVE ( ( 1.000000000000000000, 0.9740444450880465510, 0.9740444450880465510, 1.000000000000000000 ) ) 
 REPRESENTATION_ITEM ( '' )  );
#38489 = DIRECTION ( 'NONE',  ( 0.000000000000000000, 1.000000000000000000, 0.000000000000000000 ) ) ;
#38490 = VERTEX_POINT ( 'NONE', #21313 ) ;
#38491 = DIRECTION ( 'NONE',  ( -1.000000000000000000, -0.000000000000000000, -0.000000000000000000 ) ) ;
#38492 = CARTESIAN_POINT ( 'NONE',  ( 166.9999999999999716, -81.49999999999997158, -350.0000000000001705 ) ) ;
#38493 = EDGE_CURVE ( 'NONE', #8236, #35926, #10043, .T. ) ;
#38494 = CARTESIAN_POINT ( 'NONE',  ( -126.6959734468149321, -1.749999999999997335, -119.1817124430720440 ) ) ;
#38495 = DIRECTION ( 'NONE',  ( 0.000000000000000000, -1.000000000000000000, 0.000000000000000000 ) ) ;
#38496 = EDGE_LOOP ( 'NONE', ( #10248, #37465, #31271, #20486, #33724, #8046 ) ) ;
#38497 = VECTOR ( 'NONE', #38404, 1000.000000000000000 ) ;
#38498 = DIRECTION ( 'NONE',  ( 0.000000000000000000, 0.000000000000000000, 1.000000000000000000 ) ) ;
#38499 = CIRCLE ( 'NONE', #49044, 2.000000000000001776 ) ;
#38500 = DIRECTION ( 'NONE',  ( 0.000000000000000000, 0.000000000000000000, 1.000000000000000000 ) ) ;
#38501 = CARTESIAN_POINT ( 'NONE',  ( -29.39982726364978660, -16.78152490921149109, 8.356839323120299312 ) ) ;
#38502 = DIRECTION ( 'NONE',  ( -1.000000000000000000, -0.000000000000000000, -0.000000000000000000 ) ) ;
#38503 = CARTESIAN_POINT ( 'NONE',  ( -44.99506233596264337, -23.32283626942287214, 7.455576670931136185 ) ) ;
#38504 = AXIS2_PLACEMENT_3D ( 'NONE', #12740, #24545, #9647 ) ;
#38505 = ORIENTED_EDGE ( 'NONE', *, *, #43417, .T. ) ;
#38506 = ORIENTED_EDGE ( 'NONE', *, *, #29030, .T. ) ;
#38507 = CARTESIAN_POINT ( 'NONE',  ( 168.9999999999998579, -272.5000000000000000, -112.9999999999999005 ) ) ;
#38508 = ORIENTED_EDGE ( 'NONE', *, *, #28385, .F. ) ;
#38509 = CARTESIAN_POINT ( 'NONE',  ( 155.0540265531850537, 2.143131898507880377E-16, -160.9317124430720014 ) ) ;
#38510 = ORIENTED_EDGE ( 'NONE', *, *, #12381, .F. ) ;
#38511 = FACE_OUTER_BOUND ( 'NONE', #32656, .T. ) ;
#38512 = ORIENTED_EDGE ( 'NONE', *, *, #19134, .F. ) ;
#38513 = ORIENTED_EDGE ( 'NONE', *, *, #49310, .F. ) ;
#38514 = DIRECTION ( 'NONE',  ( 1.000000000000000000, 0.000000000000000000, 0.000000000000000000 ) ) ;
#38515 = PLANE ( 'NONE',  #41264 ) ;
#38516 = VERTEX_POINT ( 'NONE', #40815 ) ;
#38517 = CARTESIAN_POINT ( 'NONE',  ( -119.9999999999981668, 17.00000000000000000, 65.00000000000000000 ) ) ;
#38518 = DIRECTION ( 'NONE',  ( 0.000000000000000000, 0.000000000000000000, 1.000000000000000000 ) ) ;
#38519 = CARTESIAN_POINT ( 'NONE',  ( -6.695973446814940111, -1.750000000000024203, -79.18171244307201562 ) ) ;
#38520 = ORIENTED_EDGE ( 'NONE', *, *, #46363, .F. ) ;
#38521 = ORIENTED_EDGE ( 'NONE', *, *, #26308, .F. ) ;
#38522 = FACE_OUTER_BOUND ( 'NONE', #8252, .T. ) ;
#38523 = VECTOR ( 'NONE', #15911, 1000.000000000000000 ) ;
#38524 = CARTESIAN_POINT ( 'NONE',  ( 153.3040265531850537, 1.750000000000009992, 0.8182875569279768335 ) ) ;
#38525 = CIRCLE ( 'NONE', #33606, 4.000000000000003553 ) ;
#38526 = EDGE_CURVE ( 'NONE', #19896, #24656, #44138, .T. ) ;
#38527 = VECTOR ( 'NONE', #42951, 1000.000000000000000 ) ;
#38528 = VERTEX_POINT ( 'NONE', #29018 ) ;
#38529 = EDGE_CURVE ( 'NONE', #9147, #36272, #10275, .T. ) ;
#38530 = FACE_OUTER_BOUND ( 'NONE', #40214, .T. ) ;
#38531 = CARTESIAN_POINT ( 'NONE',  ( 0.2050626648100478400, -1.807624707196173519, 9.903764339332001398 ) ) ;
#38532 = ORIENTED_EDGE ( 'NONE', *, *, #39811, .T. ) ;
#38533 = CARTESIAN_POINT ( 'NONE',  ( 0.4098590526157686598, 3.751478160727024225, 9.865049507598756762 ) ) ;
#38534 = CIRCLE ( 'NONE', #33575, 10.00000000000000000 ) ;
#38535 = EDGE_CURVE ( 'NONE', #25164, #3012, #13612, .T. ) ;
#38536 = DIRECTION ( 'NONE',  ( -1.000000000000000000, 0.000000000000000000, 0.000000000000000000 ) ) ;
#38537 = VERTEX_POINT ( 'NONE', #13104 ) ;
#38538 = CARTESIAN_POINT ( 'NONE',  ( -1.286508520037554337, -0.4866366830703409141, 9.972175347158394487 ) ) ;
#38539 = EDGE_CURVE ( 'NONE', #21304, #41284, #22068, .T. ) ;
#38540 = CARTESIAN_POINT ( 'NONE',  ( -47.72109971266203132, -1.750000000000009548, -158.1565861772249377 ) ) ;
#38541 = CARTESIAN_POINT ( 'NONE',  ( 80.00000000000028422, 17.00000000000000000, -84.99999999999998579 ) ) ;
#38542 = EDGE_CURVE ( 'NONE', #38121, #28737, #9510, .T. ) ;
#38543 = AXIS2_PLACEMENT_3D ( 'NONE', #13628, #38009, #2825 ) ;
#38544 = DIRECTION ( 'NONE',  ( 0.000000000000000000, 0.000000000000000000, -1.000000000000000000 ) ) ;
#38545 = VERTEX_POINT ( 'NONE', #6172 ) ;
#38546 = DIRECTION ( 'NONE',  ( 0.000000000000000000, 0.000000000000000000, -1.000000000000000000 ) ) ;
#38547 = CARTESIAN_POINT ( 'NONE',  ( 339.9999999999999432, 183.0000000000000284, -344.0000000000001705 ) ) ;
#38548 = EDGE_CURVE ( 'NONE', #48491, #40717, #2074, .T. ) ;
#38549 = DIRECTION ( 'NONE',  ( -0.000000000000000000, -1.000000000000000000, -0.000000000000000000 ) ) ;
#38550 = VERTEX_POINT ( 'NONE', #5406 ) ;
#38551 = ORIENTED_EDGE ( 'NONE', *, *, #34914, .T. ) ;
#38552 = DIRECTION ( 'NONE',  ( 1.029731855339826380E-14, 1.000000000000000000, 1.702437461315276710E-17 ) ) ;
#38553 = CARTESIAN_POINT ( 'NONE',  ( -14.99999999999906919, 17.00000000000000000, -24.99999999999999289 ) ) ;
#38554 = DIRECTION ( 'NONE',  ( -1.000000000000000000, 0.000000000000000000, 0.000000000000000000 ) ) ;
#38555 = SURFACE_STYLE_USAGE ( .BOTH. , #3629 ) ;
#38556 = CARTESIAN_POINT ( 'NONE',  ( 135.0000000000006253, 17.00000000000000000, -54.99999999999999289 ) ) ;
#38557 = CARTESIAN_POINT ( 'NONE',  ( -166.6959734468149463, -1.750000000000010658, -119.1817124430720440 ) ) ;
#38558 = ORIENTED_EDGE ( 'NONE', *, *, #19874, .F. ) ;
#38559 = CARTESIAN_POINT ( 'NONE',  ( 155.0540265531850537, 2.143131898507880377E-16, 39.06828755692798438 ) ) ;
#38560 = FACE_OUTER_BOUND ( 'NONE', #22472, .T. ) ;
#38561 = CARTESIAN_POINT ( 'NONE',  ( 32.27890028733795447, -1.750000000000009548, -158.1565861772249377 ) ) ;
#38562 = AXIS2_PLACEMENT_3D ( 'NONE', #36646, #1471, #12752 ) ;
#38563 = AXIS2_PLACEMENT_3D ( 'NONE', #34158, #17958, #49729 ) ;
#38564 = DIRECTION ( 'NONE',  ( -0.000000000000000000, -0.000000000000000000, -1.000000000000000000 ) ) ;
#38565 = EDGE_LOOP ( 'NONE', ( #2319, #7742, #42840, #15776 ) ) ;
#38566 = CARTESIAN_POINT ( 'NONE',  ( 71.55402655318505367, -1.025126265847089213, 159.0682875569279418 ) ) ;
#38567 = CARTESIAN_POINT ( 'NONE',  ( -0.3862712429686889770, 1.188820645368940720, 9.972675548442463622 ) ) ;
#38568 = VERTEX_POINT ( 'NONE', #21062 ) ;
#38569 = AXIS2_PLACEMENT_3D ( 'NONE', #25582, #8112, #7600 ) ;
#38570 = CARTESIAN_POINT ( 'NONE',  ( -206.6959734468149463, 0.000000000000000000, 165.0000000000000000 ) ) ;
#38571 = CARTESIAN_POINT ( 'NONE',  ( 339.9999999999997726, -183.3431457505076878, 358.3431457505077447 ) ) ;
#38572 = VECTOR ( 'NONE', #23626, 1000.000000000000000 ) ;
#38573 = AXIS2_PLACEMENT_3D ( 'NONE', #40812, #37497, #44881 ) ;
#38574 = DIRECTION ( 'NONE',  ( 0.000000000000000000, 0.000000000000000000, 1.000000000000000000 ) ) ;
#38575 = ORIENTED_EDGE ( 'NONE', *, *, #5062, .F. ) ;
#38576 = EDGE_CURVE ( 'NONE', #21273, #46833, #44885, .T. ) ;
#38577 = FACE_OUTER_BOUND ( 'NONE', #19795, .T. ) ;
#38578 = DIRECTION ( 'NONE',  ( -1.000000000000000000, 0.000000000000000000, 0.000000000000000000 ) ) ;
#38579 = ORIENTED_EDGE ( 'NONE', *, *, #11580, .F. ) ;
#38580 = CARTESIAN_POINT ( 'NONE',  ( 14.29087950072012170, 9.652079258044652832, 8.727788335465566760 ) ) ;
#38581 = CARTESIAN_POINT ( 'NONE',  ( 35.05402655318504657, 2.143131898507880377E-16, 82.56828755692798438 ) ) ;
#38582 = CYLINDRICAL_SURFACE ( 'NONE', #22570, 1.750000000000001554 ) ;
#38583 = EDGE_LOOP ( 'NONE', ( #28299, #49366, #36914, #42809, #10668, #6323, #446, #35114, #21972, #38599, #1280, #13314, #42275, #15024, #22555 ) ) ;
#38584 = ORIENTED_EDGE ( 'NONE', *, *, #19903, .F. ) ;
#38585 = LINE ( 'NONE', #3660, #26745 ) ;
#38586 = CARTESIAN_POINT ( 'NONE',  ( 165.0000000000000284, 165.0000000000000000, 355.9999999999998863 ) ) ;
#38587 = ORIENTED_EDGE ( 'NONE', *, *, #9038, .T. ) ;
#38588 = ORIENTED_EDGE ( 'NONE', *, *, #25580, .T. ) ;
#38589 = CARTESIAN_POINT ( 'NONE',  ( 34.76907794179066258, -14.14424844080153498, -5.338708898921614932 ) ) ;
#38590 = CARTESIAN_POINT ( 'NONE',  ( 35.05402655318504657, 2.143131898507880377E-16, 42.56828755692798438 ) ) ;
#38591 = VERTEX_POINT ( 'NONE', #1575 ) ;
#38592 = CARTESIAN_POINT ( 'NONE',  ( -50.13037131770489907, -41.71198943095993172, 741.9425600500172777 ) ) ;
#38593 = EDGE_LOOP ( 'NONE', ( #44410, #16234, #45209, #12811 ) ) ;
#38594 = FACE_OUTER_BOUND ( 'NONE', #49283, .T. ) ;
#38595 = CARTESIAN_POINT ( 'NONE',  ( 194.3291528190321742, -1.750000000000009548, 81.84341382277507648 ) ) ;
#38596 = AXIS2_PLACEMENT_3D ( 'NONE', #43405, #19547, #23663 ) ;
#38597 = EDGE_CURVE ( 'NONE', #20258, #17953, #10432, .T. ) ;
#38598 = CARTESIAN_POINT ( 'NONE',  ( 9.281355226777661116, -3.722424633806168615, 0.000000000000000000 ) ) ;
#38599 = ORIENTED_EDGE ( 'NONE', *, *, #30941, .F. ) ;
#38600 = VERTEX_POINT ( 'NONE', #25678 ) ;
#38601 = ORIENTED_EDGE ( 'NONE', *, *, #11521, .F. ) ;
#38602 = CARTESIAN_POINT ( 'NONE',  ( -6.695973446814940111, 1.750000000000023315, 160.8182875569279702 ) ) ;
#38603 = ADVANCED_FACE ( 'NONE', ( #33387 ), #41321, .T. ) ;
#38604 = LINE ( 'NONE', #45987, #35741 ) ;
#38605 = CARTESIAN_POINT ( 'NONE',  ( 0.1188999517099294939, 1.297929763951737758, 9.961915419665734461 ) ) ;
#38606 = ORIENTED_EDGE ( 'NONE', *, *, #33733, .T. ) ;
#38607 = DIRECTION ( 'NONE',  ( 0.000000000000000000, 1.000000000000000000, -1.604368532695312981E-16 ) ) ;
#38608 = AXIS2_PLACEMENT_3D ( 'NONE', #50359, #3962, #46765 ) ;
#38609 = VERTEX_POINT ( 'NONE', #34391 ) ;
#38610 = DIRECTION ( 'NONE',  ( 0.000000000000000000, 0.000000000000000000, -1.000000000000000000 ) ) ;
#38611 = VERTEX_POINT ( 'NONE', #30795 ) ;
#38612 =( LENGTH_UNIT ( ) NAMED_UNIT ( * ) SI_UNIT ( .MILLI., .METRE. ) );
#38613 = DIRECTION ( 'NONE',  ( 0.000000000000000000, -0.000000000000000000, 1.000000000000000000 ) ) ;
#38614 = CARTESIAN_POINT ( 'NONE',  ( 7.129058724844953510, 15.30620660340485095, 9.178419661560148768 ) ) ;
#38615 = CARTESIAN_POINT ( 'NONE',  ( 210.0000000000000568, 2.143131898507881856E-16, 79.06828755692797017 ) ) ;
#38616 = VERTEX_POINT ( 'NONE', #11029 ) ;
#38617 = CARTESIAN_POINT ( 'NONE',  ( -1.072341519476054827, 1.326978504731037845, 9.912102921405034905 ) ) ;
#38618 = LINE ( 'NONE', #4657, #27327 ) ;
#38619 = CARTESIAN_POINT ( 'NONE',  ( 135.0000000000019043, 17.00000000000000000, 65.00000000000000000 ) ) ;
#38620 = DIRECTION ( 'NONE',  ( 0.000000000000000000, 0.000000000000000000, -1.000000000000000000 ) ) ;
#38621 =( BOUNDED_CURVE ( )  B_SPLINE_CURVE ( 3, ( #903, #21386, #32967, #40897 ),
 .UNSPECIFIED., .F., .F. ) 
 B_SPLINE_CURVE_WITH_KNOTS ( ( 4, 4 ),
 ( 1.570796326794896558, 3.141592653589793116 ),
 .UNSPECIFIED. ) 
 CURVE ( )  GEOMETRIC_REPRESENTATION_ITEM ( )  RATIONAL_B_SPLINE_CURVE ( ( 1.000000000000000000, 0.8047378541243649375, 0.8047378541243649375, 1.000000000000000000 ) ) 
 REPRESENTATION_ITEM ( '' )  );
#38622 = LINE ( 'NONE', #889, #7564 ) ;
#38623 = LINE ( 'NONE', #22696, #40929 ) ;
#38624 = ORIENTED_EDGE ( 'NONE', *, *, #30533, .F. ) ;
#38625 = CARTESIAN_POINT ( 'NONE',  ( 185.0000000000000000, -164.9999999999999432, 355.9999999999998863 ) ) ;
#38626 =( BOUNDED_CURVE ( )  B_SPLINE_CURVE ( 3, ( #44505, #11537, #3826, #252 ),
 .UNSPECIFIED., .F., .F. ) 
 B_SPLINE_CURVE_WITH_KNOTS ( ( 4, 4 ),
 ( 0.000000000000000000, 1.570796326794896780 ),
 .UNSPECIFIED. ) 
 CURVE ( )  GEOMETRIC_REPRESENTATION_ITEM ( )  RATIONAL_B_SPLINE_CURVE ( ( 1.000000000000000000, 0.8047378541243649375, 0.8047378541243649375, 1.000000000000000000 ) ) 
 REPRESENTATION_ITEM ( '' )  );
#38627 = CARTESIAN_POINT ( 'NONE',  ( 193.3040265531851105, 0.000000000000000000, 165.0000000000000000 ) ) ;
#38628 = EDGE_CURVE ( 'NONE', #38600, #44276, #22571, .T. ) ;
#38629 = VECTOR ( 'NONE', #31147, 1000.000000000000000 ) ;
#38630 = ORIENTED_EDGE ( 'NONE', *, *, #40096, .T. ) ;
#38631 = FACE_BOUND ( 'NONE', #39732, .T. ) ;
#38632 = MANIFOLD_SOLID_BREP ( 'Cut-Extrude1', #7272 ) ;
#38633 = CARTESIAN_POINT ( 'NONE',  ( 344.0000000000000000, -167.0000000000000853, -342.0000000000002842 ) ) ;
#38634 =( BOUNDED_CURVE ( )  B_SPLINE_CURVE ( 3, ( #44742, #37592, #33737, #9617 ),
 .UNSPECIFIED., .F., .F. ) 
 B_SPLINE_CURVE_WITH_KNOTS ( ( 4, 4 ),
 ( 1.570796326794896558, 3.141592653589793116 ),
 .UNSPECIFIED. ) 
 CURVE ( )  GEOMETRIC_REPRESENTATION_ITEM ( )  RATIONAL_B_SPLINE_CURVE ( ( 1.000000000000000000, 0.8047378541243649375, 0.8047378541243649375, 1.000000000000000000 ) ) 
 REPRESENTATION_ITEM ( '' )  );
#38635 = ORIENTED_EDGE ( 'NONE', *, *, #44322, .F. ) ;
#38636 = VECTOR ( 'NONE', #22264, 1000.000000000000000 ) ;
#38637 = ORIENTED_EDGE ( 'NONE', *, *, #40912, .T. ) ;
#38638 = CARTESIAN_POINT ( 'NONE',  ( 210.0000000000000568, 0.000000000000000000, -159.1817124430720298 ) ) ;
#38639 = CARTESIAN_POINT ( 'NONE',  ( -1.249999999999999778, 0.000000000000000000, -10.00000000000000000 ) ) ;
#38640 = ORIENTED_EDGE ( 'NONE', *, *, #43441, .T. ) ;
#38641 = ORIENTED_EDGE ( 'NONE', *, *, #42341, .T. ) ;
#38642 = CARTESIAN_POINT ( 'NONE',  ( -44.94597344681493922, 1.025126265847089657, -37.43171244307202272 ) ) ;
#38643 = CARTESIAN_POINT ( 'NONE',  ( -124.9459734468149321, -1.025126265847081219, -157.4317124430720582 ) ) ;
#38644 = LINE ( 'NONE', #3202, #26724 ) ;
#38645 = VERTEX_POINT ( 'NONE', #42570 ) ;
#38646 = VERTEX_POINT ( 'NONE', #14619 ) ;
#38647 = B_SPLINE_CURVE_WITH_KNOTS ( 'NONE', 3,
 ( #32693, #33217, #45206, #13437 ),
 .UNSPECIFIED., .F., .F.,
 ( 4, 4 ),
 ( 0.000000000000000000, 0.002368422649471297291 ),
 .UNSPECIFIED. ) ;
#38648 = ORIENTED_EDGE ( 'NONE', *, *, #21120, .F. ) ;
#38649 = CARTESIAN_POINT ( 'NONE',  ( -85.67084718096784002, 1.750000000000009548, 159.7931612910809065 ) ) ;
#38650 = ORIENTED_EDGE ( 'NONE', *, *, #49269, .F. ) ;
#38651 = CARTESIAN_POINT ( 'NONE',  ( -64.99999999999940314, 16.00000000000000000, -54.99999999999999289 ) ) ;
#38652 = CARTESIAN_POINT ( 'NONE',  ( 9.185112145816566098, 0.000000000000000000, 33.33601305720110020 ) ) ;
#38653 = ORIENTED_EDGE ( 'NONE', *, *, #9079, .T. ) ;
#38654 = ORIENTED_EDGE ( 'NONE', *, *, #48708, .F. ) ;
#38655 = FACE_OUTER_BOUND ( 'NONE', #47309, .T. ) ;
#38656 = EDGE_CURVE ( 'NONE', #8813, #6749, #3065, .T. ) ;
#38657 = CARTESIAN_POINT ( 'NONE',  ( -125.6708471809678542, -1.749999999999997113, -120.2068387089191219 ) ) ;
#38658 = VECTOR ( 'NONE', #11638, 1000.000000000000000 ) ;
#38659 = CYLINDRICAL_SURFACE ( 'NONE', #3560, 1.750000000000010214 ) ;
#38660 = ORIENTED_EDGE ( 'NONE', *, *, #8649, .T. ) ;
#38661 = VERTEX_POINT ( 'NONE', #41820 ) ;
#38662 = LINE ( 'NONE', #30710, #11880 ) ;
#38663 = CYLINDRICAL_SURFACE ( 'NONE', #30123, 1.750000000000015543 ) ;
#38664 = CARTESIAN_POINT ( 'NONE',  ( 360.0000000000001137, 181.0000000000000284, 355.9999999999998295 ) ) ;
#38665 = VECTOR ( 'NONE', #33938, 1000.000000000000000 ) ;
#38666 = CARTESIAN_POINT ( 'NONE',  ( 27.33593271309472073, -41.94268121623323964, -9.367992836599954742 ) ) ;
#38667 = ORIENTED_EDGE ( 'NONE', *, *, #42744, .F. ) ;
#38668 = CARTESIAN_POINT ( 'NONE',  ( -215.0000000000000568, -165.7692307692307452, 496.1538461538461888 ) ) ;
#38669 = EDGE_CURVE ( 'NONE', #43847, #45334, #17909, .T. ) ;
#38670 = DIRECTION ( 'NONE',  ( 1.000000000000000000, 0.000000000000000000, -2.312964634635843537E-16 ) ) ;
#38671 = DIRECTION ( 'NONE',  ( -3.364279341222519273E-16, 0.7071067811865474617, -0.7071067811865476838 ) ) ;
#38672 = CIRCLE ( 'NONE', #7537, 2.000000000000001776 ) ;
#38673 = DIRECTION ( 'NONE',  ( 1.000000000000000000, 0.000000000000000000, 0.000000000000000000 ) ) ;
#38674 = ADVANCED_FACE ( 'NONE', ( #26931 ), #46130, .T. ) ;
#38675 = DIRECTION ( 'NONE',  ( -0.000000000000000000, -0.000000000000000000, -1.000000000000000000 ) ) ;
#38676 = DIRECTION ( 'NONE',  ( -3.172065784643302499E-16, -1.000000000000000000, 2.537652627714642000E-15 ) ) ;
#38677 = ORIENTED_EDGE ( 'NONE', *, *, #44014, .T. ) ;
#38678 = CARTESIAN_POINT ( 'NONE',  ( -0.4166666666666669072, 0.000000000000000000, 10.00000000000000000 ) ) ;
#38679 = CARTESIAN_POINT ( 'NONE',  ( -49.67735855322972327, 8.912210285362091255, 8.356839323120299312 ) ) ;
#38680 = EDGE_CURVE ( 'NONE', #9263, #35257, #3317, .T. ) ;
#38681 = EDGE_CURVE ( 'NONE', #48612, #34716, #9094, .T. ) ;
#38683 = VERTEX_POINT ( 'NONE', #34153 ) ;
#38682 = EDGE_CURVE ( 'NONE', #40254, #37254, #18707, .T. ) ;
#38684 = LINE ( 'NONE', #18401, #11725 ) ;
#38685 = ADVANCED_FACE ( 'NONE', ( #18207 ), #33886, .T. ) ;
#38686 = CARTESIAN_POINT ( 'NONE',  ( 181.0000000000000000, -256.4999999999999432, -339.9999999999998863 ) ) ;
#38687 = ORIENTED_EDGE ( 'NONE', *, *, #4500, .T. ) ;
#38688 = DIRECTION ( 'NONE',  ( 0.000000000000000000, 0.000000000000000000, 1.000000000000000000 ) ) ;
#38689 = DIRECTION ( 'NONE',  ( 0.000000000000000000, 0.000000000000000000, 1.000000000000000000 ) ) ;
#38690 = FACE_OUTER_BOUND ( 'NONE', #23906, .T. ) ;
#38691 = VECTOR ( 'NONE', #36727, 1000.000000000000000 ) ;
#38692 = ORIENTED_EDGE ( 'NONE', *, *, #32612, .T. ) ;
#38693 = DIRECTION ( 'NONE',  ( -1.000000000000000000, -0.000000000000000000, -0.000000000000000000 ) ) ;
#38694 = ORIENTED_EDGE ( 'NONE', *, *, #22763, .F. ) ;
#38695 = ORIENTED_EDGE ( 'NONE', *, *, #36352, .T. ) ;
#38696 = DIRECTION ( 'NONE',  ( 0.000000000000000000, 0.000000000000000000, 1.000000000000000000 ) ) ;
#38697 = ORIENTED_EDGE ( 'NONE', *, *, #8275, .F. ) ;
#38698 = CYLINDRICAL_SURFACE ( 'NONE', #45855, 2.000000000000001776 ) ;
#38699 = CARTESIAN_POINT ( 'NONE',  ( -0.3862712429686809279, -1.188820645368943163, -10.00000000000000000 ) ) ;
#38700 = UNCERTAINTY_MEASURE_WITH_UNIT (LENGTH_MEASURE( 1.000000000000000082E-05 ), #20976, 'distance_accuracy_value', 'NONE');
#38701 = LINE ( 'NONE', #4488, #34353 ) ;
#38702 = DIRECTION ( 'NONE',  ( -0.000000000000000000, -0.000000000000000000, -1.000000000000000000 ) ) ;
#38703 = EDGE_CURVE ( 'NONE', #2781, #50360, #7455, .T. ) ;
#38704 = EDGE_LOOP ( 'NONE', ( #2712, #25131, #9500, #27756, #12995 ) ) ;
#38705 = DIRECTION ( 'NONE',  ( -1.000000000000000000, 0.000000000000000000, 0.000000000000000000 ) ) ;
#38706 = DIRECTION ( 'NONE',  ( -0.000000000000000000, -1.000000000000000000, -0.000000000000000000 ) ) ;
#38707 = CARTESIAN_POINT ( 'NONE',  ( 154.1026953830863420, -98.56198943095992604, -17.65743994998277699 ) ) ;
#38708 = EDGE_CURVE ( 'NONE', #9008, #11165, #33821, .T. ) ;
#38709 = VERTEX_POINT ( 'NONE', #40013 ) ;
#38710 = EDGE_CURVE ( 'NONE', #16028, #21378, #8716, .T. ) ;
#38711 = CARTESIAN_POINT ( 'NONE',  ( 0.000000000000000000, -33.89193117067290473, 910.0000000000000000 ) ) ;
#38712 = VERTEX_POINT ( 'NONE', #11794 ) ;
#38713 = EDGE_LOOP ( 'NONE', ( #26211, #3370, #36652 ) ) ;
#38714 = EDGE_LOOP ( 'NONE', ( #32970, #24235, #36885, #30738 ) ) ;
#38715 = CARTESIAN_POINT ( 'NONE',  ( -1.288422560825909224, 0.1812466941682708832, 9.986087673579197244 ) ) ;
#38716 = ADVANCED_FACE ( 'NONE', ( #20247 ), #12052, .T. ) ;
#38717 = CIRCLE ( 'NONE', #5108, 3.749999999999975575 ) ;
#38718 = FACE_OUTER_BOUND ( 'NONE', #1223, .T. ) ;
#38719 = ORIENTED_EDGE ( 'NONE', *, *, #35253, .T. ) ;
#38720 = EDGE_CURVE ( 'NONE', #24051, #39174, #4311, .T. ) ;
#38721 = CARTESIAN_POINT ( 'NONE',  ( -164.9459734468149463, -1.025126265847089435, -77.43171244307200141 ) ) ;
#38722 = LINE ( 'NONE', #49704, #17239 ) ;
#38723 = FACE_BOUND ( 'NONE', #19668, .T. ) ;
#38724 = DIRECTION ( 'NONE',  ( -1.000000000000000000, 0.000000000000000000, 0.000000000000000000 ) ) ;
#38725 = DIRECTION ( 'NONE',  ( -1.000000000000000000, -0.000000000000000000, -0.000000000000000000 ) ) ;
#38726 = CARTESIAN_POINT ( 'NONE',  ( -166.6959734468149463, -1.750000000000010658, 80.81828755692798438 ) ) ;
#38727 = CARTESIAN_POINT ( 'NONE',  ( 33.30402655318503946, -1.750000000000010658, 120.8182875569279702 ) ) ;
#38728 = CARTESIAN_POINT ( 'NONE',  ( 185.0000000000000568, 165.0000000000000000, 343.9999999999998863 ) ) ;
#38729 = VECTOR ( 'NONE', #987, 1000.000000000000000 ) ;
#38730 = PLANE ( 'NONE',  #47900 ) ;
#38731 = DIRECTION ( 'NONE',  ( 0.000000000000000000, 0.000000000000000000, 1.000000000000000000 ) ) ;
#38732 = ORIENTED_EDGE ( 'NONE', *, *, #42487, .F. ) ;
#38733 = FACE_OUTER_BOUND ( 'NONE', #41266, .T. ) ;
#38734 = PLANE ( 'NONE',  #7883 ) ;
#38735 = VECTOR ( 'NONE', #25474, 1000.000000000000000 ) ;
#38736 = ADVANCED_FACE ( 'NONE', ( #4 ), #16393, .F. ) ;
#38737 = CARTESIAN_POINT ( 'NONE',  ( 356.0000000000000000, 174.9999999999996589, -344.0000000000002842 ) ) ;
#38738 = FACE_OUTER_BOUND ( 'NONE', #22523, .T. ) ;
#38739 = ORIENTED_EDGE ( 'NONE', *, *, #25244, .F. ) ;
#38740 = CARTESIAN_POINT ( 'NONE',  ( -7.749480817862350435, -14.85497772329513211, 9.403735324607438884 ) ) ;
#38741 = DIRECTION ( 'NONE',  ( -1.000000000000000000, 0.000000000000000000, 0.000000000000000000 ) ) ;
#38742 = CARTESIAN_POINT ( 'NONE',  ( 0.3862712429686727678, 1.188820645368945605, -10.00000000000000000 ) ) ;
#38743 = CARTESIAN_POINT ( 'NONE',  ( 5.923309489234873659, -5.336940131180849534, 8.131516293641283255E-16 ) ) ;
#38744 = EDGE_CURVE ( 'NONE', #25569, #35217, #23970, .T. ) ;
#38745 = LINE ( 'NONE', #35415, #19727 ) ;
#38746 = ADVANCED_BREP_SHAPE_REPRESENTATION ( '', ( #22493, #39637, #39816, #5102, #38125, #22914, #39303, #39060, #38377, #4445, #21989, #21395, #39561, #22072, #21149, #21477, #5021, #22244, #38306, #4281, #21652, #5610, #45486 ), #41416 ) ;
#38748 = ORIENTED_EDGE ( 'NONE', *, *, #46586, .F. ) ;
#38747 = ADVANCED_FACE ( 'NONE', ( #511 ), #28461, .T. ) ;
#38749 = DIRECTION ( 'NONE',  ( -1.000000000000000000, 0.000000000000000000, 0.000000000000000000 ) ) ;
#38750 = ADVANCED_FACE ( 'NONE', ( #751 ), #36162, .T. ) ;
#38751 = EDGE_LOOP ( 'NONE', ( #46097, #45034, #13866, #5825, #2089, #8620 ) ) ;
#38752 = VERTEX_POINT ( 'NONE', #16152 ) ;
#38753 = EDGE_CURVE ( 'NONE', #4361, #11473, #19740, .T. ) ;
#38754 = CARTESIAN_POINT ( 'NONE',  ( -14.99999999999970868, 17.00000000000000000, -84.99999999999998579 ) ) ;
#38755 = FACE_BOUND ( 'NONE', #27855, .T. ) ;
#38756 = AXIS2_PLACEMENT_3D ( 'NONE', #2103, #5937, #21586 ) ;
#38757 = EDGE_CURVE ( 'NONE', #30619, #42504, #261, .T. ) ;
#38758 = ORIENTED_EDGE ( 'NONE', *, *, #17761, .F. ) ;
#38759 = CARTESIAN_POINT ( 'NONE',  ( 193.3040265531851105, 0.000000000000000000, 165.0000000000000000 ) ) ;
#38760 = ORIENTED_EDGE ( 'NONE', *, *, #43705, .T. ) ;
#38761 = ORIENTED_EDGE ( 'NONE', *, *, #48777, .T. ) ;
#38762 = PLANE ( 'NONE',  #49107 ) ;
#38763 = FACE_OUTER_BOUND ( 'NONE', #42608, .T. ) ;
#38764 = ORIENTED_EDGE ( 'NONE', *, *, #29658, .T. ) ;
#38765 = LINE ( 'NONE', #38517, #845 ) ;
#38766 = CARTESIAN_POINT ( 'NONE',  ( -64.99999999999940314, 17.00000000000000000, -54.99999999999999289 ) ) ;
#38767 = VECTOR ( 'NONE', #32608, 1000.000000000000000 ) ;
#38768 = CARTESIAN_POINT ( 'NONE',  ( 167.0000000000000284, 165.0000000000000000, 355.9999999999998863 ) ) ;
#38769 = ORIENTED_EDGE ( 'NONE', *, *, #44331, .T. ) ;
#38770 = VERTEX_POINT ( 'NONE', #43588 ) ;
#38771 = CARTESIAN_POINT ( 'NONE',  ( -33.26055721649984775, -17.33465289285453181, 8.506357886886743103 ) ) ;
#38772 = PRESENTATION_LAYER_ASSIGNMENT (  '', '', ( #32214 ) ) ;
#38773 = FACE_OUTER_BOUND ( 'NONE', #901, .T. ) ;
#38774 = EDGE_LOOP ( 'NONE', ( #3455, #39766, #10730, #82, #24974, #925 ) ) ;
#38775 = EDGE_CURVE ( 'NONE', #38770, #12440, #43839, .T. ) ;
#38776 = CARTESIAN_POINT ( 'NONE',  ( 181.0000000000000568, 165.0000000000000000, 355.9999999999998863 ) ) ;
#38777 = CARTESIAN_POINT ( 'NONE',  ( -7.721099712662037540, 1.750000000000023981, -80.20683870891910772 ) ) ;
#38778 = ORIENTED_EDGE ( 'NONE', *, *, #15788, .T. ) ;
#38779 = CYLINDRICAL_SURFACE ( 'NONE', #30312, 4.000000000000003553 ) ;
#38780 =( BOUNDED_CURVE ( )  B_SPLINE_CURVE ( 3, ( #40410, #4744, #48050, #5247 ),
 .UNSPECIFIED., .F., .F. ) 
 B_SPLINE_CURVE_WITH_KNOTS ( ( 4, 4 ),
 ( 1.570796326794896558, 3.141592653589793116 ),
 .UNSPECIFIED. ) 
 CURVE ( )  GEOMETRIC_REPRESENTATION_ITEM ( )  RATIONAL_B_SPLINE_CURVE ( ( 1.000000000000000000, 0.8047378541243649375, 0.8047378541243649375, 1.000000000000000000 ) ) 
 REPRESENTATION_ITEM ( '' )  );
#38781 = DIRECTION ( 'NONE',  ( -1.000000000000000000, -0.000000000000000000, -0.000000000000000000 ) ) ;
#38782 = B_SPLINE_SURFACE_WITH_KNOTS ( 'NONE', 3, 3, ( 
 ( #29555, #6456, #13396, #2359 ),
 ( #9305, #37784, #2598, #24967 ),
 ( #5448, #36782, #29060, #48763 ),
 ( #44679, #41109, #44921, #9559 ) ),
 .UNSPECIFIED., .F., .F., .F.,
 ( 4, 4 ),
 ( 4, 4 ),
 ( 0.000000000000000000, 1.000000000000000000 ),
 ( 0.000000000000000000, 1.000000000000000000 ),
 .UNSPECIFIED. ) ;
#38783 = PRODUCT_DEFINITION ( 'UNKNOWN', '', #38952, #24211 ) ;
#38784 = ORIENTED_EDGE ( 'NONE', *, *, #12729, .T. ) ;
#38785 = DIRECTION ( 'NONE',  ( -3.172065784643302499E-16, -1.000000000000000000, 2.537652627714642000E-15 ) ) ;
#38786 = CARTESIAN_POINT ( 'NONE',  ( -208.4459734468149463, 0.000000000000000000, 42.56828755692798438 ) ) ;
#38787 = CARTESIAN_POINT ( 'NONE',  ( 210.0000000000000568, 2.143131898507881856E-16, -80.93171244307202983 ) ) ;
#38788 = LINE ( 'NONE', #10551, #41942 ) ;
#38789 = ORIENTED_EDGE ( 'NONE', *, *, #47177, .T. ) ;
#38790 = CARTESIAN_POINT ( 'NONE',  ( 17.23491422248386584, -0.5912720620000816441, 8.727788335465566760 ) ) ;
#38791 =( NAMED_UNIT ( * ) SI_UNIT ( $, .STERADIAN. ) SOLID_ANGLE_UNIT ( ) );
#38792 = EDGE_CURVE ( 'NONE', #11587, #23937, #4831, .T. ) ;
#38793 = CARTESIAN_POINT ( 'NONE',  ( 45.42829307628542779, 21.98948915213303579, 8.356839323120299312 ) ) ;
#38794 = ORIENTED_EDGE ( 'NONE', *, *, #28338, .F. ) ;
#38795 = ORIENTED_EDGE ( 'NONE', *, *, #40602, .T. ) ;
#38796 = CARTESIAN_POINT ( 'NONE',  ( 871.4995338189595486, 1204.403237050712278, 1923.486414963447260 ) ) ;
#38797 = CARTESIAN_POINT ( 'NONE',  ( 164.9999999999999716, -174.9999999999999716, -340.0000000000001137 ) ) ;
#38798 = FACE_OUTER_BOUND ( 'NONE', #11259, .T. ) ;
#38799 = MANIFOLD_SOLID_BREP ( 'Boss-Extrude5', #25291 ) ;
#38800 = AXIS2_PLACEMENT_3D ( 'NONE', #30157, #13990, #37878 ) ;
#38801 = CARTESIAN_POINT ( 'NONE',  ( -22.82242230425432439, 2.683863964738837371, 230.0000000000000000 ) ) ;
#38802 = EDGE_CURVE ( 'NONE', #49333, #5291, #33568, .T. ) ;
#38803 = DIRECTION ( 'NONE',  ( 0.000000000000000000, 0.000000000000000000, -1.000000000000000000 ) ) ;
#38804 = VERTEX_POINT ( 'NONE', #31813 ) ;
#38805 = LINE ( 'NONE', #50281, #13254 ) ;
#38806 = VECTOR ( 'NONE', #48583, 1000.000000000000000 ) ;
#38807 = CARTESIAN_POINT ( 'NONE',  ( -50.11058929355266400, 7.578863168071933387, 7.455576670931136185 ) ) ;
#38808 = CARTESIAN_POINT ( 'NONE',  ( 4.376737514451251698, -37.28021197136517628, 1.982731392810406668 ) ) ;
#38809 = VECTOR ( 'NONE', #44089, 1000.000000000000000 ) ;
#38810 = CARTESIAN_POINT ( 'NONE',  ( 191.5540265531850537, -1.025126265847089879, -117.4317124430720156 ) ) ;
#38811 = EDGE_CURVE ( 'NONE', #12974, #10514, #29708, .T. ) ;
#38812 =( NAMED_UNIT ( * ) PLANE_ANGLE_UNIT ( ) SI_UNIT ( $, .RADIAN. ) );
#38813 = EDGE_CURVE ( 'NONE', #18558, #3258, #29455, .T. ) ;
#38814 = ORIENTED_EDGE ( 'NONE', *, *, #21249, .F. ) ;
#38815 = DIRECTION ( 'NONE',  ( 1.000000000000000000, 0.000000000000000000, -0.000000000000000000 ) ) ;
#38816 = CARTESIAN_POINT ( 'NONE',  ( 169.0000000000000000, -168.9999999999999432, -115.0000000000001847 ) ) ;
#38817 = EDGE_LOOP ( 'NONE', ( #3006, #14003, #9877, #9793, #15212, #13166 ) ) ;
#38818 = CARTESIAN_POINT ( 'NONE',  ( 79.99999999999997158, 16.00000000000000000, -90.00000000000000000 ) ) ;
#38819 = DIRECTION ( 'NONE',  ( 0.000000000000000000, 0.000000000000000000, 1.000000000000000000 ) ) ;
#38820 = EDGE_CURVE ( 'NONE', #4352, #29552, #21251, .T. ) ;
#38821 = LINE ( 'NONE', #4167, #43563 ) ;
#38822 = EDGE_LOOP ( 'NONE', ( #32469, #44443, #23943, #41774, #8585, #1854 ) ) ;
#38823 = EDGE_CURVE ( 'NONE', #6064, #13712, #1603, .T. ) ;
#38824 = ADVANCED_FACE ( 'NONE', ( #5853 ), #48403, .T. ) ;
#38825 = AXIS2_PLACEMENT_3D ( 'NONE', #13208, #9618, #16564 ) ;
#38826 = FACE_OUTER_BOUND ( 'NONE', #18789, .T. ) ;
#38827 = CARTESIAN_POINT ( 'NONE',  ( -165.3973046169136012, -62.56198943095993315, -17.65743994998275213 ) ) ;
#38828 = EDGE_LOOP ( 'NONE', ( #3282, #17100, #28704, #29707 ) ) ;
#38829 = CARTESIAN_POINT ( 'NONE',  ( -8.813458710706198573, -4.724716452304520864, 0.000000000000000000 ) ) ;
#38830 = CARTESIAN_POINT ( 'NONE',  ( 16.52264463346132572, -2.779753662172757878, 9.403735324607438884 ) ) ;
#38831 = UNCERTAINTY_MEASURE_WITH_UNIT (LENGTH_MEASURE( 1.000000000000000082E-05 ), #2367, 'distance_accuracy_value', 'NONE');
#38832 = LINE ( 'NONE', #33955, #2112 ) ;
#38833 = ADVANCED_FACE ( 'NONE', ( #13787 ), #40509, .F. ) ;
#38834 = ORIENTED_EDGE ( 'NONE', *, *, #1747, .T. ) ;
#38835 = ORIENTED_EDGE ( 'NONE', *, *, #46926, .F. ) ;
#38836 = B_SPLINE_CURVE_WITH_KNOTS ( 'NONE', 3,
 ( #15440, #11338, #31096, #42624 ),
 .UNSPECIFIED., .F., .F.,
 ( 4, 4 ),
 ( 0.000000000000000000, 0.2637263876330694368 ),
 .UNSPECIFIED. ) ;
#38837 = CARTESIAN_POINT ( 'NONE',  ( 55.00000000000002132, -52.50000000000000711, 5.000000000000000000 ) ) ;
#38838 = CARTESIAN_POINT ( 'NONE',  ( 112.2789002873379758, -1.749999999999996891, -78.15658617722492352 ) ) ;
#38839 = ORIENTED_EDGE ( 'NONE', *, *, #49621, .F. ) ;
#38840 = VERTEX_POINT ( 'NONE', #5084 ) ;
#38841 = LINE ( 'NONE', #19560, #3656 ) ;
#38842 = CARTESIAN_POINT ( 'NONE',  ( 0.000000000000000000, 184.8000000000000114, -359.8000000000002387 ) ) ;
#38843 = VECTOR ( 'NONE', #27773, 1000.000000000000000 ) ;
#38844 = CARTESIAN_POINT ( 'NONE',  ( 33.30402655318503946, 1.750000000000010214, 40.81828755692798438 ) ) ;
#38845 = ORIENTED_EDGE ( 'NONE', *, *, #26570, .T. ) ;
#38846 = DIRECTION ( 'NONE',  ( 0.000000000000000000, -0.000000000000000000, -1.000000000000000000 ) ) ;
#38847 = VECTOR ( 'NONE', #3308, 1000.000000000000000 ) ;
#38848 = ORIENTED_EDGE ( 'NONE', *, *, #45832, .T. ) ;
#38849 = FACE_OUTER_BOUND ( 'NONE', #37746, .T. ) ;
#38850 = CARTESIAN_POINT ( 'NONE',  ( 0.000000000000000000, 183.0000000000000284, 343.9999999999997726 ) ) ;
#38851 = VECTOR ( 'NONE', #33124, 1000.000000000000000 ) ;
#38852 = CARTESIAN_POINT ( 'NONE',  ( 1.066995270233474624, -33.23888904628638841, -3.760136334089591248 ) ) ;
#38853 = ORIENTED_EDGE ( 'NONE', *, *, #30351, .T. ) ;
#38854 = ORIENTED_EDGE ( 'NONE', *, *, #33362, .F. ) ;
#38855 = EDGE_LOOP ( 'NONE', ( #17916, #22340 ) ) ;
#38856 = LINE ( 'NONE', #43434, #45933 ) ;
#38857 = CARTESIAN_POINT ( 'NONE',  ( -48.98697415750977058, -11.03699497439218291, -8.016098858316205167 ) ) ;
#38858 = EDGE_LOOP ( 'NONE', ( #46288, #7667, #47601, #26379, #43634, #998 ) ) ;
#38859 = DIRECTION ( 'NONE',  ( 0.000000000000000000, 0.000000000000000000, -1.000000000000000000 ) ) ;
#38860 = VERTEX_POINT ( 'NONE', #25111 ) ;
#38861 = EDGE_CURVE ( 'NONE', #47807, #31952, #17473, .T. ) ;
#38862 = CARTESIAN_POINT ( 'NONE',  ( -165.6708471809677974, 1.750000000000009548, 41.84341382277508359 ) ) ;
#38863 = EDGE_LOOP ( 'NONE', ( #22149, #3001, #32030, #38132, #31350, #19031 ) ) ;
#38864 = DIRECTION ( 'NONE',  ( -0.000000000000000000, -1.000000000000000000, -0.000000000000000000 ) ) ;
#38865 = CARTESIAN_POINT ( 'NONE',  ( -86.69597344681494633, -1.750000000000010658, 120.8182875569279702 ) ) ;
#38866 = DIRECTION ( 'NONE',  ( 1.000000000000000000, 0.000000000000000000, 0.000000000000000000 ) ) ;
#38867 = AXIS2_PLACEMENT_3D ( 'NONE', #990, #9935, #24586 ) ;
#38868 =( BOUNDED_CURVE ( )  B_SPLINE_CURVE ( 3, ( #41406, #29860, #38335, #41658 ),
 .UNSPECIFIED., .F., .F. ) 
 B_SPLINE_CURVE_WITH_KNOTS ( ( 4, 4 ),
 ( 0.000000000000000000, 1.570796326794896558 ),
 .UNSPECIFIED. ) 
 CURVE ( )  GEOMETRIC_REPRESENTATION_ITEM ( )  RATIONAL_B_SPLINE_CURVE ( ( 1.000000000000000000, 0.8047378541243649375, 0.8047378541243649375, 1.000000000000000000 ) ) 
 REPRESENTATION_ITEM ( '' )  );
#38869 = DIRECTION ( 'NONE',  ( -0.000000000000000000, -0.000000000000000000, -1.000000000000000000 ) ) ;
#38870 = VERTEX_POINT ( 'NONE', #36424 ) ;
#38871 = ORIENTED_EDGE ( 'NONE', *, *, #1385, .F. ) ;
#38872 = CARTESIAN_POINT ( 'NONE',  ( 153.2026953830863647, -97.66198943095992036, -17.65743994998277699 ) ) ;
#38873 = DIRECTION ( 'NONE',  ( -0.7233555441435720601, 0.6904757466825006684, -0.000000000000000000 ) ) ;
#38874 = CARTESIAN_POINT ( 'NONE',  ( 28.97821631107911600, 35.56709536735927912, -9.367992836599951190 ) ) ;
#38875 = DIRECTION ( 'NONE',  ( 0.000000000000000000, 0.000000000000000000, 1.000000000000000000 ) ) ;
#38876 = EDGE_CURVE ( 'NONE', #16166, #38061, #33673, .T. ) ;
#38877 = LINE ( 'NONE', #46261, #32989 ) ;
#38878 = EDGE_CURVE ( 'NONE', #26946, #8841, #17890, .T. ) ;
#38879 = AXIS2_PLACEMENT_3D ( 'NONE', #43857, #43108, #35693 ) ;
#38880 = VECTOR ( 'NONE', #1964, 1000.000000000000000 ) ;
#38881 = CYLINDRICAL_SURFACE ( 'NONE', #36860, 4.000000000000003553 ) ;
#38882 = VERTEX_POINT ( 'NONE', #6103 ) ;
#38883 = VECTOR ( 'NONE', #21319, 1000.000000000000000 ) ;
#38884 = CARTESIAN_POINT ( 'NONE',  ( -164.9459734468149463, 1.025126265847089213, -0.9317124430720324924 ) ) ;
#38885 = DIRECTION ( 'NONE',  ( 0.5038710255240862468, 0.000000000000000000, 0.8637789008984334549 ) ) ;
#38886 = ADVANCED_FACE ( 'NONE', ( #28950 ), #16911, .T. ) ;
#38887 = ADVANCED_FACE ( 'NONE', ( #28705 ), #17402, .T. ) ;
#38888 = ORIENTED_EDGE ( 'NONE', *, *, #23459, .F. ) ;
#38889 = CARTESIAN_POINT ( 'NONE',  ( -164.9459734468149463, 2.143131898507880377E-16, 42.56828755692798438 ) ) ;
#38890 = CARTESIAN_POINT ( 'NONE',  ( -126.6959734468149321, -1.749999999999997335, 120.8182875569279702 ) ) ;
#38891 = EDGE_CURVE ( 'NONE', #25713, #36323, #19568, .T. ) ;
#38892 = CARTESIAN_POINT ( 'NONE',  ( -208.1473046169136580, 160.1880105690400171, 472.8425600500171981 ) ) ;
#38893 = VERTEX_POINT ( 'NONE', #44563 ) ;
#38894 = PRODUCT_DEFINITION_SHAPE ( 'NONE', 'NONE',  #50727 ) ;
#38895 = ORIENTED_EDGE ( 'NONE', *, *, #47586, .T. ) ;
#38896 = CARTESIAN_POINT ( 'NONE',  ( -208.4459734468149463, 0.000000000000000000, 82.56828755692798438 ) ) ;
#38897 = CARTESIAN_POINT ( 'NONE',  ( 7.576114424932982594, -33.14742743729794938, 7.906207997025717304 ) ) ;
#38898 = VECTOR ( 'NONE', #3630, 1000.000000000000000 ) ;
#38899 = ORIENTED_EDGE ( 'NONE', *, *, #39100, .F. ) ;
#38900 = EDGE_LOOP ( 'NONE', ( #47217, #37818, #22928, #12115 ) ) ;
#38901 = CARTESIAN_POINT ( 'NONE',  ( -9.281355226777547429, 3.722424633806451943, 0.000000000000000000 ) ) ;
#38902 = CARTESIAN_POINT ( 'NONE',  ( -14.49999999999999822, 12.98684210526315930, 19.37312575500899925 ) ) ;
#38903 = ORIENTED_EDGE ( 'NONE', *, *, #9534, .F. ) ;
#38904 = VECTOR ( 'NONE', #2800, 1000.000000000000000 ) ;
#38905 = ORIENTED_EDGE ( 'NONE', *, *, #1792, .F. ) ;
#38906 = VERTEX_POINT ( 'NONE', #30730 ) ;
#38907 = CARTESIAN_POINT ( 'NONE',  ( 191.5540265531850537, -1.025126265847089657, -37.43171244307202272 ) ) ;
#38908 = DIRECTION ( 'NONE',  ( 1.000000000000000000, 6.938893903907233308E-16, 0.000000000000000000 ) ) ;
#38909 = ORIENTED_EDGE ( 'NONE', *, *, #38720, .T. ) ;
#38910 = CARTESIAN_POINT ( 'NONE',  ( 356.0000000000006253, 167.0000000000000000, 341.9999999999998863 ) ) ;
#38911 = DIRECTION ( 'NONE',  ( -1.000000000000000000, 0.000000000000000000, 0.000000000000000000 ) ) ;
#38912 = CARTESIAN_POINT ( 'NONE',  ( 210.0000000000000568, 0.000000000000000000, 2.568287556927987048 ) ) ;
#38913 = EDGE_LOOP ( 'NONE', ( #48029, #35249, #22273, #41467 ) ) ;
#38914 = ORIENTED_EDGE ( 'NONE', *, *, #8874, .F. ) ;
#38915 = DIRECTION ( 'NONE',  ( -1.000000000000000000, 0.000000000000000000, 0.000000000000000000 ) ) ;
#38916 = PRESENTATION_STYLE_ASSIGNMENT (( #23235 ) ) ;
#38917 = LINE ( 'NONE', #31213, #22432 ) ;
#38918 = UNCERTAINTY_MEASURE_WITH_UNIT (LENGTH_MEASURE( 1.000000000000000082E-05 ), #13172, 'distance_accuracy_value', 'NONE');
#38919 = ORIENTED_EDGE ( 'NONE', *, *, #18111, .F. ) ;
#38920 = ORIENTED_EDGE ( 'NONE', *, *, #24583, .F. ) ;
#38921 = AXIS2_PLACEMENT_3D ( 'NONE', #45802, #38164, #21984 ) ;
#38922 = EDGE_CURVE ( 'NONE', #32533, #42729, #29969, .T. ) ;
#38923 = CARTESIAN_POINT ( 'NONE',  ( 21.24469349090191983, 33.89193117067290473, 910.0000000000000000 ) ) ;
#38924 = CARTESIAN_POINT ( 'NONE',  ( -164.9459734468149463, 2.143131898507880377E-16, -80.93171244307201562 ) ) ;
#38925 = ORIENTED_EDGE ( 'NONE', *, *, #25798, .F. ) ;
#38926 =( BOUNDED_CURVE ( )  B_SPLINE_CURVE ( 3, ( #16277, #47538, #12418, #28076 ),
 .UNSPECIFIED., .F., .F. ) 
 B_SPLINE_CURVE_WITH_KNOTS ( ( 4, 4 ),
 ( 4.712388980384689674, 6.283185307179586232 ),
 .UNSPECIFIED. ) 
 CURVE ( )  GEOMETRIC_REPRESENTATION_ITEM ( )  RATIONAL_B_SPLINE_CURVE ( ( 1.000000000000000000, 0.8047378541243649375, 0.8047378541243649375, 1.000000000000000000 ) ) 
 REPRESENTATION_ITEM ( '' )  );
#38927 = FACE_OUTER_BOUND ( 'NONE', #36476, .T. ) ;
#38928 = DIRECTION ( 'NONE',  ( -0.000000000000000000, -0.000000000000000000, -1.000000000000000000 ) ) ;
#38929 = LINE ( 'NONE', #4010, #17114 ) ;
#38930 = CARTESIAN_POINT ( 'NONE',  ( -166.6959734468149463, -1.750000000000010658, 80.81828755692798438 ) ) ;
#38931 = ORIENTED_EDGE ( 'NONE', *, *, #29142, .T. ) ;
#38932 = CARTESIAN_POINT ( 'NONE',  ( 168.9999999999999716, -174.9999999999999716, -340.0000000000001137 ) ) ;
#38933 =( BOUNDED_CURVE ( )  B_SPLINE_CURVE ( 3, ( #45380, #10268, #25926, #22056 ),
 .UNSPECIFIED., .F., .F. ) 
 B_SPLINE_CURVE_WITH_KNOTS ( ( 4, 4 ),
 ( 1.570796326794896558, 3.141592653589793116 ),
 .UNSPECIFIED. ) 
 CURVE ( )  GEOMETRIC_REPRESENTATION_ITEM ( )  RATIONAL_B_SPLINE_CURVE ( ( 1.000000000000000000, 0.8047378541243649375, 0.8047378541243649375, 1.000000000000000000 ) ) 
 REPRESENTATION_ITEM ( '' )  );
#38934 = FACE_OUTER_BOUND ( 'NONE', #46202, .T. ) ;
#38935 = CARTESIAN_POINT ( 'NONE',  ( 210.0000000000000568, 0.000000000000000000, -39.18171244307202983 ) ) ;
#38936 = DIRECTION ( 'NONE',  ( 0.000000000000000000, 0.000000000000000000, 1.000000000000000000 ) ) ;
#38937 = VECTOR ( 'NONE', #14503, 1000.000000000000000 ) ;
#38938 = AXIS2_PLACEMENT_3D ( 'NONE', #24666, #17217, #20799 ) ;
#38939 = VERTEX_POINT ( 'NONE', #6865 ) ;
#38940 = FACE_OUTER_BOUND ( 'NONE', #14570, .T. ) ;
#38941 = CARTESIAN_POINT ( 'NONE',  ( 1.250000000000000222, 0.000000000000000000, 3.333333333333333481 ) ) ;
#38942 = CARTESIAN_POINT ( 'NONE',  ( 0.000000000000000000, 0.000000000000000000, 800.0000000000000000 ) ) ;
#38943 = ORIENTED_EDGE ( 'NONE', *, *, #20926, .F. ) ;
#38944 = DIRECTION ( 'NONE',  ( -1.000000000000000000, 0.000000000000000000, 0.000000000000000000 ) ) ;
#38945 = ORIENTED_EDGE ( 'NONE', *, *, #45696, .F. ) ;
#38946 = DIRECTION ( 'NONE',  ( 1.000000000000000000, 0.000000000000000000, 0.000000000000000000 ) ) ;
#38947 = DIRECTION ( 'NONE',  ( 0.000000000000000000, -1.000000000000000000, -3.186989995019654210E-49 ) ) ;
#38948 = EDGE_CURVE ( 'NONE', #39145, #47361, #34319, .T. ) ;
#38949 = PLANE ( 'NONE',  #19915 ) ;
#38950 = DIRECTION ( 'NONE',  ( 0.000000000000000000, 1.000000000000000000, 0.000000000000000000 ) ) ;
#38951 = EDGE_LOOP ( 'NONE', ( #45234, #23564, #4625, #35758, #687, #3845 ) ) ;
#38952 = PRODUCT_DEFINITION_FORMATION_WITH_SPECIFIED_SOURCE ( 'ANY', '', #9324, .NOT_KNOWN. ) ;
#38953 =( NAMED_UNIT ( * ) SI_UNIT ( $, .STERADIAN. ) SOLID_ANGLE_UNIT ( ) );
#38954 = ORIENTED_EDGE ( 'NONE', *, *, #36410, .F. ) ;
#38955 = ORIENTED_EDGE ( 'NONE', *, *, #31003, .T. ) ;
#38956 = AXIS2_PLACEMENT_3D ( 'NONE', #45992, #22680, #26792 ) ;
#38957 = CARTESIAN_POINT ( 'NONE',  ( -0.3862712429686889770, 1.188820645368940720, 9.972675548442463622 ) ) ;
#38958 = EDGE_LOOP ( 'NONE', ( #28270, #26733, #13428, #45833, #7926, #18234, #8130, #34219 ) ) ;
#38959 = DIRECTION ( 'NONE',  ( 1.000000000000000000, 0.000000000000000000, 0.000000000000000000 ) ) ;
#38960 = CARTESIAN_POINT ( 'NONE',  ( 340.0000000000000568, 181.0000000000000284, 355.9999999999997726 ) ) ;
#38961 = CARTESIAN_POINT ( 'NONE',  ( -0.5113015165352315927, -1.175527691268679398, 9.948547179989621014 ) ) ;
#38962 = ORIENTED_EDGE ( 'NONE', *, *, #20171, .F. ) ;
#38963 = CARTESIAN_POINT ( 'NONE',  ( -114.9999999999984652, 17.00000000000000000, 60.00000000000000000 ) ) ;
#38964 = CARTESIAN_POINT ( 'NONE',  ( 355.9999999999999432, -185.0000000000001421, -360.0000000000003411 ) ) ;
#38965 = VECTOR ( 'NONE', #899, 1000.000000000000000 ) ;
#38966 = EDGE_LOOP ( 'NONE', ( #3223, #5230, #15901, #40218, #47115, #6459 ) ) ;
#38967 = FACE_OUTER_BOUND ( 'NONE', #8055, .T. ) ;
#38968 = CARTESIAN_POINT ( 'NONE',  ( -194.9999999999999432, 164.9999999999999716, 252.0000000000000000 ) ) ;
#38969 = MANIFOLD_SOLID_BREP ( 'Boss-Extrude6', #46569 ) ;
#38970 = EDGE_LOOP ( 'NONE', ( #2175, #15083, #20461, #45721 ) ) ;
#38971 = VECTOR ( 'NONE', #37181, 1000.000000000000000 ) ;
#38972 = EDGE_LOOP ( 'NONE', ( #34647, #151, #5391, #22739, #1612, #30492, #27412, #31310 ) ) ;
#38973 = VERTEX_POINT ( 'NONE', #11228 ) ;
#38974 = CARTESIAN_POINT ( 'NONE',  ( 35.00000000000091660, 17.00000000000000000, -24.99999999999999289 ) ) ;
#38975 = VECTOR ( 'NONE', #50530, 1000.000000000000000 ) ;
#38976 = CARTESIAN_POINT ( 'NONE',  ( -21.24469349090191983, -33.89193117067290473, 910.0000000000000000 ) ) ;
#38977 = ORIENTED_EDGE ( 'NONE', *, *, #1422, .T. ) ;
#38978 = DIRECTION ( 'NONE',  ( 0.000000000000000000, 0.000000000000000000, -1.000000000000000000 ) ) ;
#38979 = FILL_AREA_STYLE ('',( #18438 ) ) ;
#38980 = DIRECTION ( 'NONE',  ( -1.000000000000000000, -0.000000000000000000, -0.000000000000000000 ) ) ;
#38981 = FACE_OUTER_BOUND ( 'NONE', #6920, .T. ) ;
#38982 = CARTESIAN_POINT ( 'NONE',  ( 339.9999999999999432, -169.0000000000001137, -344.0000000000002842 ) ) ;
#38983 = CARTESIAN_POINT ( 'NONE',  ( -1.337801958641930300, -1.088266084286974689, 9.928159647716134018 ) ) ;
#38984 =( GEOMETRIC_REPRESENTATION_CONTEXT ( 3 ) GLOBAL_UNCERTAINTY_ASSIGNED_CONTEXT ( ( #19304 ) ) GLOBAL_UNIT_ASSIGNED_CONTEXT ( ( #46750, #20605, #44929 ) ) REPRESENTATION_CONTEXT ( 'NONE', 'WORKASPACE' ) );
#38985 = VECTOR ( 'NONE', #38411, 1000.000000000000000 ) ;
#38986 = CARTESIAN_POINT ( 'NONE',  ( 14.49999999999999822, 13.48684210526315930, 20.00000000000000000 ) ) ;
#38987 = DIRECTION ( 'NONE',  ( -0.000000000000000000, -0.000000000000000000, -1.000000000000000000 ) ) ;
#38988 = CARTESIAN_POINT ( 'NONE',  ( 32.27890028733795447, -1.750000000000009548, -160.2068387089191219 ) ) ;
#38989 = CARTESIAN_POINT ( 'NONE',  ( -126.6959734468149321, -1.749999999999997113, 40.81828755692798438 ) ) ;
#38990 = B_SPLINE_CURVE_WITH_KNOTS ( 'NONE', 3,
 ( #29779, #2567, #3069, #6934 ),
 .UNSPECIFIED., .F., .F.,
 ( 4, 4 ),
 ( 0.000000000000000000, 0.0001252128669263108287 ),
 .UNSPECIFIED. ) ;
#38991 = AXIS2_PLACEMENT_3D ( 'NONE', #45748, #33499, #1937 ) ;
#38992 = VERTEX_POINT ( 'NONE', #3002 ) ;
#38993 = CARTESIAN_POINT ( 'NONE',  ( 130.0000000000018474, 17.00000000000000000, 90.00000000000000000 ) ) ;
#38994 = CARTESIAN_POINT ( 'NONE',  ( -8.445973446814976526, 0.000000000000000000, -37.43171244307200141 ) ) ;
#38995 = DIRECTION ( 'NONE',  ( -1.000000000000000000, -0.000000000000000000, -0.000000000000000000 ) ) ;
#38996 = FACE_OUTER_BOUND ( 'NONE', #39137, .T. ) ;
#38997 = VERTEX_POINT ( 'NONE', #37935 ) ;
#38998 = PLANE ( 'NONE',  #2396 ) ;
#38999 = CARTESIAN_POINT ( 'NONE',  ( 113.3040265531850537, -1.749999999999996891, -159.1817124430720298 ) ) ;
#39000 = CARTESIAN_POINT ( 'NONE',  ( 342.8284271247462129, 182.9999999999999716, 357.9999999999996589 ) ) ;
#39001 = CARTESIAN_POINT ( 'NONE',  ( -44.94597344681493922, 2.143131898507880377E-16, -77.43171244307198720 ) ) ;
#39002 = ORIENTED_EDGE ( 'NONE', *, *, #31490, .T. ) ;
#39003 = VECTOR ( 'NONE', #15915, 1000.000000000000000 ) ;
#39004 = DIRECTION ( 'NONE',  ( -0.000000000000000000, -0.000000000000000000, -1.000000000000000000 ) ) ;
#39005 = ORIENTED_EDGE ( 'NONE', *, *, #49902, .F. ) ;
#39006 = EDGE_CURVE ( 'NONE', #24564, #32291, #41509, .T. ) ;
#39007 = CARTESIAN_POINT ( 'NONE',  ( 350.0000000000000000, -180.9999999999999716, -360.0000000000002274 ) ) ;
#39008 = AXIS2_PLACEMENT_3D ( 'NONE', #23176, #26275, #10864 ) ;
#39009 = ORIENTED_EDGE ( 'NONE', *, *, #10322, .F. ) ;
#39010 = CARTESIAN_POINT ( 'NONE',  ( 185.0000000000000284, 6.000000000000060396, 339.9999999999998863 ) ) ;
#39011 = ADVANCED_FACE ( 'NONE', ( #46338 ), #10460, .T. ) ;
#39012 = DIRECTION ( 'NONE',  ( 0.000000000000000000, -1.822804496942679766E-16, -1.000000000000000000 ) ) ;
#39013 = ORIENTED_EDGE ( 'NONE', *, *, #35715, .F. ) ;
#39014 = CARTESIAN_POINT ( 'NONE',  ( 168.9999999999999716, -270.5000000000000000, -114.9999999999999147 ) ) ;
#39015 = ORIENTED_EDGE ( 'NONE', *, *, #10493, .T. ) ;
#39016 = ADVANCED_FACE ( 'NONE', ( #2508 ), #23007, .T. ) ;
#39017 = ADVANCED_FACE ( 'NONE', ( #10705 ), #42011, .T. ) ;
#39018 = VECTOR ( 'NONE', #22532, 1000.000000000000000 ) ;
#39019 = EDGE_LOOP ( 'NONE', ( #4836, #22720, #6949, #28502, #38266, #21852 ) ) ;
#39020 = CARTESIAN_POINT ( 'NONE',  ( 71.55402655318505367, 0.000000000000000000, 79.06828755692797017 ) ) ;
#39021 = LINE ( 'NONE', #529, #6031 ) ;
#39022 = PRESENTATION_LAYER_ASSIGNMENT (  '', '', ( #14427 ) ) ;
#39023 = ORIENTED_EDGE ( 'NONE', *, *, #30614, .F. ) ;
#39024 = CYLINDRICAL_SURFACE ( 'NONE', #19657, 1.750000000000001554 ) ;
#39025 = CARTESIAN_POINT ( 'NONE',  ( 112.2789002873379758, 1.749999999999996669, -0.2068387089191042749 ) ) ;
#39026 = CARTESIAN_POINT ( 'NONE',  ( -177.4999999999999716, -77.43746236555679729, -130.5992382549688671 ) ) ;
#39027 = ORIENTED_EDGE ( 'NONE', *, *, #28731, .F. ) ;
#39028 = DIRECTION ( 'NONE',  ( 1.000000000000000000, 0.000000000000000000, 0.000000000000000000 ) ) ;
#39029 = VECTOR ( 'NONE', #1712, 1000.000000000000000 ) ;
#39030 = PLANE ( 'NONE',  #11664 ) ;
#39031 = EDGE_LOOP ( 'NONE', ( #1525, #35135, #34899, #18688 ) ) ;
#39032 = CARTESIAN_POINT ( 'NONE',  ( 0.000000000000000000, 183.0000000000000284, -356.0000000000002274 ) ) ;
#39033 = CARTESIAN_POINT ( 'NONE',  ( -25.45361382821521445, 27.58774327458509390, 1.982731392810406668 ) ) ;
#39034 = VERTEX_POINT ( 'NONE', #26101 ) ;
#39035 = CARTESIAN_POINT ( 'NONE',  ( 210.0000000000000568, 2.143131898507881116E-16, 39.06828755692797728 ) ) ;
#39036 = DIRECTION ( 'NONE',  ( 1.000000000000000000, 0.000000000000000000, 0.000000000000000000 ) ) ;
#39037 = EDGE_CURVE ( 'NONE', #20525, #24506, #15677, .T. ) ;
#39038 = ORIENTED_EDGE ( 'NONE', *, *, #17459, .T. ) ;
#39039 = EDGE_CURVE ( 'NONE', #46103, #14468, #38684, .T. ) ;
#39040 = DIRECTION ( 'NONE',  ( 1.000000000000000000, 0.000000000000000000, 0.000000000000000000 ) ) ;
#39041 = DIRECTION ( 'NONE',  ( 0.000000000000000000, -0.000000000000000000, -1.000000000000000000 ) ) ;
#39042 = CARTESIAN_POINT ( 'NONE',  ( -210.0000000000000568, 0.000000000000000000, -39.18171244307202983 ) ) ;
#39043 = CARTESIAN_POINT ( 'NONE',  ( 0.4152287376636409899, -2.070986276654470881, 9.884520316594377576 ) ) ;
#39044 = ADVANCED_FACE ( 'NONE', ( #42264 ), #22762, .T. ) ;
#39045 = AXIS2_PLACEMENT_3D ( 'NONE', #39655, #32466, #47303 ) ;
#39046 = EDGE_CURVE ( 'NONE', #44330, #20358, #49665, .T. ) ;
#39047 = VECTOR ( 'NONE', #39279, 1000.000000000000000 ) ;
#39048 = ORIENTED_EDGE ( 'NONE', *, *, #427, .F. ) ;
#39049 = CARTESIAN_POINT ( 'NONE',  ( 31.94178169330218964, -9.256608784833820991, -3.760136334089591248 ) ) ;
#39050 = EDGE_CURVE ( 'NONE', #7869, #43947, #11988, .T. ) ;
#39051 = CARTESIAN_POINT ( 'NONE',  ( 111.5540265531850537, -1.025126265847081664, 2.568287556927973281 ) ) ;
#39052 = EDGE_CURVE ( 'NONE', #27797, #44740, #27383, .T. ) ;
#39053 = CARTESIAN_POINT ( 'NONE',  ( 9.260964247899973856, -13.84230907185609460, -9.683996418299976483 ) ) ;
#39054 = ORIENTED_EDGE ( 'NONE', *, *, #25591, .F. ) ;
#39055 = VERTEX_POINT ( 'NONE', #192 ) ;
#39056 = DIRECTION ( 'NONE',  ( 0.9254228096423284811, 2.231518430201009162E-15, 0.3789361732451775877 ) ) ;
#39057 = DIRECTION ( 'NONE',  ( -0.000000000000000000, -0.000000000000000000, 1.000000000000000000 ) ) ;
#39058 = AXIS2_PLACEMENT_3D ( 'NONE', #42978, #47050, #42467 ) ;
#39059 = CARTESIAN_POINT ( 'NONE',  ( -124.9459734468149321, -1.025126265847081886, -40.93171244307202272 ) ) ;
#39060 = MANIFOLD_SOLID_BREP ( 'Square tube 20 X 20 X 2(1)[8]', #20377 ) ;
#39061 = CARTESIAN_POINT ( 'NONE',  ( -205.6708471809678827, -1.750000000000009326, -158.1565861772249377 ) ) ;
#39062 = VECTOR ( 'NONE', #39494, 1000.000000000000000 ) ;
#39063 = DIRECTION ( 'NONE',  ( -1.000000000000000000, -0.000000000000000000, -0.000000000000000000 ) ) ;
#39064 = ORIENTED_EDGE ( 'NONE', *, *, #11750, .F. ) ;
#39065 = CARTESIAN_POINT ( 'NONE',  ( -0.3862712429686729343, -1.188820645368946050, -3.333333333333333481 ) ) ;
#39066 = CARTESIAN_POINT ( 'NONE',  ( -16.16402646813540755, 4.033894069732547827, -3.546734833711462365 ) ) ;
#39067 = ADVANCED_FACE ( 'NONE', ( #47595 ), #28140, .F. ) ;
#39068 = EDGE_CURVE ( 'NONE', #18793, #4444, #35608, .T. ) ;
#39069 = VECTOR ( 'NONE', #44163, 1000.000000000000000 ) ;
#39070 =( BOUNDED_CURVE ( )  B_SPLINE_CURVE ( 3, ( #4952, #32423, #48017, #12902 ),
 .UNSPECIFIED., .F., .F. ) 
 B_SPLINE_CURVE_WITH_KNOTS ( ( 4, 4 ),
 ( 1.570796326794896558, 3.141592653589793116 ),
 .UNSPECIFIED. ) 
 CURVE ( )  GEOMETRIC_REPRESENTATION_ITEM ( )  RATIONAL_B_SPLINE_CURVE ( ( 1.000000000000000000, 0.8047378541243649375, 0.8047378541243649375, 1.000000000000000000 ) ) 
 REPRESENTATION_ITEM ( '' )  );
#39071 = ORIENTED_EDGE ( 'NONE', *, *, #3763, .T. ) ;
#39072 = EDGE_CURVE ( 'NONE', #18367, #27545, #20183, .T. ) ;
#39073 = LINE ( 'NONE', #42630, #45200 ) ;
#39074 = EDGE_LOOP ( 'NONE', ( #31466, #957, #48666, #33969 ) ) ;
#39075 = EDGE_CURVE ( 'NONE', #29935, #47880, #27132, .T. ) ;
#39076 = CARTESIAN_POINT ( 'NONE',  ( 339.9999999999999432, 166.6568542494925396, -341.6568542494925396 ) ) ;
#39077 = CARTESIAN_POINT ( 'NONE',  ( -7.749480817862350435, -14.85497772329513211, 9.403735324607438884 ) ) ;
#39078 = ORIENTED_EDGE ( 'NONE', *, *, #48550, .F. ) ;
#39079 = CARTESIAN_POINT ( 'NONE',  ( -24.39427009666018265, -44.07992421011638129, 8.807470649214879543 ) ) ;
#39080 = CARTESIAN_POINT ( 'NONE',  ( 80.00000000000061107, 17.00000000000000000, -54.99999999999999289 ) ) ;
#39081 = CARTESIAN_POINT ( 'NONE',  ( -1.011271242968693862, 0.7347315653655780432, -10.00000000000000000 ) ) ;
#39082 = DIRECTION ( 'NONE',  ( -1.000000000000000000, 0.000000000000000000, 0.000000000000000000 ) ) ;
#39083 = ORIENTED_EDGE ( 'NONE', *, *, #794, .F. ) ;
#39084 = EDGE_CURVE ( 'NONE', #21262, #40406, #5187, .T. ) ;
#39085 = DIRECTION ( 'NONE',  ( 0.000000000000000000, 0.000000000000000000, -1.000000000000000000 ) ) ;
#39086 = DIRECTION ( 'NONE',  ( 1.000000000000000000, -0.000000000000000000, 0.000000000000000000 ) ) ;
#39087 = ORIENTED_EDGE ( 'NONE', *, *, #6541, .T. ) ;
#39088 = CARTESIAN_POINT ( 'NONE',  ( 113.3040265531850537, 1.749999999999997335, -119.1817124430720440 ) ) ;
#39089 = CARTESIAN_POINT ( 'NONE',  ( 339.9999999999999432, -168.9999999999999432, -360.0000000000002274 ) ) ;
#39090 = LINE ( 'NONE', #4424, #31172 ) ;
#39091 = DIRECTION ( 'NONE',  ( 0.000000000000000000, 1.000000000000000000, -0.000000000000000000 ) ) ;
#39092 =( BOUNDED_CURVE ( )  B_SPLINE_CURVE ( 3, ( #23485, #26316, #22456, #6807 ),
 .UNSPECIFIED., .F., .F. ) 
 B_SPLINE_CURVE_WITH_KNOTS ( ( 4, 4 ),
 ( 4.712388980384689674, 6.283185307179586232 ),
 .UNSPECIFIED. ) 
 CURVE ( )  GEOMETRIC_REPRESENTATION_ITEM ( )  RATIONAL_B_SPLINE_CURVE ( ( 1.000000000000000000, 0.8047378541243649375, 0.8047378541243649375, 1.000000000000000000 ) ) 
 REPRESENTATION_ITEM ( '' )  );
#39093 = EDGE_LOOP ( 'NONE', ( #21341, #46503, #1421, #13797 ) ) ;
#39094 = ORIENTED_EDGE ( 'NONE', *, *, #33487, .F. ) ;
#39095 = DIRECTION ( 'NONE',  ( 0.000000000000000000, 0.000000000000000000, 1.000000000000000000 ) ) ;
#39096 = B_SPLINE_CURVE_WITH_KNOTS ( 'NONE', 3,
 ( #38567, #3379, #27258, #45955 ),
 .UNSPECIFIED., .F., .F.,
 ( 4, 4 ),
 ( 0.000000000000000000, 0.0002610106747150458747 ),
 .UNSPECIFIED. ) ;
#39097 = ORIENTED_EDGE ( 'NONE', *, *, #8064, .F. ) ;
#39098 = CARTESIAN_POINT ( 'NONE',  ( 195.0540265531851105, 2.143131898507880377E-16, -120.9317124430720156 ) ) ;
#39099 = CARTESIAN_POINT ( 'NONE',  ( -0.5000000000000000000, -0.5000000000000000000, 1000.000000000000000 ) ) ;
#39100 = EDGE_CURVE ( 'NONE', #12877, #19097, #442, .T. ) ;
#39101 = EDGE_LOOP ( 'NONE', ( #17883, #49078, #13494, #7931 ) ) ;
#39102 = DIRECTION ( 'NONE',  ( 0.000000000000000000, -1.000000000000000000, 0.000000000000000000 ) ) ;
#39103 = EDGE_LOOP ( 'NONE', ( #46191, #14918, #23403, #33660 ) ) ;
#39104 = CARTESIAN_POINT ( 'NONE',  ( 7.499999999999996447, 194.9999999999999716, -224.9999999999999716 ) ) ;
#39105 = VECTOR ( 'NONE', #11751, 1000.000000000000000 ) ;
#39106 = CARTESIAN_POINT ( 'NONE',  ( 130.0000000000021032, 17.00000000000000000, 95.00000000000000000 ) ) ;
#39107 = ADVANCED_FACE ( 'NONE', ( #43013 ), #35362, .F. ) ;
#39109 = VERTEX_POINT ( 'NONE', #47083 ) ;
#39108 = EDGE_CURVE ( 'NONE', #41145, #19783, #39699, .T. ) ;
#39110 = ORIENTED_EDGE ( 'NONE', *, *, #44744, .F. ) ;
#39111 = ORIENTED_EDGE ( 'NONE', *, *, #47512, .F. ) ;
#39112 = DIRECTION ( 'NONE',  ( 0.000000000000000000, 5.664403186863042467E-17, 1.000000000000000000 ) ) ;
#39113 = DIRECTION ( 'NONE',  ( 0.000000000000000000, 0.000000000000000000, 1.000000000000000000 ) ) ;
#39114 = CYLINDRICAL_SURFACE ( 'NONE', #8497, 1.750000000000001554 ) ;
#39115 = ADVANCED_FACE ( 'NONE', ( #16087 ), #11727, .F. ) ;
#39116 = ORIENTED_EDGE ( 'NONE', *, *, #13150, .F. ) ;
#39117 = CARTESIAN_POINT ( 'NONE',  ( 33.30402655318503946, 1.750000000000010658, 120.8182875569279702 ) ) ;
#39118 = ORIENTED_EDGE ( 'NONE', *, *, #17243, .T. ) ;
#39119 = EDGE_CURVE ( 'NONE', #34716, #23271, #24831, .T. ) ;
#39120 = DIRECTION ( 'NONE',  ( 0.000000000000000000, -1.000000000000000000, 0.000000000000000000 ) ) ;
#39121 = ORIENTED_EDGE ( 'NONE', *, *, #27402, .T. ) ;
#39122 = EDGE_CURVE ( 'NONE', #24991, #2139, #27894, .T. ) ;
#39123 = CARTESIAN_POINT ( 'NONE',  ( 210.0000000000000568, 2.143131898507881856E-16, -80.93171244307202983 ) ) ;
#39124 = CARTESIAN_POINT ( 'NONE',  ( 13.92102703536701114, 30.85732372859822803, 8.356839323120299312 ) ) ;
#39125 = CARTESIAN_POINT ( 'NONE',  ( 193.3040265531851105, 1.750000000000010658, -79.18171244307201562 ) ) ;
#39126 = VECTOR ( 'NONE', #7594, 1000.000000000000000 ) ;
#39127 = DIRECTION ( 'NONE',  ( -1.000000000000000000, 0.000000000000000000, -1.612977847700450206E-50 ) ) ;
#39128 = ORIENTED_EDGE ( 'NONE', *, *, #42214, .T. ) ;
#39129 = ORIENTED_EDGE ( 'NONE', *, *, #41420, .T. ) ;
#39130 = CARTESIAN_POINT ( 'NONE',  ( 0.000000000000000000, 0.000000000000000000, 800.0000000000000000 ) ) ;
#39131 = EDGE_CURVE ( 'NONE', #5910, #15638, #30078, .T. ) ;
#39132 = FACE_OUTER_BOUND ( 'NONE', #24271, .T. ) ;
#39133 = CARTESIAN_POINT ( 'NONE',  ( 115.0540265531850395, 2.143131898507847836E-16, 42.56828755692795596 ) ) ;
#39134 = CARTESIAN_POINT ( 'NONE',  ( -46.69597344681494633, -1.750000000000010658, 80.81828755692798438 ) ) ;
#39135 = EDGE_CURVE ( 'NONE', #25919, #43433, #35346, .T. ) ;
#39136 = CARTESIAN_POINT ( 'NONE',  ( 34.94239438780391538, 13.71128139791418832, 3.209567239418968487 ) ) ;
#39137 = EDGE_LOOP ( 'NONE', ( #49010, #45156, #19799, #9927 ) ) ;
#39138 = FACE_OUTER_BOUND ( 'NONE', #38828, .T. ) ;
#39139 = CARTESIAN_POINT ( 'NONE',  ( 339.9999999999999432, -185.0000000000001421, -356.0000000000002274 ) ) ;
#39140 = VERTEX_POINT ( 'NONE', #48596 ) ;
#39141 = DIRECTION ( 'NONE',  ( 1.000000000000000000, 0.000000000000000000, 0.000000000000000000 ) ) ;
#39142 = CARTESIAN_POINT ( 'NONE',  ( -167.7210997126620384, 1.750000000000009548, 39.79316129108089228 ) ) ;
#39143 = CARTESIAN_POINT ( 'NONE',  ( 0.7849184246612691540, -1.242376769536456704, 9.958264684458541183 ) ) ;
#39144 = ORIENTED_EDGE ( 'NONE', *, *, #14888, .F. ) ;
#39145 = VERTEX_POINT ( 'NONE', #40704 ) ;
#39146 = CARTESIAN_POINT ( 'NONE',  ( 193.3040265531851105, -1.750000000000010658, -79.18171244307201562 ) ) ;
#39147 = CARTESIAN_POINT ( 'NONE',  ( -69.99999999999940314, 16.00000000000000000, -54.99999999999999289 ) ) ;
#39148 = AXIS2_PLACEMENT_3D ( 'NONE', #6341, #21986, #37660 ) ;
#39149 = ORIENTED_EDGE ( 'NONE', *, *, #47845, .T. ) ;
#39150 = ORIENTED_EDGE ( 'NONE', *, *, #17136, .F. ) ;
#39151 = CARTESIAN_POINT ( 'NONE',  ( 0.06526599240121484791, -1.373921316406707449, 9.972175347158280800 ) ) ;
#39152 = CARTESIAN_POINT ( 'NONE',  ( 24.47767542868285062, -23.18653802921781448, 8.807470649214879543 ) ) ;
#39153 = DIRECTION ( 'NONE',  ( 0.000000000000000000, 0.000000000000000000, -1.000000000000000000 ) ) ;
#39154 = FACE_OUTER_BOUND ( 'NONE', #23504, .T. ) ;
#39155 = ORIENTED_EDGE ( 'NONE', *, *, #26229, .T. ) ;
#39156 = VERTEX_POINT ( 'NONE', #36628 ) ;
#39157 = ORIENTED_EDGE ( 'NONE', *, *, #32148, .T. ) ;
#39158 = CARTESIAN_POINT ( 'NONE',  ( -8.445973446814976526, 0.000000000000000000, 122.5682875569279986 ) ) ;
#39159 = LINE ( 'NONE', #30956, #2938 ) ;
#39160 = ORIENTED_EDGE ( 'NONE', *, *, #5765, .F. ) ;
#39161 = ADVANCED_FACE ( 'NONE', ( #16844, #21689 ), #44772, .T. ) ;
#39162 = CARTESIAN_POINT ( 'NONE',  ( -0.4166666666666669072, 0.000000000000000000, 10.00000000000000000 ) ) ;
#39163 = EDGE_CURVE ( 'NONE', #39985, #26096, #28128, .T. ) ;
#39164 = CARTESIAN_POINT ( 'NONE',  ( 0.7601424845489945792, -1.297311920616997627, 9.927319414211225990 ) ) ;
#39165 = FACE_OUTER_BOUND ( 'NONE', #40541, .T. ) ;
#39166 = VERTEX_POINT ( 'NONE', #5027 ) ;
#39167 =( BOUNDED_CURVE ( )  B_SPLINE_CURVE ( 3, ( #41717, #18352, #10662, #26325 ),
 .UNSPECIFIED., .F., .F. ) 
 B_SPLINE_CURVE_WITH_KNOTS ( ( 4, 4 ),
 ( 1.570796326794896558, 3.141592653589793116 ),
 .UNSPECIFIED. ) 
 CURVE ( )  GEOMETRIC_REPRESENTATION_ITEM ( )  RATIONAL_B_SPLINE_CURVE ( ( 1.000000000000000000, 0.8047378541243649375, 0.8047378541243649375, 1.000000000000000000 ) ) 
 REPRESENTATION_ITEM ( '' )  );
#39168 = ORIENTED_EDGE ( 'NONE', *, *, #32557, .F. ) ;
#39169 = CARTESIAN_POINT ( 'NONE',  ( -164.9999999999984936, 17.00000000000000000, 35.00000000000000000 ) ) ;
#39170 = CARTESIAN_POINT ( 'NONE',  ( 181.0000000000000284, -9.999999999999953815, -111.0000000000001563 ) ) ;
#39171 = DIRECTION ( 'NONE',  ( 1.000000000000000000, 0.000000000000000000, 0.000000000000000000 ) ) ;
#39172 = EDGE_CURVE ( 'NONE', #290, #11134, #23284, .T. ) ;
#39173 = VERTEX_POINT ( 'NONE', #33011 ) ;
#39174 = VERTEX_POINT ( 'NONE', #12975 ) ;
#39175 = ADVANCED_FACE ( 'NONE', ( #28635 ), #25304, .T. ) ;
#39176 = CYLINDRICAL_SURFACE ( 'NONE', #27441, 10.00000000000000000 ) ;
#39177 = PRESENTATION_STYLE_ASSIGNMENT (( #27874 ) ) ;
#39178 = VERTEX_POINT ( 'NONE', #21436 ) ;
#39179 = ADVANCED_FACE ( 'NONE', ( #25053 ), #1951, .T. ) ;
#39180 = CARTESIAN_POINT ( 'NONE',  ( -167.4999999999999716, 74.83106485270648989, -120.5992382549688955 ) ) ;
#39181 = CARTESIAN_POINT ( 'NONE',  ( -119.9999999999987921, 16.00000000000000000, 5.000000000000004441 ) ) ;
#39182 = DIRECTION ( 'NONE',  ( -1.000000000000000000, -0.000000000000000000, -0.000000000000000000 ) ) ;
#39183 = CARTESIAN_POINT ( 'NONE',  ( 1.011271242968677653, 0.7347315653656002477, -10.00000000000000000 ) ) ;
#39184 = ORIENTED_EDGE ( 'NONE', *, *, #5533, .T. ) ;
#39185 = DIRECTION ( 'NONE',  ( 0.000000000000000000, -2.537652627714643577E-15, -1.000000000000000000 ) ) ;
#39186 = CARTESIAN_POINT ( 'NONE',  ( 210.0000000000000568, 2.143131898507880377E-16, 159.0682875569279702 ) ) ;
#39187 = EDGE_CURVE ( 'NONE', #15972, #15720, #36878, .T. ) ;
#39188 = CARTESIAN_POINT ( 'NONE',  ( 164.9999999999999716, 16.00000000000000000, 5.000000000000004441 ) ) ;
#39189 = CARTESIAN_POINT ( 'NONE',  ( 35.05402655318504657, 2.143131898507880377E-16, 165.0000000000000000 ) ) ;
#39190 = AXIS2_PLACEMENT_3D ( 'NONE', #46324, #23777, #50666 ) ;
#39191 = ORIENTED_EDGE ( 'NONE', *, *, #45223, .F. ) ;
#39192 = LINE ( 'NONE', #11225, #26157 ) ;
#39193 = CARTESIAN_POINT ( 'NONE',  ( -33.64889274059387958, 3.704246042440976439, 8.356839323120299312 ) ) ;
#39194 = DIRECTION ( 'NONE',  ( 1.000000000000000000, 0.000000000000000000, 0.000000000000000000 ) ) ;
#39195 = ORIENTED_EDGE ( 'NONE', *, *, #22425, .T. ) ;
#39196 = CARTESIAN_POINT ( 'NONE',  ( -48.44597344681495343, 0.000000000000000000, 122.5682875569279702 ) ) ;
#39197 = DIRECTION ( 'NONE',  ( 0.000000000000000000, 1.000000000000000000, 0.000000000000000000 ) ) ;
#39198 = ORIENTED_EDGE ( 'NONE', *, *, #14215, .F. ) ;
#39199 = PLANE ( 'NONE',  #45004 ) ;
#39200 = CARTESIAN_POINT ( 'NONE',  ( 14.49999999999999822, -46.01315789473684248, -5.916985404131818171 ) ) ;
#39201 = CARTESIAN_POINT ( 'NONE',  ( -44.94597344681493922, 1.025126265847089879, 122.5682875569280128 ) ) ;
#39202 = ORIENTED_EDGE ( 'NONE', *, *, #38369, .T. ) ;
#39203 = DIRECTION ( 'NONE',  ( -1.000000000000000000, -0.000000000000000000, -0.000000000000000000 ) ) ;
#39204 = B_SPLINE_SURFACE_WITH_KNOTS ( 'NONE', 3, 3, ( 
 ( #46251, #23457, #42427, #7289 ),
 ( #15256, #49826, #50343, #18821 ),
 ( #38102, #27042, #30395, #30916 ),
 ( #7046, #22684, #38357, #46499 ) ),
 .UNSPECIFIED., .F., .F., .F.,
 ( 4, 4 ),
 ( 4, 4 ),
 ( 0.000000000000000000, 1.000000000000000000 ),
 ( 0.000000000000000000, 1.000000000000000000 ),
 .UNSPECIFIED. ) ;
#39205 = EDGE_LOOP ( 'NONE', ( #25765, #10155, #4515, #38954, #11370, #36075, #49428, #42061 ) ) ;
#39206 = ORIENTED_EDGE ( 'NONE', *, *, #42405, .F. ) ;
#39207 = DIRECTION ( 'NONE',  ( 1.000000000000000000, 0.000000000000000000, 0.000000000000000000 ) ) ;
#39208 = ADVANCED_FACE ( 'NONE', ( #37874 ), #49354, .F. ) ;
#39209 = FACE_OUTER_BOUND ( 'NONE', #44162, .T. ) ;
#39210 = VERTEX_POINT ( 'NONE', #11864 ) ;
#39211 = DIRECTION ( 'NONE',  ( -1.000000000000000000, 0.000000000000000000, 0.000000000000000000 ) ) ;
#39212 = FACE_OUTER_BOUND ( 'NONE', #33179, .T. ) ;
#39213 = CARTESIAN_POINT ( 'NONE',  ( 17.34922095635755568, 33.24536858281893359, 8.914903342594564961 ) ) ;
#39214 = ORIENTED_EDGE ( 'NONE', *, *, #41354, .T. ) ;
#39215 = DIRECTION ( 'NONE',  ( -0.000000000000000000, -1.000000000000000000, -0.000000000000000000 ) ) ;
#39216 = CARTESIAN_POINT ( 'NONE',  ( 165.0000000000000000, -174.9999999999999716, -99.00000000000014211 ) ) ;
#39217 = CARTESIAN_POINT ( 'NONE',  ( 194.9999999999999716, 164.9999999999999716, 372.0000000000000000 ) ) ;
#39218 =( BOUNDED_CURVE ( )  B_SPLINE_CURVE ( 3, ( #2331, #45148, #2093, #10036 ),
 .UNSPECIFIED., .F., .F. ) 
 B_SPLINE_CURVE_WITH_KNOTS ( ( 4, 4 ),
 ( 1.570796326794896558, 3.141592653589793116 ),
 .UNSPECIFIED. ) 
 CURVE ( )  GEOMETRIC_REPRESENTATION_ITEM ( )  RATIONAL_B_SPLINE_CURVE ( ( 1.000000000000000000, 0.8047378541243649375, 0.8047378541243649375, 1.000000000000000000 ) ) 
 REPRESENTATION_ITEM ( '' )  );
#39219 = ORIENTED_EDGE ( 'NONE', *, *, #30680, .F. ) ;
#39220 = VECTOR ( 'NONE', #29079, 1000.000000000000000 ) ;
#39221 = CARTESIAN_POINT ( 'NONE',  ( 168.9999999999999716, 165.0000000000000000, -356.0000000000001705 ) ) ;
#39222 = CARTESIAN_POINT ( 'NONE',  ( -7.372990760266265653, 6.123233995736766282E-16, 5.000000000000000000 ) ) ;
#39223 = ORIENTED_EDGE ( 'NONE', *, *, #41507, .F. ) ;
#39224 = ORIENTED_EDGE ( 'NONE', *, *, #35100, .F. ) ;
#39225 = ORIENTED_EDGE ( 'NONE', *, *, #47742, .T. ) ;
#39226 = CARTESIAN_POINT ( 'NONE',  ( 33.14391172085757375, 37.72293746533119929, -8.016098858316199838 ) ) ;
#39227 =( BOUNDED_CURVE ( )  B_SPLINE_CURVE ( 3, ( #42708, #11944, #47041, #27602 ),
 .UNSPECIFIED., .F., .F. ) 
 B_SPLINE_CURVE_WITH_KNOTS ( ( 4, 4 ),
 ( 4.712388980384689674, 6.283185307179586232 ),
 .UNSPECIFIED. ) 
 CURVE ( )  GEOMETRIC_REPRESENTATION_ITEM ( )  RATIONAL_B_SPLINE_CURVE ( ( 1.000000000000000000, 0.8047378541243649375, 0.8047378541243649375, 1.000000000000000000 ) ) 
 REPRESENTATION_ITEM ( '' )  );
#39228 = LINE ( 'NONE', #23567, #28316 ) ;
#39229 = ORIENTED_EDGE ( 'NONE', *, *, #14890, .T. ) ;
#39230 = CLOSED_SHELL ( 'NONE', ( #45207, #25344, #50075, #20269, #1561, #33775, #28003, #45243, #28651, #38181, #43760, #47291, #45082, #2605, #26003, #27698, #22686, #23531, #21725, #8972, #14599, #33581, #33751, #20443, #34070, #46481, #35772, #25296, #33501, #12963, #36478, #47811, #43551, #8051, #2075, #41302, #27415, #38750, #30067, #13430, #10259, #39702, #28428, #6426, #17833, #38109, #14185, #46478, #35650, #36890, #42606, #45784, #35635, #26814, #9882, #29406, #18607 ) ) ;
#39231 = CARTESIAN_POINT ( 'NONE',  ( 32.27890028733795447, -1.750000000000009548, 161.8434138227750907 ) ) ;
#39232 = CYLINDRICAL_SURFACE ( 'NONE', #13125, 1.749999999999987566 ) ;
#39233 = CARTESIAN_POINT ( 'NONE',  ( 0.3862712429686894766, -1.188820645368940276, 10.00000000000000000 ) ) ;
#39234 = CARTESIAN_POINT ( 'NONE',  ( -3.229232847726260403, 16.57333684275945629, 9.178419661560148768 ) ) ;
#39235 = FACE_OUTER_BOUND ( 'NONE', #21279, .T. ) ;
#39236 = CARTESIAN_POINT ( 'NONE',  ( 71.55402655318505367, 0.000000000000000000, 82.56828755692799859 ) ) ;
#39237 = CARTESIAN_POINT ( 'NONE',  ( -1.275927284277175167, 0.1224368140627496299, 9.976582533991679824 ) ) ;
#39238 = B_SPLINE_CURVE_WITH_KNOTS ( 'NONE', 3,
 ( #5580, #17879, #33558, #44550 ),
 .UNSPECIFIED., .F., .F.,
 ( 4, 4 ),
 ( 0.000000000000000000, 0.0002610106747335709325 ),
 .UNSPECIFIED. ) ;
#39240 = ADVANCED_FACE ( 'NONE', ( #34014 ), #17843, .F. ) ;
#39239 = CARTESIAN_POINT ( 'NONE',  ( 45.35314062630785514, -8.244242869018759023, 8.807470649214881320 ) ) ;
#39241 = CARTESIAN_POINT ( 'NONE',  ( -9.760995290733800900, 2.173239732351794462, 9.646707543097347681 ) ) ;
#39242 = CYLINDRICAL_SURFACE ( 'NONE', #28935, 1.750000000000001554 ) ;
#39243 = PLANE ( 'NONE',  #19148 ) ;
#39244 = FACE_OUTER_BOUND ( 'NONE', #4007, .T. ) ;
#39245 = DIRECTION ( 'NONE',  ( 0.000000000000000000, -0.2223603367690619725, -0.9749645535258958384 ) ) ;
#39246 = CARTESIAN_POINT ( 'NONE',  ( -119.9999999999987921, 16.00000000000000000, 5.000000000000004441 ) ) ;
#39247 = ORIENTED_EDGE ( 'NONE', *, *, #4528, .F. ) ;
#39248 = CYLINDRICAL_SURFACE ( 'NONE', #42526, 1.750000000000036193 ) ;
#39249 = CARTESIAN_POINT ( 'NONE',  ( 114.3291528190321173, -1.749999999999996225, 159.7931612910809065 ) ) ;
#39250 = CARTESIAN_POINT ( 'NONE',  ( 342.0000000000000568, 182.1715728752537871, 357.1715728752535597 ) ) ;
#39251 = LINE ( 'NONE', #4093, #23838 ) ;
#39252 = VECTOR ( 'NONE', #2432, 1000.000000000000000 ) ;
#39253 = ORIENTED_EDGE ( 'NONE', *, *, #43353, .F. ) ;
#39254 = CARTESIAN_POINT ( 'NONE',  ( -0.9983599181300891745, -1.124146016603549070, 9.953784399990620813 ) ) ;
#39256 = ORIENTED_EDGE ( 'NONE', *, *, #24576, .F. ) ;
#39255 = AXIS2_PLACEMENT_3D ( 'NONE', #49473, #46126, #30034 ) ;
#39257 = LINE ( 'NONE', #42327, #21286 ) ;
#39258 = VECTOR ( 'NONE', #6974, 1000.000000000000000 ) ;
#39259 = ORIENTED_EDGE ( 'NONE', *, *, #17496, .T. ) ;
#39260 = VECTOR ( 'NONE', #49189, 1000.000000000000000 ) ;
#39261 = CARTESIAN_POINT ( 'NONE',  ( 164.9999999999999716, -180.9999999999999716, -350.0000000000001705 ) ) ;
#39262 = DIRECTION ( 'NONE',  ( 0.000000000000000000, 0.000000000000000000, -1.000000000000000000 ) ) ;
#39263 = ORIENTED_EDGE ( 'NONE', *, *, #20553, .T. ) ;
#39264 = DIRECTION ( 'NONE',  ( -0.000000000000000000, -0.000000000000000000, -1.000000000000000000 ) ) ;
#39265 = CIRCLE ( 'NONE', #14666, 1.750000000000036193 ) ;
#39266 = EDGE_LOOP ( 'NONE', ( #41106, #37946, #46854, #32164, #18161, #15281 ) ) ;
#39267 = EDGE_CURVE ( 'NONE', #39676, #19082, #45767, .T. ) ;
#39268 = AXIS2_PLACEMENT_3D ( 'NONE', #6185, #18217, #49232 ) ;
#39269 = VERTEX_POINT ( 'NONE', #6802 ) ;
#39270 = CARTESIAN_POINT ( 'NONE',  ( -14.99999999999812594, 16.00000000000000000, 65.00000000000000000 ) ) ;
#39271 = CARTESIAN_POINT ( 'NONE',  ( -119.9999999999997158, 17.00000000000000000, -84.99999999999998579 ) ) ;
#39272 = ORIENTED_EDGE ( 'NONE', *, *, #34383, .F. ) ;
#39273 = DIRECTION ( 'NONE',  ( -0.000000000000000000, -1.000000000000000000, -0.000000000000000000 ) ) ;
#39274 = DIRECTION ( 'NONE',  ( -1.000000000000000000, 0.000000000000000000, 0.000000000000000000 ) ) ;
#39275 = ORIENTED_EDGE ( 'NONE', *, *, #18348, .F. ) ;
#39276 = DIRECTION ( 'NONE',  ( -1.000000000000000000, 0.000000000000000000, 0.000000000000000000 ) ) ;
#39277 = CARTESIAN_POINT ( 'NONE',  ( 169.0000000000000284, 175.0000000000000284, 339.9999999999998863 ) ) ;
#39278 = ORIENTED_EDGE ( 'NONE', *, *, #21484, .T. ) ;
#39279 = DIRECTION ( 'NONE',  ( -1.000000000000000000, -0.000000000000000000, -0.000000000000000000 ) ) ;
#39280 = CARTESIAN_POINT ( 'NONE',  ( 153.3040265531850537, -1.750000000000010214, 40.81828755692798438 ) ) ;
#39281 = ORIENTED_EDGE ( 'NONE', *, *, #19553, .T. ) ;
#39282 = FACE_OUTER_BOUND ( 'NONE', #40661, .T. ) ;
#39283 = DIRECTION ( 'NONE',  ( -0.000000000000000000, -0.000000000000000000, -1.000000000000000000 ) ) ;
#39284 = VERTEX_POINT ( 'NONE', #45265 ) ;
#39285 = FACE_OUTER_BOUND ( 'NONE', #21398, .T. ) ;
#39286 = AXIS2_PLACEMENT_3D ( 'NONE', #40445, #5282, #39443 ) ;
#39287 = CARTESIAN_POINT ( 'NONE',  ( -32.43949840348904701, -7.871562655726277669, -9.367992836599951190 ) ) ;
#39288 = CARTESIAN_POINT ( 'NONE',  ( -69.99999999999816680, 16.00000000000000000, 65.00000000000000000 ) ) ;
#39289 = PLANE ( 'NONE',  #40336 ) ;
#39290 = AXIS2_PLACEMENT_3D ( 'NONE', #38816, #3645, #19291 ) ;
#39291 = ORIENTED_EDGE ( 'NONE', *, *, #2358, .F. ) ;
#39292 = CARTESIAN_POINT ( 'NONE',  ( 0.3862712429686727678, 1.188820645368945605, -10.00000000000000000 ) ) ;
#39293 = AXIS2_PLACEMENT_3D ( 'NONE', #43298, #47112, #47364 ) ;
#39295 = ADVANCED_FACE ( 'NONE', ( #10648 ), #36798, .T. ) ;
#39294 = DIRECTION ( 'NONE',  ( 1.000000000000000000, 0.000000000000000000, 1.586032872232979935E-16 ) ) ;
#39296 = LINE ( 'NONE', #19779, #35479 ) ;
#39297 = ORIENTED_EDGE ( 'NONE', *, *, #39671, .T. ) ;
#39298 = ORIENTED_EDGE ( 'NONE', *, *, #46995, .F. ) ;
#39299 = PRODUCT_CONTEXT ( 'NONE', #21692, 'mechanical' ) ;
#39301 = CARTESIAN_POINT ( 'NONE',  ( 31.55402655318503236, 1.025126265847089657, -120.9317124430720440 ) ) ;
#39300 = VECTOR ( 'NONE', #14696, 1000.000000000000000 ) ;
#39302 = DIRECTION ( 'NONE',  ( 0.000000000000000000, 0.000000000000000000, 1.000000000000000000 ) ) ;
#39303 = MANIFOLD_SOLID_BREP ( 'Square tube 20 X 20 X 2(1)[7]', #34309 ) ;
#39304 = DIRECTION ( 'NONE',  ( -0.000000000000000000, -0.000000000000000000, -1.000000000000000000 ) ) ;
#39305 = CARTESIAN_POINT ( 'NONE',  ( 2.418900724918336298, 41.61933801977895087, -9.387872844313825738 ) ) ;
#39306 = ORIENTED_EDGE ( 'NONE', *, *, #43053, .T. ) ;
#39307 = CARTESIAN_POINT ( 'NONE',  ( -5.000000000000000000, -175.0000000000000284, 353.7500000000001705 ) ) ;
#39308 = EDGE_CURVE ( 'NONE', #1108, #47565, #18335, .T. ) ;
#39309 = EDGE_CURVE ( 'NONE', #48553, #49726, #14198, .T. ) ;
#39310 = PRODUCT_DEFINITION_SHAPE ( 'NONE', 'NONE',  #50735 ) ;
#39311 = DIRECTION ( 'NONE',  ( 0.000000000000000000, 0.000000000000000000, 1.000000000000000000 ) ) ;
#39312 = CARTESIAN_POINT ( 'NONE',  ( 210.0000000000000568, 0.000000000000000000, 0.8182875569279768335 ) ) ;
#39313 = DIRECTION ( 'NONE',  ( 1.333906992743555050E-23, -1.000000000000000000, 0.000000000000000000 ) ) ;
#39314 = EDGE_CURVE ( 'NONE', #40295, #24192, #41594, .T. ) ;
#39315 = ORIENTED_EDGE ( 'NONE', *, *, #29142, .F. ) ;
#39316 = CARTESIAN_POINT ( 'NONE',  ( 114.3291528190321173, 1.749999999999996891, -120.2068387089191219 ) ) ;
#39317 = ORIENTED_EDGE ( 'NONE', *, *, #17055, .F. ) ;
#39318 = FACE_OUTER_BOUND ( 'NONE', #18361, .T. ) ;
#39319 = VERTEX_POINT ( 'NONE', #37624 ) ;
#39320 = FACE_OUTER_BOUND ( 'NONE', #14895, .T. ) ;
#39321 = CARTESIAN_POINT ( 'NONE',  ( -1.011271242968693862, 0.7347315653655780432, -3.333333333333333481 ) ) ;
#39322 = EDGE_CURVE ( 'NONE', #47604, #24955, #40562, .T. ) ;
#39323 = DIRECTION ( 'NONE',  ( 1.000000000000000000, 0.000000000000000000, -0.000000000000000000 ) ) ;
#39324 = EDGE_CURVE ( 'NONE', #41657, #13983, #10723, .T. ) ;
#39325 = AXIS2_PLACEMENT_3D ( 'NONE', #22016, #10979, #21771 ) ;
#39326 = VERTEX_POINT ( 'NONE', #24180 ) ;
#39327 = VECTOR ( 'NONE', #17654, 1000.000000000000000 ) ;
#39328 = EDGE_CURVE ( 'NONE', #16502, #40868, #1333, .T. ) ;
#39329 = ADVANCED_FACE ( 'NONE', ( #35480 ), #28525, .T. ) ;
#39330 = AXIS2_PLACEMENT_3D ( 'NONE', #42383, #30602, #45957 ) ;
#39331 = CARTESIAN_POINT ( 'NONE',  ( 85.00000000000029843, 17.00000000000000000, -60.00000000000000000 ) ) ;
#39332 = DIRECTION ( 'NONE',  ( 1.000000000000000000, -0.000000000000000000, 0.000000000000000000 ) ) ;
#39333 = ORIENTED_EDGE ( 'NONE', *, *, #37159, .T. ) ;
#39334 = CARTESIAN_POINT ( 'NONE',  ( -0.5107275442771143092, -1.175643901748072873, 9.976582533991681601 ) ) ;
#39335 = DIRECTION ( 'NONE',  ( 1.586032880504786307E-16, -1.654361225106055350E-24, 1.000000000000000000 ) ) ;
#39336 = DIRECTION ( 'NONE',  ( 0.000000000000000000, -1.000000000000000000, -3.186989995019654210E-49 ) ) ;
#39337 = FACE_OUTER_BOUND ( 'NONE', #35636, .T. ) ;
#39338 = AXIS2_PLACEMENT_3D ( 'NONE', #15928, #47431, #35189 ) ;
#39339 = EDGE_CURVE ( 'NONE', #15022, #24864, #24532, .T. ) ;
#39340 = ORIENTED_EDGE ( 'NONE', *, *, #1295, .T. ) ;
#39341 = VERTEX_POINT ( 'NONE', #28774 ) ;
#39342 = PLANE ( 'NONE',  #2951 ) ;
#39343 = CIRCLE ( 'NONE', #17208, 3.750000000000000000 ) ;
#39344 = VERTEX_POINT ( 'NONE', #20311 ) ;
#39345 = CARTESIAN_POINT ( 'NONE',  ( 193.3040265531851105, 1.750000000000010658, -119.1817124430720440 ) ) ;
#39346 = PLANE ( 'NONE',  #30026 ) ;
#39347 = DIRECTION ( 'NONE',  ( 1.110223024625156171E-16, -0.7071067811865474617, 0.7071067811865474617 ) ) ;
#39348 = ORIENTED_EDGE ( 'NONE', *, *, #38753, .T. ) ;
#39349 = CARTESIAN_POINT ( 'NONE',  ( 360.0000000000000000, 175.0000000000000284, -106.0000000000001990 ) ) ;
#39350 = ORIENTED_EDGE ( 'NONE', *, *, #2083, .T. ) ;
#39351 = LINE ( 'NONE', #10863, #33727 ) ;
#39352 = EDGE_CURVE ( 'NONE', #18302, #35538, #28013, .T. ) ;
#39353 = LINE ( 'NONE', #43932, #40690 ) ;
#39354 = LINE ( 'NONE', #46996, #41131 ) ;
#39355 = ADVANCED_FACE ( 'NONE', ( #43647 ), #44150, .T. ) ;
#39356 = ORIENTED_EDGE ( 'NONE', *, *, #23018, .F. ) ;
#39357 = EDGE_CURVE ( 'NONE', #20835, #25904, #21223, .T. ) ;
#39358 = VERTEX_POINT ( 'NONE', #328 ) ;
#39359 = ORIENTED_EDGE ( 'NONE', *, *, #45308, .T. ) ;
#39360 = CARTESIAN_POINT ( 'NONE',  ( 181.0000000000000000, 165.0000000000000000, -340.0000000000001705 ) ) ;
#39361 = EDGE_CURVE ( 'NONE', #35762, #15096, #4672, .T. ) ;
#39362 = CARTESIAN_POINT ( 'NONE',  ( -14.52758583651993618, -8.922352469211071835, 8.953103998512858652 ) ) ;
#39363 = ORIENTED_EDGE ( 'NONE', *, *, #17673, .F. ) ;
#39364 = CARTESIAN_POINT ( 'NONE',  ( -44.94597344681493922, 2.143131898507880377E-16, -80.93171244307204404 ) ) ;
#39366 = ORIENTED_EDGE ( 'NONE', *, *, #42053, .T. ) ;
#39365 = VECTOR ( 'NONE', #6122, 1000.000000000000000 ) ;
#39367 = EDGE_CURVE ( 'NONE', #37516, #15344, #48593, .T. ) ;
#39368 = FACE_OUTER_BOUND ( 'NONE', #32720, .T. ) ;
#39370 = VERTEX_POINT ( 'NONE', #40078 ) ;
#39369 = AXIS2_PLACEMENT_3D ( 'NONE', #25055, #40952, #37382 ) ;
#39371 =( NAMED_UNIT ( * ) SI_UNIT ( $, .STERADIAN. ) SOLID_ANGLE_UNIT ( ) );
#39372 =( BOUNDED_CURVE ( )  B_SPLINE_CURVE ( 3, ( #24585, #27675, #31792, #43569 ),
 .UNSPECIFIED., .F., .F. ) 
 B_SPLINE_CURVE_WITH_KNOTS ( ( 4, 4 ),
 ( 3.141592653589793116, 4.712388980384689674 ),
 .UNSPECIFIED. ) 
 CURVE ( )  GEOMETRIC_REPRESENTATION_ITEM ( )  RATIONAL_B_SPLINE_CURVE ( ( 1.000000000000000000, 0.8047378541243649375, 0.8047378541243649375, 1.000000000000000000 ) ) 
 REPRESENTATION_ITEM ( '' )  );
#39373 = CARTESIAN_POINT ( 'NONE',  ( 33.30402655318503946, 0.000000000000000000, 165.0000000000000000 ) ) ;
#39374 = PLANE ( 'NONE',  #43228 ) ;
#39375 = VECTOR ( 'NONE', #29585, 1000.000000000000000 ) ;
#39376 = VECTOR ( 'NONE', #11151, 1000.000000000000000 ) ;
#39377 = DIRECTION ( 'NONE',  ( -0.000000000000000000, -0.000000000000000000, -1.000000000000000000 ) ) ;
#39378 = CARTESIAN_POINT ( 'NONE',  ( 1.249999999999999778, 0.000000000000000000, 10.00000000000000000 ) ) ;
#39379 = ORIENTED_EDGE ( 'NONE', *, *, #47745, .T. ) ;
#39380 = ORIENTED_EDGE ( 'NONE', *, *, #8363, .F. ) ;
#39382 = VECTOR ( 'NONE', #21468, 1000.000000000000000 ) ;
#39381 = CARTESIAN_POINT ( 'NONE',  ( 0.000000000000000000, 167.0000000000000000, -344.0000000000001705 ) ) ;
#39383 =( BOUNDED_CURVE ( )  B_SPLINE_CURVE ( 3, ( #16454, #24661, #22942, #3698 ),
 .UNSPECIFIED., .F., .F. ) 
 B_SPLINE_CURVE_WITH_KNOTS ( ( 4, 4 ),
 ( 0.000000000000000000, 1.570796326794896558 ),
 .UNSPECIFIED. ) 
 CURVE ( )  GEOMETRIC_REPRESENTATION_ITEM ( )  RATIONAL_B_SPLINE_CURVE ( ( 1.000000000000000000, 0.8047378541243649375, 0.8047378541243649375, 1.000000000000000000 ) ) 
 REPRESENTATION_ITEM ( '' )  );
#39384 = MECHANICAL_DESIGN_GEOMETRIC_PRESENTATION_REPRESENTATION (  '', ( #2467 ), #28698 ) ;
#39385 = CARTESIAN_POINT ( 'NONE',  ( 71.55402655318505367, -1.025126265847089879, -117.4317124430720156 ) ) ;
#39386 = CYLINDRICAL_SURFACE ( 'NONE', #25773, 1.750000000000008438 ) ;
#39387 = VECTOR ( 'NONE', #13805, 1000.000000000000000 ) ;
#39388 = EDGE_CURVE ( 'NONE', #37149, #13307, #20930, .T. ) ;
#39389 = CARTESIAN_POINT ( 'NONE',  ( -14.52758583651993618, -8.922352469211071835, 8.953103998512858652 ) ) ;
#39390 = ORIENTED_EDGE ( 'NONE', *, *, #17073, .F. ) ;
#39391 = CARTESIAN_POINT ( 'NONE',  ( 357.9999999999999432, -165.0000000000001137, -106.0000000000001990 ) ) ;
#39392 =( BOUNDED_CURVE ( )  B_SPLINE_CURVE ( 3, ( #7604, #50649, #4001, #19651 ),
 .UNSPECIFIED., .F., .F. ) 
 B_SPLINE_CURVE_WITH_KNOTS ( ( 4, 4 ),
 ( 0.000000000000000000, 1.570796326794896780 ),
 .UNSPECIFIED. ) 
 CURVE ( )  GEOMETRIC_REPRESENTATION_ITEM ( )  RATIONAL_B_SPLINE_CURVE ( ( 1.000000000000000000, 0.8047378541243649375, 0.8047378541243649375, 1.000000000000000000 ) ) 
 REPRESENTATION_ITEM ( '' )  );
#39393 = DIRECTION ( 'NONE',  ( -0.000000000000000000, -0.000000000000000000, -1.000000000000000000 ) ) ;
#39394 = ORIENTED_EDGE ( 'NONE', *, *, #37900, .F. ) ;
#39395 = EDGE_CURVE ( 'NONE', #39034, #7468, #8271, .T. ) ;
#39396 = EDGE_CURVE ( 'NONE', #38090, #49813, #826, .T. ) ;
#39397 = CARTESIAN_POINT ( 'NONE',  ( 168.9999999999999716, 175.0000000000000284, -356.0000000000001705 ) ) ;
#39398 = CARTESIAN_POINT ( 'NONE',  ( -168.4459734468149463, 0.000000000000000000, 39.06828755692798438 ) ) ;
#39399 = EDGE_CURVE ( 'NONE', #7818, #34262, #23911, .T. ) ;
#39400 = PLANE ( 'NONE',  #6171 ) ;
#39401 = EDGE_CURVE ( 'NONE', #41447, #1049, #26466, .T. ) ;
#39402 = ORIENTED_EDGE ( 'NONE', *, *, #44948, .T. ) ;
#39403 = ORIENTED_EDGE ( 'NONE', *, *, #15864, .F. ) ;
#39404 = DIRECTION ( 'NONE',  ( 0.000000000000000000, -0.000000000000000000, -1.000000000000000000 ) ) ;
#39405 = EDGE_CURVE ( 'NONE', #36736, #23599, #47720, .T. ) ;
#39406 = CARTESIAN_POINT ( 'NONE',  ( 24.39427009665985224, 44.07992421011656603, 8.807470649214879543 ) ) ;
#39407 = AXIS2_PLACEMENT_3D ( 'NONE', #1216, #16862, #33776 ) ;
#39408 = ORIENTED_EDGE ( 'NONE', *, *, #4201, .T. ) ;
#39409 = ORIENTED_EDGE ( 'NONE', *, *, #25215, .T. ) ;
#39410 = DIRECTION ( 'NONE',  ( -1.000000000000000000, 0.000000000000000000, 0.000000000000000000 ) ) ;
#39411 = CARTESIAN_POINT ( 'NONE',  ( -206.6959734468149463, 1.750000000000009992, 0.8182875569279768335 ) ) ;
#39412 = ORIENTED_EDGE ( 'NONE', *, *, #11238, .T. ) ;
#39413 = VERTEX_POINT ( 'NONE', #33149 ) ;
#39414 = VERTEX_POINT ( 'NONE', #29783 ) ;
#39415 = VECTOR ( 'NONE', #5255, 1000.000000000000000 ) ;
#39416 = CIRCLE ( 'NONE', #70, 2.000000000000001776 ) ;
#39417 = FACE_OUTER_BOUND ( 'NONE', #28482, .T. ) ;
#39418 = ORIENTED_EDGE ( 'NONE', *, *, #33616, .T. ) ;
#39419 = CARTESIAN_POINT ( 'NONE',  ( 7.576114424932982594, -33.14742743729794938, 7.906207997025717304 ) ) ;
#39420 = EDGE_CURVE ( 'NONE', #4890, #30787, #17729, .T. ) ;
#39421 = PLANE ( 'NONE',  #18375 ) ;
#39422 = DIRECTION ( 'NONE',  ( 1.000000000000000000, 0.000000000000000000, 0.000000000000000000 ) ) ;
#39423 = VERTEX_POINT ( 'NONE', #1829 ) ;
#39424 = VERTEX_POINT ( 'NONE', #6425 ) ;
#39425 = CYLINDRICAL_SURFACE ( 'NONE', #14774, 1.750000000000036193 ) ;
#39426 = CARTESIAN_POINT ( 'NONE',  ( 1.011271242968688311, -0.7347315653655855927, -10.00000000000000000 ) ) ;
#39427 = DIRECTION ( 'NONE',  ( -1.000000000000000000, -0.000000000000000000, -0.000000000000000000 ) ) ;
#39428 = EDGE_LOOP ( 'NONE', ( #46732, #221, #44838, #28653 ) ) ;
#39429 = ORIENTED_EDGE ( 'NONE', *, *, #8410, .F. ) ;
#39430 = CARTESIAN_POINT ( 'NONE',  ( 16.02661358026014327, 4.530191650547718218, -9.683996418299976483 ) ) ;
#39431 = DIRECTION ( 'NONE',  ( -1.000000000000000000, -0.000000000000000000, -0.000000000000000000 ) ) ;
#39432 = ORIENTED_EDGE ( 'NONE', *, *, #37787, .T. ) ;
#39433 = CARTESIAN_POINT ( 'NONE',  ( -6.695973446814940111, 0.000000000000000000, 165.0000000000000000 ) ) ;
#39434 = DIRECTION ( 'NONE',  ( -1.587271980518778491E-16, 5.169878828456422968E-26, 1.000000000000000000 ) ) ;
#39435 = FACE_OUTER_BOUND ( 'NONE', #30383, .T. ) ;
#39436 = CARTESIAN_POINT ( 'NONE',  ( 30.25247992116058526, -39.82368563463805344, -3.760136334089591248 ) ) ;
#39437 = ORIENTED_EDGE ( 'NONE', *, *, #6631, .F. ) ;
#39438 = EDGE_CURVE ( 'NONE', #16814, #47750, #9517, .T. ) ;
#39439 = CARTESIAN_POINT ( 'NONE',  ( -0.5113015165352315927, -1.175527691268679398, 9.948547179989621014 ) ) ;
#39440 = DIRECTION ( 'NONE',  ( -0.000000000000000000, -0.000000000000000000, -1.000000000000000000 ) ) ;
#39441 = VECTOR ( 'NONE', #11899, 1000.000000000000000 ) ;
#39442 = CARTESIAN_POINT ( 'NONE',  ( -7.721099712662037540, 1.750000000000022427, 1.843413822775074040 ) ) ;
#39443 = DIRECTION ( 'NONE',  ( 1.000000000000000000, 0.000000000000000000, 0.000000000000000000 ) ) ;
#39444 = CARTESIAN_POINT ( 'NONE',  ( -16.52264463346130796, 2.779753662172870232, 9.403735324607438884 ) ) ;
#39445 = VECTOR ( 'NONE', #22950, 1000.000000000000000 ) ;
#39446 = CARTESIAN_POINT ( 'NONE',  ( 164.9999999999999716, 16.00000000000000000, 115.0000000000000142 ) ) ;
#39447 = ORIENTED_EDGE ( 'NONE', *, *, #255, .F. ) ;
#39448 = DIRECTION ( 'NONE',  ( -1.000000000000000000, 0.000000000000000000, 0.000000000000000000 ) ) ;
#39449 = ADVANCED_FACE ( 'NONE', ( #45649 ), #13621, .F. ) ;
#39450 = EDGE_CURVE ( 'NONE', #25022, #11648, #32892, .T. ) ;
#39451 = CARTESIAN_POINT ( 'NONE',  ( 340.0000000000000568, 169.0000000000000000, 355.9999999999997726 ) ) ;
#39452 = ORIENTED_EDGE ( 'NONE', *, *, #24046, .T. ) ;
#39453 = CARTESIAN_POINT ( 'NONE',  ( 80.00000000000186162, 17.00000000000000000, 65.00000000000000000 ) ) ;
#39454 = DIRECTION ( 'NONE',  ( -1.000000000000000000, 0.000000000000000000, -0.000000000000000000 ) ) ;
#39455 = CARTESIAN_POINT ( 'NONE',  ( -3.951902932896436571, -0.4322042056279351008, 3.247138655587367140 ) ) ;
#39456 = EDGE_CURVE ( 'NONE', #43496, #30589, #10029, .T. ) ;
#39457 = ORIENTED_EDGE ( 'NONE', *, *, #18103, .F. ) ;
#39458 = CARTESIAN_POINT ( 'NONE',  ( -124.9459734468149321, -1.025126265847081664, -37.43171244307203693 ) ) ;
#39459 = ORIENTED_EDGE ( 'NONE', *, *, #31562, .F. ) ;
#39460 = ORIENTED_EDGE ( 'NONE', *, *, #22357, .T. ) ;
#39461 = CARTESIAN_POINT ( 'NONE',  ( 85.00000000000029843, 16.00000000000000000, -84.99999999999998579 ) ) ;
#39462 = EDGE_CURVE ( 'NONE', #29622, #2364, #36997, .T. ) ;
#39463 = DIRECTION ( 'NONE',  ( -1.000000000000000000, 0.000000000000000000, -2.958228394578794270E-31 ) ) ;
#39464 = EDGE_CURVE ( 'NONE', #11195, #21418, #15990, .T. ) ;
#39465 = VERTEX_POINT ( 'NONE', #36754 ) ;
#39466 = CARTESIAN_POINT ( 'NONE',  ( 0.000000000000000000, 50.00000000000002132, 800.0000000000000000 ) ) ;
#39467 = DIRECTION ( 'NONE',  ( 0.000000000000000000, 0.000000000000000000, -1.000000000000000000 ) ) ;
#39468 =( BOUNDED_CURVE ( )  B_SPLINE_CURVE ( 3, ( #14719, #42160, #22669, #16746 ),
 .UNSPECIFIED., .F., .F. ) 
 B_SPLINE_CURVE_WITH_KNOTS ( ( 4, 4 ),
 ( 4.712388980384689674, 6.283185307179586232 ),
 .UNSPECIFIED. ) 
 CURVE ( )  GEOMETRIC_REPRESENTATION_ITEM ( )  RATIONAL_B_SPLINE_CURVE ( ( 1.000000000000000000, 0.8047378541243649375, 0.8047378541243649375, 1.000000000000000000 ) ) 
 REPRESENTATION_ITEM ( '' )  );
#39469 = EDGE_CURVE ( 'NONE', #37195, #32609, #42195, .T. ) ;
#39470 = CARTESIAN_POINT ( 'NONE',  ( 1.655785408456140084, 0.7536129375913136474, 9.903764339332061795 ) ) ;
#39471 = ORIENTED_EDGE ( 'NONE', *, *, #36410, .T. ) ;
#39472 = VECTOR ( 'NONE', #30507, 1000.000000000000000 ) ;
#39473 = FACE_OUTER_BOUND ( 'NONE', #23179, .T. ) ;
#39474 = LINE ( 'NONE', #40474, #12726 ) ;
#39475 = PRESENTATION_STYLE_ASSIGNMENT (( #11755 ) ) ;
#39476 = ORIENTED_EDGE ( 'NONE', *, *, #22067, .T. ) ;
#39477 = CARTESIAN_POINT ( 'NONE',  ( 210.0000000000000568, 0.000000000000000000, -39.18171244307202983 ) ) ;
#39478 = LINE ( 'NONE', #15858, #49836 ) ;
#39479 = MANIFOLD_SOLID_BREP ( 'Boss-Extrude3', #45729 ) ;
#39480 = ORIENTED_EDGE ( 'NONE', *, *, #16414, .F. ) ;
#39481 = ORIENTED_EDGE ( 'NONE', *, *, #48034, .T. ) ;
#39482 = ORIENTED_EDGE ( 'NONE', *, *, #50701, .T. ) ;
#39483 = DIRECTION ( 'NONE',  ( 0.000000000000000000, 0.000000000000000000, 1.000000000000000000 ) ) ;
#39484 = CARTESIAN_POINT ( 'NONE',  ( 168.9999999999999716, -184.9999999999999716, -344.0000000000001137 ) ) ;
#39485 = AXIS2_PLACEMENT_3D ( 'NONE', #4906, #1076, #827 ) ;
#39486 = EDGE_LOOP ( 'NONE', ( #41214, #47672, #32785, #44145 ) ) ;
#39487 = CARTESIAN_POINT ( 'NONE',  ( 4.204997580903516941, -7.388441598285492518, 225.0000000000000000 ) ) ;
#39488 = DIRECTION ( 'NONE',  ( -0.000000000000000000, -1.000000000000000000, -0.000000000000000000 ) ) ;
#39489 = LINE ( 'NONE', #19717, #22269 ) ;
#39490 = CARTESIAN_POINT ( 'NONE',  ( -225.0000000000000568, -153.6999999999999602, 254.8599999999999852 ) ) ;
#39491 = CARTESIAN_POINT ( 'NONE',  ( -389.0218519071287346, 0.000000000000000000, 192.5658166940287970 ) ) ;
#39492 = FACE_OUTER_BOUND ( 'NONE', #31371, .T. ) ;
#39493 = CARTESIAN_POINT ( 'NONE',  ( -5.083187235775261215, -8.611690166631138510, 9.646707543097347681 ) ) ;
#39494 = DIRECTION ( 'NONE',  ( -0.000000000000000000, -0.000000000000000000, -1.000000000000000000 ) ) ;
#39495 = CARTESIAN_POINT ( 'NONE',  ( -0.2050626648094178439, 1.807624707194796843, 9.903764339332081335 ) ) ;
#39496 = DIRECTION ( 'NONE',  ( -0.000000000000000000, -0.000000000000000000, -1.000000000000000000 ) ) ;
#39497 = CARTESIAN_POINT ( 'NONE',  ( 358.0000000000001137, 169.0000000000000000, 349.9999999999998863 ) ) ;
#39498 = EDGE_CURVE ( 'NONE', #20980, #19783, #1899, .T. ) ;
#39499 = CARTESIAN_POINT ( 'NONE',  ( 167.0000000000000284, 165.0000000000000000, 355.9999999999998863 ) ) ;
#39500 = CARTESIAN_POINT ( 'NONE',  ( 0.000000000000000000, 165.0000000000000000, -356.0000000000002274 ) ) ;
#39501 = CARTESIAN_POINT ( 'NONE',  ( -204.9459734468148895, -1.025126265847089435, 39.06828755692797728 ) ) ;
#39502 = CARTESIAN_POINT ( 'NONE',  ( -49.75871208702130133, 40.58472229863599523, 5.000000000000000000 ) ) ;
#39503 = ORIENTED_EDGE ( 'NONE', *, *, #536, .T. ) ;
#39504 = CARTESIAN_POINT ( 'NONE',  ( -164.9999999999984936, 17.00000000000000000, 60.00000000000000000 ) ) ;
#39505 = AXIS2_PLACEMENT_3D ( 'NONE', #45422, #5695, #45168 ) ;
#39506 = CARTESIAN_POINT ( 'NONE',  ( 130.0000000000012221, 17.00000000000000000, 5.000000000000004441 ) ) ;
#39507 = CARTESIAN_POINT ( 'NONE',  ( 4.632259372452904422, -3.749670805219074143, 1.768604793866979108E-15 ) ) ;
#39508 = CARTESIAN_POINT ( 'NONE',  ( -33.43156050989129824, 4.370686678976795747, 8.807470649214879543 ) ) ;
#39509 = ORIENTED_EDGE ( 'NONE', *, *, #15787, .T. ) ;
#39510 = ORIENTED_EDGE ( 'NONE', *, *, #19266, .T. ) ;
#39511 = EDGE_CURVE ( 'NONE', #2812, #38442, #7142, .T. ) ;
#39512 = AXIS2_PLACEMENT_3D ( 'NONE', #40380, #8575, #12656 ) ;
#39513 = LINE ( 'NONE', #43086, #46626 ) ;
#39514 = ORIENTED_EDGE ( 'NONE', *, *, #25089, .T. ) ;
#39515 = CARTESIAN_POINT ( 'NONE',  ( 193.3040265531851105, -1.750000000000009992, 0.8182875569279768335 ) ) ;
#39516 = DIRECTION ( 'NONE',  ( -0.000000000000000000, -1.000000000000000000, -0.000000000000000000 ) ) ;
#39517 = ORIENTED_EDGE ( 'NONE', *, *, #20547, .F. ) ;
#39518 = DIRECTION ( 'NONE',  ( -0.4740998230350174647, -0.3386427307392981256, -0.8127425537743155903 ) ) ;
#39519 = EDGE_LOOP ( 'NONE', ( #4520, #20717, #12152, #33620 ) ) ;
#39520 = EDGE_CURVE ( 'NONE', #5419, #31711, #41829, .T. ) ;
#39521 = ADVANCED_FACE ( 'NONE', ( #38511 ), #34917, .T. ) ;
#39522 =( BOUNDED_CURVE ( )  B_SPLINE_CURVE ( 3, ( #30768, #46379, #34881, #26904 ),
 .UNSPECIFIED., .F., .F. ) 
 B_SPLINE_CURVE_WITH_KNOTS ( ( 4, 4 ),
 ( 4.712388980384689674, 6.283185307179586232 ),
 .UNSPECIFIED. ) 
 CURVE ( )  GEOMETRIC_REPRESENTATION_ITEM ( )  RATIONAL_B_SPLINE_CURVE ( ( 1.000000000000000000, 0.8047378541243649375, 0.8047378541243649375, 1.000000000000000000 ) ) 
 REPRESENTATION_ITEM ( '' )  );
#39523 = VERTEX_POINT ( 'NONE', #15647 ) ;
#39524 = CARTESIAN_POINT ( 'NONE',  ( 164.9999999999999716, -184.9999999999999716, -344.0000000000006253 ) ) ;
#39525 = CARTESIAN_POINT ( 'NONE',  ( 339.9999999999999432, -166.6568542494925396, -341.6568542494925396 ) ) ;
#39526 = ORIENTED_EDGE ( 'NONE', *, *, #23807, .T. ) ;
#39527 = CARTESIAN_POINT ( 'NONE',  ( 31.55402655318503236, 0.000000000000000000, -117.4317124430720156 ) ) ;
#39528 = LINE ( 'NONE', #773, #39003 ) ;
#39529 = EDGE_CURVE ( 'NONE', #28572, #37476, #14629, .T. ) ;
#39530 = LINE ( 'NONE', #43603, #19991 ) ;
#39531 = B_SPLINE_CURVE_WITH_KNOTS ( 'NONE', 3,
 ( #8389, #4533, #30987, #46334 ),
 .UNSPECIFIED., .F., .F.,
 ( 4, 4 ),
 ( 0.9895749839358303213, 1.000000000000000000 ),
 .UNSPECIFIED. ) ;
#39532 =( BOUNDED_CURVE ( )  B_SPLINE_CURVE ( 3, ( #17224, #28523, #29022, #824 ),
 .UNSPECIFIED., .F., .F. ) 
 B_SPLINE_CURVE_WITH_KNOTS ( ( 4, 4 ),
 ( 4.712388980384689674, 6.283185307179586232 ),
 .UNSPECIFIED. ) 
 CURVE ( )  GEOMETRIC_REPRESENTATION_ITEM ( )  RATIONAL_B_SPLINE_CURVE ( ( 1.000000000000000000, 0.8047378541243649375, 0.8047378541243649375, 1.000000000000000000 ) ) 
 REPRESENTATION_ITEM ( '' )  );
#39533 = CARTESIAN_POINT ( 'NONE',  ( -88.44597344681491791, 0.000000000000000000, 162.5682875569279702 ) ) ;
#39534 = DIRECTION ( 'NONE',  ( -0.000000000000000000, -1.000000000000000000, -0.000000000000000000 ) ) ;
#39535 = ORIENTED_EDGE ( 'NONE', *, *, #7117, .T. ) ;
#39536 = CARTESIAN_POINT ( 'NONE',  ( 151.5540265531850537, 1.025126265847089435, 82.56828755692798438 ) ) ;
#39537 = DIRECTION ( 'NONE',  ( -1.000000000000000000, 0.000000000000000000, 0.000000000000000000 ) ) ;
#39538 = PRESENTATION_LAYER_ASSIGNMENT (  '', '', ( #45229 ) ) ;
#39539 = VERTEX_POINT ( 'NONE', #23341 ) ;
#39540 = PLANE ( 'NONE',  #39338 ) ;
#39541 = VECTOR ( 'NONE', #1246, 1000.000000000000000 ) ;
#39542 = DIRECTION ( 'NONE',  ( 0.000000000000000000, -0.000000000000000000, 1.000000000000000000 ) ) ;
#39543 = ORIENTED_EDGE ( 'NONE', *, *, #32494, .F. ) ;
#39544=STYLED_ITEM('',(#50747),#38125);
#39545 = CYLINDRICAL_SURFACE ( 'NONE', #2153, 1.750000000000015543 ) ;
#39546 = FACE_OUTER_BOUND ( 'NONE', #15250, .T. ) ;
#39547 = DIRECTION ( 'NONE',  ( -0.000000000000000000, -1.000000000000000000, -0.000000000000000000 ) ) ;
#39548 = CARTESIAN_POINT ( 'NONE',  ( 0.3904210042914120771, -2.126747006146346930, 9.882710035074770971 ) ) ;
#39549 = AXIS2_PLACEMENT_3D ( 'NONE', #32081, #46918, #35439 ) ;
#39550 = ORIENTED_EDGE ( 'NONE', *, *, #13057, .F. ) ;
#39551 = DIRECTION ( 'NONE',  ( 0.000000000000000000, 0.000000000000000000, 1.000000000000000000 ) ) ;
#39552 = CARTESIAN_POINT ( 'NONE',  ( -2.052549611693787135, 0.2039603569406744088, 9.894754715216729224 ) ) ;
#39553 = CARTESIAN_POINT ( 'NONE',  ( 164.9999999999999716, 17.00000000000000000, 95.00000000000000000 ) ) ;
#39554 = ORIENTED_EDGE ( 'NONE', *, *, #39801, .F. ) ;
#39555 = EDGE_CURVE ( 'NONE', #47169, #35315, #19959, .T. ) ;
#39556 = ORIENTED_EDGE ( 'NONE', *, *, #1892, .T. ) ;
#39557 = CARTESIAN_POINT ( 'NONE',  ( 718.1651790843212666, 792.7343818613097710, 2038.209884924934386 ) ) ;
#39558 = DIRECTION ( 'NONE',  ( -0.000000000000000000, -1.000000000000000000, -0.000000000000000000 ) ) ;
#39559 = DIRECTION ( 'NONE',  ( -1.586032892321652236E-16, -1.000000000000000000, -6.853681917100419162E-49 ) ) ;
#39560 = CARTESIAN_POINT ( 'NONE',  ( -12.15085308559838317, 11.68662139125813226, 2.590526750877053086 ) ) ;
#39561 = MANIFOLD_SOLID_BREP ( 'Square tube 20 X 20 X 2(1)[13]', #43305 ) ;
#39562 = CARTESIAN_POINT ( 'NONE',  ( 155.0540265531850537, 2.143131898507880377E-16, -160.9317124430720014 ) ) ;
#39563 = EDGE_LOOP ( 'NONE', ( #37873, #31237, #30284, #49268, #19938, #38069 ) ) ;
#39564 = CARTESIAN_POINT ( 'NONE',  ( -114.9999999999984652, 16.00000000000000000, 60.00000000000000000 ) ) ;
#39565 = VECTOR ( 'NONE', #39347, 1000.000000000000114 ) ;
#39566 = CARTESIAN_POINT ( 'NONE',  ( -167.7210997126620384, 1.750000000000009548, -78.15658617722490931 ) ) ;
#39567 = CARTESIAN_POINT ( 'NONE',  ( 2.052549611693792464, -0.2039603569406628347, 9.894754715216725671 ) ) ;
#39568 = VERTEX_POINT ( 'NONE', #39014 ) ;
#39569 = FACE_BOUND ( 'NONE', #27322, .T. ) ;
#39570 = ORIENTED_EDGE ( 'NONE', *, *, #23345, .T. ) ;
#39571 = CARTESIAN_POINT ( 'NONE',  ( 339.9999999999999432, 169.0000000000001705, -344.0000000000002842 ) ) ;
#39572 = PRESENTATION_LAYER_ASSIGNMENT (  '', '', ( #33013 ) ) ;
#39573 = ORIENTED_EDGE ( 'NONE', *, *, #35644, .T. ) ;
#39574 = CARTESIAN_POINT ( 'NONE',  ( -124.9459734468149463, 2.143131898507847836E-16, -0.9317124430719969652 ) ) ;
#39575 = VECTOR ( 'NONE', #41745, 1000.000000000000000 ) ;
#39576 = DIRECTION ( 'NONE',  ( 1.000000000000000000, 0.000000000000000000, 0.000000000000000000 ) ) ;
#39577 = CARTESIAN_POINT ( 'NONE',  ( 75.05402655318509630, -1.025126265847089213, 42.56828755692799149 ) ) ;
#39578 = CARTESIAN_POINT ( 'NONE',  ( 210.0000000000000568, 0.000000000000000000, -79.18171244307201562 ) ) ;
#39579 = ORIENTED_EDGE ( 'NONE', *, *, #24604, .F. ) ;
#39580 = AXIS2_PLACEMENT_3D ( 'NONE', #43329, #4097, #12540 ) ;
#39581 = CARTESIAN_POINT ( 'NONE',  ( -4.207128120815918256E-14, 3.058192377181588826E-14, 10.00000000000000000 ) ) ;
#39582 = AXIS2_PLACEMENT_3D ( 'NONE', #41032, #5876, #37214 ) ;
#39583 = CARTESIAN_POINT ( 'NONE',  ( 165.0000000000000000, 2.775557561562891351E-14, -99.00000000000014211 ) ) ;
#39584 = ORIENTED_EDGE ( 'NONE', *, *, #7076, .F. ) ;
#39585 = FACE_OUTER_BOUND ( 'NONE', #24766, .T. ) ;
#39586 = PLANE ( 'NONE',  #12586 ) ;
#39587 = DIRECTION ( 'NONE',  ( -1.000000000000000000, -0.000000000000000000, -0.000000000000000000 ) ) ;
#39588 = FACE_OUTER_BOUND ( 'NONE', #6668, .T. ) ;
#39589 = EDGE_CURVE ( 'NONE', #13970, #22765, #18978, .T. ) ;
#39590 = EDGE_LOOP ( 'NONE', ( #25196, #3305, #25083, #15151, #26327, #46485 ) ) ;
#39591 = EDGE_LOOP ( 'NONE', ( #26061, #45675, #12838, #11605, #16554 ) ) ;
#39592 = DIRECTION ( 'NONE',  ( 1.000000000000000000, 0.000000000000000000, 0.000000000000000000 ) ) ;
#39593 = ORIENTED_EDGE ( 'NONE', *, *, #44364, .T. ) ;
#39594 = CARTESIAN_POINT ( 'NONE',  ( 153.3040265531850537, -1.750000000000010658, 80.81828755692798438 ) ) ;
#39595 = CARTESIAN_POINT ( 'NONE',  ( 210.0000000000000568, 0.000000000000000000, 82.56828755692799859 ) ) ;
#39596 = ORIENTED_EDGE ( 'NONE', *, *, #45325, .T. ) ;
#39597 = CARTESIAN_POINT ( 'NONE',  ( -8.831420117243776957, -14.12636088103186260, -3.546734833711462365 ) ) ;
#39598 = ORIENTED_EDGE ( 'NONE', *, *, #37821, .T. ) ;
#39599 = B_SPLINE_CURVE_WITH_KNOTS ( 'NONE', 3,
 ( #7597, #19891, #30961, #42982, #46546, #23231 ),
 .UNSPECIFIED., .F., .F.,
 ( 4, 2, 4 ),
 ( 4.629632144690684174E-17, 0.009882509389272370673, 0.01976501877854469624 ),
 .UNSPECIFIED. ) ;
#39600 = EDGE_CURVE ( 'NONE', #11492, #20673, #22582, .T. ) ;
#39601 = LINE ( 'NONE', #36265, #19359 ) ;
#39602 = LINE ( 'NONE', #3931, #17329 ) ;
#39603 = ORIENTED_EDGE ( 'NONE', *, *, #24576, .T. ) ;
#39604 = ORIENTED_EDGE ( 'NONE', *, *, #17733, .F. ) ;
#39605 = AXIS2_PLACEMENT_3D ( 'NONE', #1013, #29216, #40018 ) ;
#39606 = EDGE_LOOP ( 'NONE', ( #46539, #33467, #17863, #26706 ) ) ;
#39607 = CARTESIAN_POINT ( 'NONE',  ( 183.0000000000000000, -93.49999999999998579, -350.0000000000001705 ) ) ;
#39608 = CARTESIAN_POINT ( 'NONE',  ( 114.3291528190321173, -1.749999999999996669, -118.1565861772249661 ) ) ;
#39609 = VECTOR ( 'NONE', #29383, 1000.000000000000000 ) ;
#39610 = DIRECTION ( 'NONE',  ( -0.000000000000000000, -1.000000000000000000, -0.000000000000000000 ) ) ;
#39611 = PRODUCT_DEFINITION_CONTEXT ( 'detailed design', #4994, 'design' ) ;
#39612 = ORIENTED_EDGE ( 'NONE', *, *, #1719, .T. ) ;
#39613 = EDGE_CURVE ( 'NONE', #34689, #20602, #50492, .T. ) ;
#39614 = ORIENTED_EDGE ( 'NONE', *, *, #9676, .T. ) ;
#39615 = CARTESIAN_POINT ( 'NONE',  ( 9.563755223200855582, 2.971660568388050372, 3.215106848023521646 ) ) ;
#39616 = ORIENTED_EDGE ( 'NONE', *, *, #13352, .T. ) ;
#39617 = DIRECTION ( 'NONE',  ( 0.000000000000000000, 0.000000000000000000, 1.000000000000000000 ) ) ;
#39618 = CARTESIAN_POINT ( 'NONE',  ( -114.9999999999987779, 17.00000000000000000, 5.000000000000004441 ) ) ;
#39619 = LINE ( 'NONE', #15257, #35733 ) ;
#39620 = VECTOR ( 'NONE', #8449, 1000.000000000000000 ) ;
#39621 = CARTESIAN_POINT ( 'NONE',  ( -2.538055338523177440, -33.28424297489108596, -9.367992836599954742 ) ) ;
#39622 = DIRECTION ( 'NONE',  ( -1.586032892321652482E-16, 0.000000000000000000, -1.000000000000000000 ) ) ;
#39623 = ORIENTED_EDGE ( 'NONE', *, *, #1325, .T. ) ;
#39624 = ORIENTED_EDGE ( 'NONE', *, *, #36629, .T. ) ;
#39625 = FACE_OUTER_BOUND ( 'NONE', #42850, .T. ) ;
#39626 = B_SPLINE_SURFACE_WITH_KNOTS ( 'NONE', 3, 3, ( 
 ( #14724, #33983, #48820, #45736 ),
 ( #10873, #30386, #26530, #42169 ),
 ( #13710, #362, #39362, #35516 ),
 ( #46244, #38349, #23183, #3421 ) ),
 .UNSPECIFIED., .F., .F., .F.,
 ( 4, 4 ),
 ( 4, 4 ),
 ( 0.000000000000000000, 1.000000000000000000 ),
 ( 0.000000000000000000, 1.000000000000000000 ),
 .UNSPECIFIED. ) ;
#39627 = DIRECTION ( 'NONE',  ( -0.000000000000000000, -0.000000000000000000, -1.000000000000000000 ) ) ;
#39628 = DIRECTION ( 'NONE',  ( 0.000000000000000000, 1.000000000000000000, 0.000000000000000000 ) ) ;
#39629 = CARTESIAN_POINT ( 'NONE',  ( 344.0000000000000000, -165.0000000000001137, -94.00000000000019895 ) ) ;
#39630 = ORIENTED_EDGE ( 'NONE', *, *, #25021, .T. ) ;
#39631 = DIRECTION ( 'NONE',  ( 6.765175596986472868E-16, -0.9749645535258953943, 0.2223603367690637489 ) ) ;
#39632 = CARTESIAN_POINT ( 'NONE',  ( -168.4459734468149747, 1.025126265847089657, 119.0682875569279560 ) ) ;
#39633 = ORIENTED_EDGE ( 'NONE', *, *, #31688, .F. ) ;
#39634 = EDGE_CURVE ( 'NONE', #1914, #26837, #46905, .T. ) ;
#39635 = ADVANCED_FACE ( 'NONE', ( #18476 ), #38265, .T. ) ;
#39636 = DIRECTION ( 'NONE',  ( 1.000000000000000000, -1.586032892321652236E-16, -1.586032892321651989E-16 ) ) ;
#39637 = MANIFOLD_SOLID_BREP ( 'Square tube 20 X 20 X 2(1)[2]', #8090 ) ;
#39638 = VECTOR ( 'NONE', #9463, 1000.000000000000000 ) ;
#39639 = DIRECTION ( 'NONE',  ( -6.765175596986471882E-16, 0.9749645535258953943, -0.2223603367690637489 ) ) ;
#39640 = FACE_OUTER_BOUND ( 'NONE', #41940, .T. ) ;
#39641 = EDGE_CURVE ( 'NONE', #12244, #17553, #1273, .T. ) ;
#39642 = ORIENTED_EDGE ( 'NONE', *, *, #37210, .T. ) ;
#39643 = ORIENTED_EDGE ( 'NONE', *, *, #35566, .T. ) ;
#39644 = CARTESIAN_POINT ( 'NONE',  ( 169.0000000000000000, -174.9999999999999716, -97.00000000000014211 ) ) ;
#39645 = AXIS2_PLACEMENT_3D ( 'NONE', #38759, #45895, #3844 ) ;
#39646 = EDGE_CURVE ( 'NONE', #48914, #39055, #26694, .T. ) ;
#39647 = FACE_OUTER_BOUND ( 'NONE', #22569, .T. ) ;
#39648 = AXIS2_PLACEMENT_3D ( 'NONE', #32805, #24098, #16636 ) ;
#39649 = EDGE_CURVE ( 'NONE', #7223, #13192, #16922, .T. ) ;
#39650 = VERTEX_POINT ( 'NONE', #47162 ) ;
#39651 = VERTEX_POINT ( 'NONE', #24373 ) ;
#39652 = CARTESIAN_POINT ( 'NONE',  ( 195.0540265531851105, 2.143131898507880377E-16, -117.4317124430720725 ) ) ;
#39653 = CARTESIAN_POINT ( 'NONE',  ( -0.8101545402525901496, -3.892041480676482479, 3.247138655587363587 ) ) ;
#39654 = CARTESIAN_POINT ( 'NONE',  ( -6.875132362119187768, 50.00000000000000711, 8.356839323120299312 ) ) ;
#39655 = CARTESIAN_POINT ( 'NONE',  ( 344.0000000000000000, -174.9999999999999716, 343.9999999999998295 ) ) ;
#39656 = CARTESIAN_POINT ( 'NONE',  ( -126.6959734468149321, 1.749999999999996891, -159.1817124430720298 ) ) ;
#39657 = ORIENTED_EDGE ( 'NONE', *, *, #21247, .T. ) ;
#39658 = ORIENTED_EDGE ( 'NONE', *, *, #23850, .T. ) ;
#39659 = VERTEX_POINT ( 'NONE', #28215 ) ;
#39660 = CARTESIAN_POINT ( 'NONE',  ( 0.1287570809895604018, 0.3962735484563146282, 10.00000000000000000 ) ) ;
#39661 =( BOUNDED_CURVE ( )  B_SPLINE_CURVE ( 3, ( #34792, #11670, #7836, #27323 ),
 .UNSPECIFIED., .F., .F. ) 
 B_SPLINE_CURVE_WITH_KNOTS ( ( 4, 4 ),
 ( 4.712388980384689674, 6.283185307179586232 ),
 .UNSPECIFIED. ) 
 CURVE ( )  GEOMETRIC_REPRESENTATION_ITEM ( )  RATIONAL_B_SPLINE_CURVE ( ( 1.000000000000000000, 0.8047378541243649375, 0.8047378541243649375, 1.000000000000000000 ) ) 
 REPRESENTATION_ITEM ( '' )  );
#39662 = ORIENTED_EDGE ( 'NONE', *, *, #20610, .F. ) ;
#39663 = DIRECTION ( 'NONE',  ( -1.000000000000000000, 0.000000000000000000, 0.000000000000000000 ) ) ;
#39664 = ORIENTED_EDGE ( 'NONE', *, *, #27088, .T. ) ;
#39665 = ORIENTED_EDGE ( 'NONE', *, *, #30598, .F. ) ;
#39666 = CARTESIAN_POINT ( 'NONE',  ( 350.0000000000000000, 181.0000000000000284, -356.0000000000002274 ) ) ;
#39668 = CARTESIAN_POINT ( 'NONE',  ( 1.011271242968688311, -0.7347315653655855927, 3.333333333333333481 ) ) ;
#39667 =( BOUNDED_CURVE ( )  B_SPLINE_CURVE ( 3, ( #9813, #10571, #25476, #38046 ),
 .UNSPECIFIED., .F., .F. ) 
 B_SPLINE_CURVE_WITH_KNOTS ( ( 4, 4 ),
 ( 0.000000000000000000, 1.570796326794896558 ),
 .UNSPECIFIED. ) 
 CURVE ( )  GEOMETRIC_REPRESENTATION_ITEM ( )  RATIONAL_B_SPLINE_CURVE ( ( 1.000000000000000000, 0.8047378541243649375, 0.8047378541243649375, 1.000000000000000000 ) ) 
 REPRESENTATION_ITEM ( '' )  );
#39669 = CARTESIAN_POINT ( 'NONE',  ( 193.3040265531851105, 1.750000000000010658, -119.1817124430720440 ) ) ;
#39670 = VERTEX_POINT ( 'NONE', #27705 ) ;
#39671 = EDGE_CURVE ( 'NONE', #5729, #37149, #8214, .T. ) ;
#39672 = EDGE_CURVE ( 'NONE', #6245, #46611, #17625, .T. ) ;
#39673 = ORIENTED_EDGE ( 'NONE', *, *, #48073, .F. ) ;
#39674 = CARTESIAN_POINT ( 'NONE',  ( 210.0000000000000568, 0.000000000000000000, 122.5682875569279844 ) ) ;
#39675 = CARTESIAN_POINT ( 'NONE',  ( 183.0000000000000284, -174.9999999999999716, -99.00000000000014211 ) ) ;
#39676 = VERTEX_POINT ( 'NONE', #43093 ) ;
#39677 = EDGE_CURVE ( 'NONE', #27283, #39414, #522, .T. ) ;
#39678 = DIRECTION ( 'NONE',  ( 0.000000000000000000, -0.3846153846153845812, -0.9230769230769231282 ) ) ;
#39679 = FACE_OUTER_BOUND ( 'NONE', #41573, .T. ) ;
#39680 = DIRECTION ( 'NONE',  ( 0.000000000000000000, 0.000000000000000000, -1.000000000000000000 ) ) ;
#39681 = EDGE_CURVE ( 'NONE', #47520, #8172, #16651, .T. ) ;
#39682 = VECTOR ( 'NONE', #50503, 1000.000000000000000 ) ;
#39683 = LINE ( 'NONE', #34830, #46199 ) ;
#39684 = ORIENTED_EDGE ( 'NONE', *, *, #42110, .T. ) ;
#39685 = EDGE_CURVE ( 'NONE', #10108, #45431, #7962, .T. ) ;
#39686 = AXIS2_PLACEMENT_3D ( 'NONE', #13362, #1581, #41077 ) ;
#39687 = CARTESIAN_POINT ( 'NONE',  ( 1.011271242968683648, 0.7347315653655930312, 10.00000000000000000 ) ) ;
#39688 = ADVANCED_FACE ( 'NONE', ( #19748 ), #47912, .F. ) ;
#39689 = DIRECTION ( 'NONE',  ( -1.000000000000000000, -0.000000000000000000, -0.000000000000000000 ) ) ;
#39690 =( BOUNDED_CURVE ( )  B_SPLINE_CURVE ( 3, ( #46166, #45416, #34178, #15165 ),
 .UNSPECIFIED., .F., .F. ) 
 B_SPLINE_CURVE_WITH_KNOTS ( ( 4, 4 ),
 ( 3.141592653589793116, 4.712388980384689674 ),
 .UNSPECIFIED. ) 
 CURVE ( )  GEOMETRIC_REPRESENTATION_ITEM ( )  RATIONAL_B_SPLINE_CURVE ( ( 1.000000000000000000, 0.8047378541243649375, 0.8047378541243649375, 1.000000000000000000 ) ) 
 REPRESENTATION_ITEM ( '' )  );
#39691 = CARTESIAN_POINT ( 'NONE',  ( 1.011271242968683648, 0.7347315653655930312, -3.333333333333333481 ) ) ;
#39692 = MECHANICAL_DESIGN_GEOMETRIC_PRESENTATION_REPRESENTATION (  '', ( #23252 ), #4438 ) ;
#39693 = FACE_OUTER_BOUND ( 'NONE', #5376, .T. ) ;
#39694 = DIRECTION ( 'NONE',  ( 0.000000000000000000, 0.000000000000000000, 1.000000000000000000 ) ) ;
#39695 = PLANE ( 'NONE',  #4529 ) ;
#39696 = EDGE_CURVE ( 'NONE', #33331, #47564, #23598, .T. ) ;
#39697 = DIRECTION ( 'NONE',  ( 0.000000000000000000, 0.000000000000000000, 1.000000000000000000 ) ) ;
#39698 = EDGE_LOOP ( 'NONE', ( #36691, #10129, #44869, #30656 ) ) ;
#39699 = LINE ( 'NONE', #31242, #18264 ) ;
#39700 = AXIS2_PLACEMENT_3D ( 'NONE', #7166, #29312, #2119 ) ;
#39701 = EDGE_CURVE ( 'NONE', #5897, #23745, #44617, .T. ) ;
#39702 = ADVANCED_FACE ( 'NONE', ( #4104 ), #35683, .T. ) ;
#39703 = CARTESIAN_POINT ( 'NONE',  ( -88.44597344681497475, 0.000000000000000000, -0.9317124430720524764 ) ) ;
#39704 = ORIENTED_EDGE ( 'NONE', *, *, #43987, .T. ) ;
#39705 = DIRECTION ( 'NONE',  ( -1.000000000000000000, 0.000000000000000000, 0.000000000000000000 ) ) ;
#39706 = PLANE ( 'NONE',  #48557 ) ;
#39707 = CARTESIAN_POINT ( 'NONE',  ( 164.9999999999999716, 17.00000000000000000, -85.00000000000001421 ) ) ;
#39708 = VERTEX_POINT ( 'NONE', #39771 ) ;
#39709 = DIRECTION ( 'NONE',  ( -1.000000000000000000, 0.000000000000000000, 0.000000000000000000 ) ) ;
#39710 = ORIENTED_EDGE ( 'NONE', *, *, #40387, .F. ) ;
#39711 = ORIENTED_EDGE ( 'NONE', *, *, #3045, .F. ) ;
#39712 = FACE_OUTER_BOUND ( 'NONE', #5348, .T. ) ;
#39713 = CARTESIAN_POINT ( 'NONE',  ( 30.00000000000153833, 17.00000000000000000, 35.00000000000000000 ) ) ;
#39714 = EDGE_LOOP ( 'NONE', ( #9229, #28145, #30555, #3324, #44759, #14983 ) ) ;
#39715 = CARTESIAN_POINT ( 'NONE',  ( 2.188678504086826848, -0.3267089737525829540, 9.881002359080282460 ) ) ;
#39716 = CARTESIAN_POINT ( 'NONE',  ( -41.18776771165107675, 7.147140551973688360, 8.846626183609803462 ) ) ;
#39717 = VECTOR ( 'NONE', #35497, 1000.000000000000000 ) ;
#39718 = ORIENTED_EDGE ( 'NONE', *, *, #31800, .F. ) ;
#39719 = AXIS2_PLACEMENT_3D ( 'NONE', #10466, #26106, #37941 ) ;
#39720 = ADVANCED_FACE ( 'NONE', ( #4615 ), #16401, .T. ) ;
#39721 = CYLINDRICAL_SURFACE ( 'NONE', #11221, 1.750000000000015543 ) ;
#39722 = ORIENTED_EDGE ( 'NONE', *, *, #19614, .T. ) ;
#39723 = VECTOR ( 'NONE', #23507, 1000.000000000000000 ) ;
#39724 = PLANE ( 'NONE',  #47086 ) ;
#39725 = LINE ( 'NONE', #4559, #29986 ) ;
#39726 = CARTESIAN_POINT ( 'NONE',  ( 169.0000000000000000, -9.999999999999953815, -111.0000000000001563 ) ) ;
#39727 = VERTEX_POINT ( 'NONE', #36949 ) ;
#39728 = CARTESIAN_POINT ( 'NONE',  ( 34.38425513258721367, -36.82177522737821107, 8.807470649214879543 ) ) ;
#39729 = DIRECTION ( 'NONE',  ( 0.000000000000000000, -1.000000000000000000, 0.000000000000000000 ) ) ;
#39730 = EDGE_LOOP ( 'NONE', ( #22217, #34013, #6513, #13865 ) ) ;
#39731 = EDGE_CURVE ( 'NONE', #43884, #14506, #49168, .T. ) ;
#39732 = EDGE_LOOP ( 'NONE', ( #25927, #33490, #10366, #23551 ) ) ;
#39733 = ORIENTED_EDGE ( 'NONE', *, *, #8467, .F. ) ;
#39734 = CARTESIAN_POINT ( 'NONE',  ( 168.9999999999999716, 6.000000000000060396, 339.9999999999998295 ) ) ;
#39735 = ORIENTED_EDGE ( 'NONE', *, *, #31867, .T. ) ;
#39736 = CARTESIAN_POINT ( 'NONE',  ( -86.69597344681494633, -1.750000000000010658, -119.1817124430720440 ) ) ;
#39737 = CARTESIAN_POINT ( 'NONE',  ( -19.99999999999846523, 17.00000000000000000, 35.00000000000000000 ) ) ;
#39738 = DIRECTION ( 'NONE',  ( -0.000000000000000000, -1.000000000000000000, -0.000000000000000000 ) ) ;
#39739 = EDGE_CURVE ( 'NONE', #34855, #8918, #22866, .T. ) ;
#39740 = AXIS2_PLACEMENT_3D ( 'NONE', #29828, #10072, #41375 ) ;
#39741 = CARTESIAN_POINT ( 'NONE',  ( -44.94597344681493922, 1.025126265847089657, 42.56828755692799149 ) ) ;
#39742 = CARTESIAN_POINT ( 'NONE',  ( 168.9999999999999716, -174.9999999999999716, -342.0000000000001137 ) ) ;
#39743 = EDGE_CURVE ( 'NONE', #24017, #28153, #2516, .T. ) ;
#39744 = VECTOR ( 'NONE', #38312, 1000.000000000000000 ) ;
#39745 = PLANE ( 'NONE',  #42296 ) ;
#39746 = CARTESIAN_POINT ( 'NONE',  ( 191.5540265531850537, 1.025126265847089213, -37.43171244307202272 ) ) ;
#39747 = ADVANCED_FACE ( 'NONE', ( #9707 ), #6363, .F. ) ;
#39748 = FACE_OUTER_BOUND ( 'NONE', #41479, .T. ) ;
#39749 = FACE_OUTER_BOUND ( 'NONE', #22039, .T. ) ;
#39750 = EDGE_CURVE ( 'NONE', #22924, #44274, #25621, .T. ) ;
#39751 = EDGE_CURVE ( 'NONE', #41862, #17026, #21766, .T. ) ;
#39752 = LINE ( 'NONE', #35906, #10737 ) ;
#39753 = SPHERICAL_SURFACE ( 'NONE', #7703, 0.5000000000000000000 ) ;
#39754 = CARTESIAN_POINT ( 'NONE',  ( 9.999999999999998224, 1.843143693225357538E-15, 8.340239149798797769 ) ) ;
#39755 = VERTEX_POINT ( 'NONE', #2020 ) ;
#39756 = LINE ( 'NONE', #20241, #17160 ) ;
#39757 = ADVANCED_FACE ( 'NONE', ( #2260 ), #18157, .T. ) ;
#39758 = CARTESIAN_POINT ( 'NONE',  ( 0.000000000000000000, -50.00000000000000000, 0.000000000000000000 ) ) ;
#39759 = CARTESIAN_POINT ( 'NONE',  ( -168.4459734468149463, 0.000000000000000000, 2.568287556927978166 ) ) ;
#39760 = VECTOR ( 'NONE', #8177, 1000.000000000000000 ) ;
#39761 = CARTESIAN_POINT ( 'NONE',  ( 0.3862712429686810944, 1.188820645368943607, 10.00000000000000000 ) ) ;
#39762 = ORIENTED_EDGE ( 'NONE', *, *, #7417, .T. ) ;
#39763 =( NAMED_UNIT ( * ) PLANE_ANGLE_UNIT ( ) SI_UNIT ( $, .RADIAN. ) );
#39764 = DIRECTION ( 'NONE',  ( -0.000000000000000000, -0.000000000000000000, -1.000000000000000000 ) ) ;
#39765 =( BOUNDED_CURVE ( )  B_SPLINE_CURVE ( 3, ( #4944, #31919, #27805, #1114 ),
 .UNSPECIFIED., .F., .F. ) 
 B_SPLINE_CURVE_WITH_KNOTS ( ( 4, 4 ),
 ( 0.000000000000000000, 1.570796326794896780 ),
 .UNSPECIFIED. ) 
 CURVE ( )  GEOMETRIC_REPRESENTATION_ITEM ( )  RATIONAL_B_SPLINE_CURVE ( ( 1.000000000000000000, 0.8047378541243649375, 0.8047378541243649375, 1.000000000000000000 ) ) 
 REPRESENTATION_ITEM ( '' )  );
#39766 = ORIENTED_EDGE ( 'NONE', *, *, #24322, .T. ) ;
#39767 = CARTESIAN_POINT ( 'NONE',  ( 16.69947034530964913, -2.312583065866261389, 2.590526750877053086 ) ) ;
#39768 = DIRECTION ( 'NONE',  ( 0.000000000000000000, 0.000000000000000000, 1.000000000000000000 ) ) ;
#39769 = LINE ( 'NONE', #16399, #7164 ) ;
#39770 = VERTEX_POINT ( 'NONE', #32830 ) ;
#39771 = CARTESIAN_POINT ( 'NONE',  ( 71.55402655318505367, 0.000000000000000000, -120.9317124430720725 ) ) ;
#39772 = ORIENTED_EDGE ( 'NONE', *, *, #25580, .F. ) ;
#39773 = VERTEX_POINT ( 'NONE', #6113 ) ;
#39774 = CARTESIAN_POINT ( 'NONE',  ( 113.3040265531850537, 0.000000000000000000, 165.0000000000000000 ) ) ;
#39775 = LINE ( 'NONE', #43853, #48588 ) ;
#39776 = APPLICATION_CONTEXT ( 'automotive_design' ) ;
#39777 = ORIENTED_EDGE ( 'NONE', *, *, #20330, .F. ) ;
#39778 = CARTESIAN_POINT ( 'NONE',  ( 210.0000000000000568, 0.000000000000000000, 0.8182875569279768335 ) ) ;
#39779 = CARTESIAN_POINT ( 'NONE',  ( 0.000000000000000000, -168.9999999999999432, -356.0000000000002274 ) ) ;
#39780 = DIRECTION ( 'NONE',  ( -1.000000000000000000, -0.000000000000000000, -0.000000000000000000 ) ) ;
#39781 = VECTOR ( 'NONE', #10822, 1000.000000000000000 ) ;
#39782 = DIRECTION ( 'NONE',  ( 0.000000000000000000, 0.000000000000000000, 1.000000000000000000 ) ) ;
#39783 = ORIENTED_EDGE ( 'NONE', *, *, #36282, .F. ) ;
#39784 = ADVANCED_FACE ( 'NONE', ( #17411 ), #14053, .T. ) ;
#39785 = CARTESIAN_POINT ( 'NONE',  ( 210.0000000000000568, 2.143131898507880377E-16, -160.9317124430720298 ) ) ;
#39786 = MECHANICAL_DESIGN_GEOMETRIC_PRESENTATION_REPRESENTATION (  '', ( #11089 ), #8648 ) ;
#39787 = ORIENTED_EDGE ( 'NONE', *, *, #44291, .F. ) ;
#39788 = DIRECTION ( 'NONE',  ( 0.000000000000000000, 0.000000000000000000, 1.000000000000000000 ) ) ;
#39789 = VECTOR ( 'NONE', #41935, 1000.000000000000000 ) ;
#39790 = CARTESIAN_POINT ( 'NONE',  ( 154.3291528190321458, -1.750000000000009548, 39.79316129108089228 ) ) ;
#39791 = AXIS2_PLACEMENT_3D ( 'NONE', #36972, #30765, #22036 ) ;
#39792 = ORIENTED_EDGE ( 'NONE', *, *, #16180, .T. ) ;
#39793 = DIRECTION ( 'NONE',  ( -1.000000000000000000, 0.000000000000000000, 0.000000000000000000 ) ) ;
#39794 = PLANE ( 'NONE',  #31698 ) ;
#39795 = ORIENTED_EDGE ( 'NONE', *, *, #47742, .F. ) ;
#39796 = CIRCLE ( 'NONE', #20918, 4.000000000000003553 ) ;
#39797 = LINE ( 'NONE', #291, #50443 ) ;
#39798 = CARTESIAN_POINT ( 'NONE',  ( 35.05402655318504657, 2.143131898507880377E-16, 2.568287556927978166 ) ) ;
#39799 = DIRECTION ( 'NONE',  ( -2.958228394578793832E-31, 0.000000000000000000, -1.000000000000000000 ) ) ;
#39800 = CARTESIAN_POINT ( 'NONE',  ( 0.3656201545664388708, -2.182515578491310393, 9.881002359080277131 ) ) ;
#39801 = EDGE_CURVE ( 'NONE', #35891, #31251, #9964, .T. ) ;
#39802 = EDGE_CURVE ( 'NONE', #22583, #48305, #50136, .T. ) ;
#39803 = EDGE_LOOP ( 'NONE', ( #37623, #19804, #21895, #36372, #13359, #42089 ) ) ;
#39804 = LINE ( 'NONE', #4876, #16080 ) ;
#39805 = EDGE_CURVE ( 'NONE', #20580, #1904, #43845, .T. ) ;
#39806 = PLANE ( 'NONE',  #25647 ) ;
#39807 = ORIENTED_EDGE ( 'NONE', *, *, #50014, .T. ) ;
#39808 = ORIENTED_EDGE ( 'NONE', *, *, #9182, .F. ) ;
#39809 = EDGE_CURVE ( 'NONE', #11132, #15809, #21014, .T. ) ;
#39810 = PRODUCT_CONTEXT ( 'NONE', #29271, 'mechanical' ) ;
#39811 = EDGE_CURVE ( 'NONE', #43082, #16057, #49045, .T. ) ;
#39812 = DIRECTION ( 'NONE',  ( -1.000000000000000000, 0.000000000000000000, -0.000000000000000000 ) ) ;
#39813 = CARTESIAN_POINT ( 'NONE',  ( -15.00199999999999712, -34.54492135858216528, 5.000000000000000000 ) ) ;
#39814 = AXIS2_PLACEMENT_3D ( 'NONE', #43409, #1085, #32384 ) ;
#39815 = CARTESIAN_POINT ( 'NONE',  ( -26.18032376592659105, 21.95228666728381128, 7.455576670931136185 ) ) ;
#39816 = MANIFOLD_SOLID_BREP ( 'Square tube 20 X 20 X 2(1)[3]', #15476 ) ;
#39818 = VECTOR ( 'NONE', #15478, 1000.000000000000000 ) ;
#39817 = PLANE ( 'NONE',  #33891 ) ;
#39819 = CARTESIAN_POINT ( 'NONE',  ( 169.0000000000000000, -174.9999999999999716, -99.00000000000014211 ) ) ;
#39820 = EDGE_LOOP ( 'NONE', ( #46656, #14721, #8381, #45398 ) ) ;
#39821 = EDGE_CURVE ( 'NONE', #37052, #42864, #15079, .T. ) ;
#39822 = DIRECTION ( 'NONE',  ( 2.312964634635864737E-16, -0.000000000000000000, 1.000000000000000000 ) ) ;
#39823 = CARTESIAN_POINT ( 'NONE',  ( -6.695973446814940111, 0.000000000000000000, 165.0000000000000000 ) ) ;
#39824 = LINE ( 'NONE', #15442, #24175 ) ;
#39825 = LINE ( 'NONE', #8258, #37926 ) ;
#39826 = ADVANCED_FACE ( 'NONE', ( #33330 ), #18769, .T. ) ;
#39827 =( BOUNDED_CURVE ( )  B_SPLINE_CURVE ( 3, ( #32707, #1165, #32467, #39656 ),
 .UNSPECIFIED., .F., .F. ) 
 B_SPLINE_CURVE_WITH_KNOTS ( ( 4, 4 ),
 ( 0.000000000000000000, 1.570796326794896558 ),
 .UNSPECIFIED. ) 
 CURVE ( )  GEOMETRIC_REPRESENTATION_ITEM ( )  RATIONAL_B_SPLINE_CURVE ( ( 1.000000000000000000, 0.8047378541243649375, 0.8047378541243649375, 1.000000000000000000 ) ) 
 REPRESENTATION_ITEM ( '' )  );
#39828 = AXIS2_PLACEMENT_3D ( 'NONE', #43888, #27992, #24162 ) ;
#39829 = ORIENTED_EDGE ( 'NONE', *, *, #45852, .F. ) ;
#39830 = LINE ( 'NONE', #23654, #42807 ) ;
#39831 = ORIENTED_EDGE ( 'NONE', *, *, #15792, .F. ) ;
#39832 = CARTESIAN_POINT ( 'NONE',  ( 12.35406723005396046, -11.51001571518080624, 9.178419661560148768 ) ) ;
#39833 = AXIS2_PLACEMENT_3D ( 'NONE', #9796, #45173, #10061 ) ;
#39834 = ORIENTED_EDGE ( 'NONE', *, *, #21458, .F. ) ;
#39835 = CARTESIAN_POINT ( 'NONE',  ( -23.26005729352344176, -44.90397804740339183, 7.906207997025717304 ) ) ;
#39836 = CARTESIAN_POINT ( 'NONE',  ( 339.9999999999999432, -168.9999999999999432, -358.0000000000002274 ) ) ;
#39837 =( BOUNDED_CURVE ( )  B_SPLINE_CURVE ( 3, ( #42497, #30720, #35094, #184 ),
 .UNSPECIFIED., .F., .F. ) 
 B_SPLINE_CURVE_WITH_KNOTS ( ( 4, 4 ),
 ( 1.570796326794896558, 3.141592653589793116 ),
 .UNSPECIFIED. ) 
 CURVE ( )  GEOMETRIC_REPRESENTATION_ITEM ( )  RATIONAL_B_SPLINE_CURVE ( ( 1.000000000000000000, 0.8047378541243649375, 0.8047378541243649375, 1.000000000000000000 ) ) 
 REPRESENTATION_ITEM ( '' )  );
#39838 = CARTESIAN_POINT ( 'NONE',  ( -205.6708471809678827, -1.750000000000009548, -38.15658617722494483 ) ) ;
#39839 = CARTESIAN_POINT ( 'NONE',  ( -124.9459734468149321, -1.025126265847081664, -77.43171244307201562 ) ) ;
#39840 = AXIS2_PLACEMENT_3D ( 'NONE', #40437, #44007, #48077 ) ;
#39841 = VERTEX_POINT ( 'NONE', #22271 ) ;
#39842 = CIRCLE ( 'NONE', #47136, 22.00000000000000000 ) ;
#39843 = DIRECTION ( 'NONE',  ( -1.000000000000000000, 0.000000000000000000, 0.000000000000000000 ) ) ;
#39844 = DIRECTION ( 'NONE',  ( 0.000000000000000000, 0.2981428420003837121, 0.9545212652235329776 ) ) ;
#39845 = ORIENTED_EDGE ( 'NONE', *, *, #17586, .F. ) ;
#39846 = CARTESIAN_POINT ( 'NONE',  ( 5.873104089934109595, 0.6060605173725697181, 9.586754400234156037 ) ) ;
#39847 = CARTESIAN_POINT ( 'NONE',  ( 0.5000000000000000000, 0.5000000000000000000, 1000.000000000000000 ) ) ;
#39848 = DIRECTION ( 'NONE',  ( 0.7233555441435720601, -0.6904757466825006684, 0.000000000000000000 ) ) ;
#39849 = CARTESIAN_POINT ( 'NONE',  ( 33.30402655318503946, 1.750000000000010658, -119.1817124430720440 ) ) ;
#39850 = EDGE_CURVE ( 'NONE', #4897, #27926, #18411, .T. ) ;
#39851 = ORIENTED_EDGE ( 'NONE', *, *, #28374, .T. ) ;
#39852 = ORIENTED_EDGE ( 'NONE', *, *, #10493, .F. ) ;
#39853 = FACE_OUTER_BOUND ( 'NONE', #4344, .T. ) ;
#39854 = EDGE_CURVE ( 'NONE', #40520, #27700, #3521, .T. ) ;
#39855 = AXIS2_PLACEMENT_3D ( 'NONE', #9467, #41028, #2710 ) ;
#39856 = VERTEX_POINT ( 'NONE', #19164 ) ;
#39857 = VECTOR ( 'NONE', #10794, 1000.000000000000000 ) ;
#39858 = CARTESIAN_POINT ( 'NONE',  ( 0.000000000000000000, -180.9999999999999716, -342.0000000000001705 ) ) ;
#39859 = CARTESIAN_POINT ( 'NONE',  ( -86.69597344681494633, -1.750000000000010214, 40.81828755692798438 ) ) ;
#39860 = CARTESIAN_POINT ( 'NONE',  ( -166.6959734468149463, 0.000000000000000000, 165.0000000000000000 ) ) ;
#39861 = ORIENTED_EDGE ( 'NONE', *, *, #1512, .T. ) ;
#39862 = CARTESIAN_POINT ( 'NONE',  ( -18.67411147745623978, -27.51799019669813973, -3.760136334089591248 ) ) ;
#39863 = DIRECTION ( 'NONE',  ( -0.8637789008984334549, 0.000000000000000000, 0.5038710255240862468 ) ) ;
#39865 = CIRCLE ( 'NONE', #19365, 4.999999999999997335 ) ;
#39864 = CARTESIAN_POINT ( 'NONE',  ( 10.00000000000000000, 1.224646799147353256E-15, 10.00000000000000000 ) ) ;
#39866 = ORIENTED_EDGE ( 'NONE', *, *, #46155, .T. ) ;
#39867 = ORIENTED_EDGE ( 'NONE', *, *, #19863, .T. ) ;
#39868 = VECTOR ( 'NONE', #28444, 1000.000000000000000 ) ;
#39869 = ORIENTED_EDGE ( 'NONE', *, *, #3918, .F. ) ;
#39870 = CARTESIAN_POINT ( 'NONE',  ( 4.641001526964561918, 45.74479092860853058, -8.016098858316205167 ) ) ;
#39871 = DIRECTION ( 'NONE',  ( 0.000000000000000000, 2.537652627714643577E-15, 1.000000000000000000 ) ) ;
#39872 = CARTESIAN_POINT ( 'NONE',  ( -8.445973446814964092, -1.025126265847097651, 82.56828755692798438 ) ) ;
#39873 = EDGE_LOOP ( 'NONE', ( #36122, #39905, #32648, #8171 ) ) ;
#39874 = CARTESIAN_POINT ( 'NONE',  ( -46.69597344681494633, 0.000000000000000000, 165.0000000000000000 ) ) ;
#39875 = VERTEX_POINT ( 'NONE', #45827 ) ;
#39876 = AXIS2_PLACEMENT_3D ( 'NONE', #1593, #25188, #40833 ) ;
#39877 = DIRECTION ( 'NONE',  ( 0.000000000000000000, 2.969158215481698263E-48, -1.000000000000000000 ) ) ;
#39878 = VERTEX_POINT ( 'NONE', #49424 ) ;
#39879 = CARTESIAN_POINT ( 'NONE',  ( -32.70595913738893756, -11.36290827441765927, -1.383675951444729435 ) ) ;
#39880 = DIRECTION ( 'NONE',  ( 1.000000000000000000, 0.000000000000000000, 0.000000000000000000 ) ) ;
#39881 = CARTESIAN_POINT ( 'NONE',  ( -87.72109971266203843, -1.750000000000009548, -160.2068387089191219 ) ) ;
#39882 = DIRECTION ( 'NONE',  ( 1.000000000000000000, 0.000000000000000000, 0.000000000000000000 ) ) ;
#39883 = PLANE ( 'NONE',  #32421 ) ;
#39884 = DIRECTION ( 'NONE',  ( -0.000000000000000000, -1.000000000000000000, -0.000000000000000000 ) ) ;
#39885 = DIRECTION ( 'NONE',  ( -1.000000000000000000, 0.000000000000000000, 0.000000000000000000 ) ) ;
#39886 = ORIENTED_EDGE ( 'NONE', *, *, #8906, .F. ) ;
#39887 = ORIENTED_EDGE ( 'NONE', *, *, #34626, .T. ) ;
#39888 = ADVANCED_FACE ( 'NONE', ( #23270 ), #38202, .T. ) ;
#39889 = PLANE ( 'NONE',  #37868 ) ;
#39890 = CARTESIAN_POINT ( 'NONE',  ( -9.760995290733800900, 2.173239732351794462, 9.646707543097347681 ) ) ;
#39891 = CARTESIAN_POINT ( 'NONE',  ( 31.55402655318503236, -1.025126265847089435, -40.93171244307204404 ) ) ;
#39892 = CARTESIAN_POINT ( 'NONE',  ( 185.0000000000000000, 175.0000000000000284, -356.0000000000001705 ) ) ;
#39893 = VECTOR ( 'NONE', #1787, 1000.000000000000000 ) ;
#39894 =( GEOMETRIC_REPRESENTATION_CONTEXT ( 3 ) GLOBAL_UNCERTAINTY_ASSIGNED_CONTEXT ( ( #24594 ) ) GLOBAL_UNIT_ASSIGNED_CONTEXT ( ( #8368, #4508, #32481 ) ) REPRESENTATION_CONTEXT ( 'NONE', 'WORKASPACE' ) );
#39895 = FACE_OUTER_BOUND ( 'NONE', #10452, .T. ) ;
#39896 = ORIENTED_EDGE ( 'NONE', *, *, #16285, .T. ) ;
#39897 = CARTESIAN_POINT ( 'NONE',  ( 75.05402655318509630, 2.143131898507880377E-16, -0.9317124430720524764 ) ) ;
#39898 = DIRECTION ( 'NONE',  ( 0.000000000000000000, 1.000000000000000000, 0.000000000000000000 ) ) ;
#39899 = ORIENTED_EDGE ( 'NONE', *, *, #17666, .T. ) ;
#39900 = FACE_OUTER_BOUND ( 'NONE', #29721, .T. ) ;
#39901 = CARTESIAN_POINT ( 'NONE',  ( 73.30402655318508209, 1.750000000000010214, 40.81828755692798438 ) ) ;
#39902 = CARTESIAN_POINT ( 'NONE',  ( 357.1715728752541850, 167.0000000000003411, -342.0000000000004547 ) ) ;
#39903 = LINE ( 'NONE', #12182, #34869 ) ;
#39904 = ORIENTED_EDGE ( 'NONE', *, *, #22462, .T. ) ;
#39905 = ORIENTED_EDGE ( 'NONE', *, *, #3691, .F. ) ;
#39906 = CARTESIAN_POINT ( 'NONE',  ( -167.4999999999999432, 102.5000000000000142, -8.474599139414886295 ) ) ;
#39907 = VECTOR ( 'NONE', #7020, 1000.000000000000000 ) ;
#39908 = CARTESIAN_POINT ( 'NONE',  ( 22.69295089195473736, 45.31600496604706052, 7.455576670931136185 ) ) ;
#39909 = EDGE_CURVE ( 'NONE', #25838, #26976, #44541, .T. ) ;
#39910 = ORIENTED_EDGE ( 'NONE', *, *, #38526, .F. ) ;
#39911 = ORIENTED_EDGE ( 'NONE', *, *, #16714, .F. ) ;
#39912 = CARTESIAN_POINT ( 'NONE',  ( 30.00000000000029132, 16.00000000000000000, -84.99999999999998579 ) ) ;
#39913 = CARTESIAN_POINT ( 'NONE',  ( 8.277096487746778308, -50.00000000000000000, 7.455576670931136185 ) ) ;
#39914 = CARTESIAN_POINT ( 'NONE',  ( 29.18392875402930997, 17.44843138996603216, 7.906207997025717304 ) ) ;
#39915 = SHAPE_REPRESENTATION ( 'fan', ( #45486 ), #38147 ) ;
#39916 = DIRECTION ( 'NONE',  ( 0.000000000000000000, 0.000000000000000000, -1.000000000000000000 ) ) ;
#39917 = ORIENTED_EDGE ( 'NONE', *, *, #50528, .T. ) ;
#39918 = ORIENTED_EDGE ( 'NONE', *, *, #38539, .T. ) ;
#39919 = VERTEX_POINT ( 'NONE', #34854 ) ;
#39920 = CARTESIAN_POINT ( 'NONE',  ( 72.27890028733797578, -1.750000000000009548, 41.84341382277508359 ) ) ;
#39921 = VECTOR ( 'NONE', #1014, 1000.000000000000000 ) ;
#39922 = LINE ( 'NONE', #38912, #11527 ) ;
#39923 = ORIENTED_EDGE ( 'NONE', *, *, #10813, .T. ) ;
#39924 = ORIENTED_EDGE ( 'NONE', *, *, #21834, .F. ) ;
#39925 = CARTESIAN_POINT ( 'NONE',  ( -8.445973446814914354, 2.143131898507880377E-16, -160.9317124430720298 ) ) ;
#39926 = CARTESIAN_POINT ( 'NONE',  ( 210.0000000000000568, 0.000000000000000000, -159.1817124430720298 ) ) ;
#39927 = CARTESIAN_POINT ( 'NONE',  ( 6.174150299305392053, -50.00000000000000000, 8.807470649214879543 ) ) ;
#39928 = EDGE_LOOP ( 'NONE', ( #48866, #1464, #2789, #50169, #16675, #547 ) ) ;
#39929 = ORIENTED_EDGE ( 'NONE', *, *, #23673, .F. ) ;
#39930 = CARTESIAN_POINT ( 'NONE',  ( -0.3862712429686729343, -1.188820645368946050, 10.00000000000000000 ) ) ;
#39931 = CARTESIAN_POINT ( 'NONE',  ( -70.00000000000002842, 17.00000000000000000, -114.9999999999999858 ) ) ;
#39932 = ORIENTED_EDGE ( 'NONE', *, *, #21751, .T. ) ;
#39933 = PLANE ( 'NONE',  #28919 ) ;
#39934 = CARTESIAN_POINT ( 'NONE',  ( -2.322372356066614074, -2.286285436021753270, 9.799352050262461589 ) ) ;
#39935 = DIRECTION ( 'NONE',  ( -1.000000000000000000, 0.000000000000000000, -0.000000000000000000 ) ) ;
#39936 = DIRECTION ( 'NONE',  ( -0.000000000000000000, -0.000000000000000000, -1.000000000000000000 ) ) ;
#39937 = ORIENTED_EDGE ( 'NONE', *, *, #49636, .F. ) ;
#39938 = EDGE_CURVE ( 'NONE', #9083, #34191, #38443, .T. ) ;
#39939 = CARTESIAN_POINT ( 'NONE',  ( -46.76852358249002606, 17.86468378716741512, -9.367992836599954742 ) ) ;
#39940 = CARTESIAN_POINT ( 'NONE',  ( -0.1530804384065780344, 1.323112372394628977, 9.951893257059998277 ) ) ;
#39941 = CARTESIAN_POINT ( 'NONE',  ( -167.4999999999999432, 102.5000000000000142, -10.00000000000000000 ) ) ;
#39942 = EDGE_CURVE ( 'NONE', #6443, #16093, #47797, .T. ) ;
#39943 = FACE_OUTER_BOUND ( 'NONE', #37570, .T. ) ;
#39944 = EDGE_CURVE ( 'NONE', #10841, #21654, #10470, .T. ) ;
#39945 = DIRECTION ( 'NONE',  ( -1.586032892321652236E-16, -1.000000000000000000, -2.288264760618012091E-48 ) ) ;
#39946 = EDGE_CURVE ( 'NONE', #43746, #7277, #45590, .T. ) ;
#39947 = EDGE_CURVE ( 'NONE', #10849, #18366, #14017, .T. ) ;
#39948 = DIRECTION ( 'NONE',  ( -0.000000000000000000, -1.000000000000000000, -0.000000000000000000 ) ) ;
#39949 = DIRECTION ( 'NONE',  ( 1.000000000000000000, 0.000000000000000000, 0.000000000000000000 ) ) ;
#39950 = EDGE_CURVE ( 'NONE', #6697, #43021, #11025, .T. ) ;
#39951 = ORIENTED_EDGE ( 'NONE', *, *, #48069, .F. ) ;
#39952 = VECTOR ( 'NONE', #8463, 1000.000000000000000 ) ;
#39953 = FACE_OUTER_BOUND ( 'NONE', #24544, .T. ) ;
#39954 = ORIENTED_EDGE ( 'NONE', *, *, #49304, .F. ) ;
#39955 = FACE_OUTER_BOUND ( 'NONE', #4142, .T. ) ;
#39956 = CARTESIAN_POINT ( 'NONE',  ( 26.18032376592674737, -21.95228666728361233, 7.455576670931136185 ) ) ;
#39957 = CARTESIAN_POINT ( 'NONE',  ( 350.0000000000000000, 167.0000000000000000, -344.0000000000001705 ) ) ;
#39958 = ORIENTED_EDGE ( 'NONE', *, *, #34788, .F. ) ;
#39959 = CARTESIAN_POINT ( 'NONE',  ( -164.9459734468149463, -1.025126265847089435, -117.4317124430720156 ) ) ;
#39960 = EDGE_CURVE ( 'NONE', #28669, #37345, #4544, .T. ) ;
#39962 = ORIENTED_EDGE ( 'NONE', *, *, #39634, .T. ) ;
#39961 = EDGE_CURVE ( 'NONE', #31607, #12842, #19265, .T. ) ;
#39963 = ORIENTED_EDGE ( 'NONE', *, *, #3700, .F. ) ;
#39964 = CARTESIAN_POINT ( 'NONE',  ( 0.3862712429686978033, -1.188820645368937834, -10.00000000000000000 ) ) ;
#39965 = CARTESIAN_POINT ( 'NONE',  ( 1.962712821592840662, 1.022159834731142691, 9.881002359080275355 ) ) ;
#39966 =( BOUNDED_CURVE ( )  B_SPLINE_CURVE ( 3, ( #32649, #41096, #5940, #21588 ),
 .UNSPECIFIED., .F., .F. ) 
 B_SPLINE_CURVE_WITH_KNOTS ( ( 4, 4 ),
 ( 0.2242347511090889423, 1.570796326794895670 ),
 .UNSPECIFIED. ) 
 CURVE ( )  GEOMETRIC_REPRESENTATION_ITEM ( )  RATIONAL_B_SPLINE_CURVE ( ( 1.000000000000000000, 0.8545200852688790150, 0.8545200852688790150, 1.000000000000000000 ) ) 
 REPRESENTATION_ITEM ( '' )  );
#39967 = ADVANCED_FACE ( 'NONE', ( #35110 ), #50685, .T. ) ;
#39968 = EDGE_CURVE ( 'NONE', #13126, #9081, #29767, .T. ) ;
#39969 = ORIENTED_EDGE ( 'NONE', *, *, #42623, .F. ) ;
#39970 = LINE ( 'NONE', #48610, #18017 ) ;
#39971 = ORIENTED_EDGE ( 'NONE', *, *, #45272, .F. ) ;
#39972 = ADVANCED_FACE ( 'NONE', ( #28406 ), #47602, .T. ) ;
#39973 =( BOUNDED_CURVE ( )  B_SPLINE_CURVE ( 3, ( #37801, #48783, #6472, #14159 ),
 .UNSPECIFIED., .F., .F. ) 
 B_SPLINE_CURVE_WITH_KNOTS ( ( 4, 4 ),
 ( 0.000000000000000000, 1.570796326794896558 ),
 .UNSPECIFIED. ) 
 CURVE ( )  GEOMETRIC_REPRESENTATION_ITEM ( )  RATIONAL_B_SPLINE_CURVE ( ( 1.000000000000000000, 0.8047378541243649375, 0.8047378541243649375, 1.000000000000000000 ) ) 
 REPRESENTATION_ITEM ( '' )  );
#39974 = EDGE_CURVE ( 'NONE', #50130, #24506, #35046, .T. ) ;
#39975 = CARTESIAN_POINT ( 'NONE',  ( 0.3896797354184660667, -1.262193838292004155, 9.943883492372872723 ) ) ;
#39976 = ORIENTED_EDGE ( 'NONE', *, *, #1093, .F. ) ;
#39977 = CARTESIAN_POINT ( 'NONE',  ( 80.00000000000061107, 17.00000000000000000, -30.00000000000000000 ) ) ;
#39978 = CARTESIAN_POINT ( 'NONE',  ( -8.445973446814976526, 0.000000000000000000, -157.4317124430720014 ) ) ;
#39979 = CARTESIAN_POINT ( 'NONE',  ( 1.011271242968688311, -0.7347315653655855927, -10.00000000000000000 ) ) ;
#39980 = VERTEX_POINT ( 'NONE', #35866 ) ;
#39981 = CARTESIAN_POINT ( 'NONE',  ( 210.0000000000000568, 0.000000000000000000, 40.81828755692798438 ) ) ;
#39982 = LINE ( 'NONE', #35132, #26121 ) ;
#39983 = ORIENTED_EDGE ( 'NONE', *, *, #8649, .F. ) ;
#39984 = EDGE_LOOP ( 'NONE', ( #14392, #14884, #6801, #27264 ) ) ;
#39985 = VERTEX_POINT ( 'NONE', #20190 ) ;
#39986 = CARTESIAN_POINT ( 'NONE',  ( -0.3896797354171960270, 1.262193838292709147, 9.943883492372847854 ) ) ;
#39987 =( BOUNDED_CURVE ( )  B_SPLINE_CURVE ( 3, ( #47954, #36473, #1313, #16960 ),
 .UNSPECIFIED., .F., .F. ) 
 B_SPLINE_CURVE_WITH_KNOTS ( ( 4, 4 ),
 ( 3.141592653589793116, 4.712388980384689674 ),
 .UNSPECIFIED. ) 
 CURVE ( )  GEOMETRIC_REPRESENTATION_ITEM ( )  RATIONAL_B_SPLINE_CURVE ( ( 1.000000000000000000, 0.8047378541243649375, 0.8047378541243649375, 1.000000000000000000 ) ) 
 REPRESENTATION_ITEM ( '' )  );
#39988 = CARTESIAN_POINT ( 'NONE',  ( 349.9999999999999432, -168.9999999999999432, 343.9999999999997726 ) ) ;
#39989 = ORIENTED_EDGE ( 'NONE', *, *, #34064, .T. ) ;
#39990 = EDGE_CURVE ( 'NONE', #6697, #11814, #47693, .T. ) ;
#39991 = LINE ( 'NONE', #12514, #47064 ) ;
#39992 = CARTESIAN_POINT ( 'NONE',  ( 0.000000000000000000, 165.2000000000000171, 359.7999999999997840 ) ) ;
#39993 = DIRECTION ( 'NONE',  ( -0.000000000000000000, -0.000000000000000000, -1.000000000000000000 ) ) ;
#39994 = EDGE_CURVE ( 'NONE', #29467, #41788, #20431, .T. ) ;
#39995 = CARTESIAN_POINT ( 'NONE',  ( 35.05402655318504657, 2.143131898507880377E-16, -160.9317124430720582 ) ) ;
#39996 = VECTOR ( 'NONE', #18876, 1000.000000000000000 ) ;
#39997 = ADVANCED_FACE ( 'NONE', ( #958 ), #35369, .F. ) ;
#39998 = CARTESIAN_POINT ( 'NONE',  ( -85.67084718096784002, -1.750000000000009548, 39.79316129108089228 ) ) ;
#39999 = CARTESIAN_POINT ( 'NONE',  ( -556.8973046169135159, 53.53801056904005407, -64.63743994998280584 ) ) ;
#40000 = EDGE_CURVE ( 'NONE', #44684, #46959, #40261, .T. ) ;
#40001 = DIRECTION ( 'NONE',  ( 0.000000000000000000, 0.000000000000000000, 1.000000000000000000 ) ) ;
#40002 = DIRECTION ( 'NONE',  ( 0.000000000000000000, -0.000000000000000000, -1.000000000000000000 ) ) ;
#40003 = ADVANCED_FACE ( 'NONE', ( #12483 ), #8149, .T. ) ;
#40004 = DIRECTION ( 'NONE',  ( -4.758098676964957447E-16, -1.000000000000000000, 7.143884938411937192E-48 ) ) ;
#40005 = UNCERTAINTY_MEASURE_WITH_UNIT (LENGTH_MEASURE( 1.000000000000000082E-05 ), #7757, 'distance_accuracy_value', 'NONE');
#40006 = CARTESIAN_POINT ( 'NONE',  ( 0.000000000000000000, 17.00000000000000000, 0.000000000000000000 ) ) ;
#40007 = VERTEX_POINT ( 'NONE', #16342 ) ;
#40008 = LINE ( 'NONE', #48398, #43371 ) ;
#40009 = DIRECTION ( 'NONE',  ( 0.000000000000000000, -1.000000000000000000, 0.000000000000000000 ) ) ;
#40010 = DIRECTION ( 'NONE',  ( -0.000000000000000000, -0.000000000000000000, 1.000000000000000000 ) ) ;
#40011 = EDGE_CURVE ( 'NONE', #18038, #34447, #31761, .T. ) ;
#40012 = ORIENTED_EDGE ( 'NONE', *, *, #36260, .F. ) ;
#40013 = CARTESIAN_POINT ( 'NONE',  ( 185.0000000000000000, -268.5000000000000000, -339.9999999999998863 ) ) ;
#40014 = CARTESIAN_POINT ( 'NONE',  ( 164.9999999999999716, -256.4999999999999432, -339.9999999999998863 ) ) ;
#40015 = EDGE_CURVE ( 'NONE', #26840, #16599, #21609, .T. ) ;
#40016 = ORIENTED_EDGE ( 'NONE', *, *, #30073, .F. ) ;
#40017 = CARTESIAN_POINT ( 'NONE',  ( -32.00969891772112419, -38.54699130261795403, -8.917361510505369182 ) ) ;
#40018 = DIRECTION ( 'NONE',  ( 1.000000000000000000, 0.000000000000000000, 0.000000000000000000 ) ) ;
#40019 = CARTESIAN_POINT ( 'NONE',  ( -0.8282505383454070724, -1.889063466747028297, 9.894754715216727448 ) ) ;
#40020 = ORIENTED_EDGE ( 'NONE', *, *, #35160, .T. ) ;
#40021 = ORIENTED_EDGE ( 'NONE', *, *, #26632, .F. ) ;
#40022 = ORIENTED_EDGE ( 'NONE', *, *, #13318, .F. ) ;
#40023 = ADVANCED_FACE ( 'NONE', ( #32756 ), #36886, .T. ) ;
#40024 = ADVANCED_FACE ( 'NONE', ( #16856 ), #6049, .F. ) ;
#40025 = CIRCLE ( 'NONE', #40816, 2.000000000000001776 ) ;
#40026 = ORIENTED_EDGE ( 'NONE', *, *, #26556, .T. ) ;
#40027 = CARTESIAN_POINT ( 'NONE',  ( -166.6959734468149463, -1.750000000000010214, 40.81828755692798438 ) ) ;
#40028 = CARTESIAN_POINT ( 'NONE',  ( -46.69597344681494633, -1.750000000000010658, 120.8182875569279702 ) ) ;
#40029 = VERTEX_POINT ( 'NONE', #20695 ) ;
#40030 = CARTESIAN_POINT ( 'NONE',  ( 73.30402655318508209, -1.750000000000010214, -39.18171244307202983 ) ) ;
#40031 = CARTESIAN_POINT ( 'NONE',  ( 113.3040265531850537, 1.749999999999996891, 0.8182875569279768335 ) ) ;
#40032 = EDGE_CURVE ( 'NONE', #44427, #48473, #13495, .T. ) ;
#40033 = LINE ( 'NONE', #43349, #1189 ) ;
#40034 = ADVANCED_FACE ( 'NONE', ( #33277 ), #1212, .T. ) ;
#40035 = DIRECTION ( 'NONE',  ( 0.000000000000000000, -1.000000000000000000, 0.000000000000000000 ) ) ;
#40036 = VERTEX_POINT ( 'NONE', #48100 ) ;
#40037 = EDGE_CURVE ( 'NONE', #43275, #10525, #31484, .T. ) ;
#40038 = FACE_OUTER_BOUND ( 'NONE', #23614, .T. ) ;
#40039 = ORIENTED_EDGE ( 'NONE', *, *, #31177, .T. ) ;
#40040 = DIRECTION ( 'NONE',  ( 1.000000000000000000, -0.000000000000000000, -0.000000000000000000 ) ) ;
#40041 = DIRECTION ( 'NONE',  ( 1.000000000000000000, 0.000000000000000000, 0.000000000000000000 ) ) ;
#40042 = ORIENTED_EDGE ( 'NONE', *, *, #34666, .F. ) ;
#40043 = PLANE ( 'NONE',  #19649 ) ;
#40044 = CYLINDRICAL_SURFACE ( 'NONE', #9553, 1.750000000000015543 ) ;
#40045 = B_SPLINE_SURFACE_WITH_KNOTS ( 'NONE', 3, 3, ( 
 ( #40168, #4259, #24274, #5004 ),
 ( #35839, #5258, #36598, #39668 ),
 ( #48060, #20151, #16310, #43498 ),
 ( #47567, #12450, #44242, #39426 ) ),
 .UNSPECIFIED., .F., .F., .F.,
 ( 4, 4 ),
 ( 4, 4 ),
 ( 0.000000000000000000, 1.000000000000000000 ),
 ( 0.000000000000000000, 1.000000000000000000 ),
 .UNSPECIFIED. ) ;
#40046 = ORIENTED_EDGE ( 'NONE', *, *, #4832, .T. ) ;
#40047 = LINE ( 'NONE', #20023, #9541 ) ;
#40048 = CARTESIAN_POINT ( 'NONE',  ( -13.59579750444763668, 10.60877755095910935, 8.727788335465566760 ) ) ;
#40049 = DIRECTION ( 'NONE',  ( -1.000000000000000000, -0.000000000000000000, -0.000000000000000000 ) ) ;
#40050 = CARTESIAN_POINT ( 'NONE',  ( -207.2473046169136808, -154.8119894309599260, 472.8425600500171981 ) ) ;
#40051 = EDGE_CURVE ( 'NONE', #38609, #31049, #45464, .T. ) ;
#40052 = ORIENTED_EDGE ( 'NONE', *, *, #2256, .F. ) ;
#40053 = PLANE ( 'NONE',  #19570 ) ;
#40054 = FACE_OUTER_BOUND ( 'NONE', #28110, .T. ) ;
#40055 = CARTESIAN_POINT ( 'NONE',  ( -5.000000000000000000, 165.2000000000000171, 359.7999999999997840 ) ) ;
#40056 = ORIENTED_EDGE ( 'NONE', *, *, #36574, .T. ) ;
#40057 = ORIENTED_EDGE ( 'NONE', *, *, #4201, .F. ) ;
#40058 = APPLICATION_PROTOCOL_DEFINITION ( 'draft international standard', 'automotive_design', 1998, #20728 ) ;
#40059 = FACE_OUTER_BOUND ( 'NONE', #48122, .T. ) ;
#40060 = DIRECTION ( 'NONE',  ( 1.000000000000000000, -0.000000000000000000, -0.000000000000000000 ) ) ;
#40061 = AXIS2_PLACEMENT_3D ( 'NONE', #42185, #38365, #34777 ) ;
#40062 = CARTESIAN_POINT ( 'NONE',  ( -33.16902712922616558, 37.70469005304312304, 1.847720168420772691 ) ) ;
#40063 = DIRECTION ( 'NONE',  ( -0.000000000000000000, -1.000000000000000000, -0.000000000000000000 ) ) ;
#40064 = LINE ( 'NONE', #35465, #9238 ) ;
#40065 = ORIENTED_EDGE ( 'NONE', *, *, #46921, .T. ) ;
#40066 = CARTESIAN_POINT ( 'NONE',  ( -214.9999999999999432, -173.0000000000000000, 112.0000000000000284 ) ) ;
#40067 = EDGE_CURVE ( 'NONE', #43972, #17766, #26301, .T. ) ;
#40068 = CARTESIAN_POINT ( 'NONE',  ( 191.5540265531851105, 0.000000000000000000, 165.0000000000000000 ) ) ;
#40069 = CARTESIAN_POINT ( 'NONE',  ( -0.8433491450857070193, 0.9182416014173486740, 9.981352469109932457 ) ) ;
#40070 = DIRECTION ( 'NONE',  ( -1.000000000000000000, 0.000000000000000000, 0.000000000000000000 ) ) ;
#40071 = ORIENTED_EDGE ( 'NONE', *, *, #17474, .T. ) ;
#40072 = CARTESIAN_POINT ( 'NONE',  ( -4.999999999999948486, -214.9999999999999716, -234.7500000000000000 ) ) ;
#40073 = VERTEX_POINT ( 'NONE', #5547 ) ;
#40074 = DIRECTION ( 'NONE',  ( 1.000000000000000000, 0.000000000000000000, 0.000000000000000000 ) ) ;
#40075 = ORIENTED_EDGE ( 'NONE', *, *, #30391, .F. ) ;
#40076 = CARTESIAN_POINT ( 'NONE',  ( 75.05402655318509630, 2.143131898507880377E-16, -157.4317124430720014 ) ) ;
#40077 = CARTESIAN_POINT ( 'NONE',  ( 84.99999999999997158, 17.00000000000000000, -114.9999999999999858 ) ) ;
#40078 = CARTESIAN_POINT ( 'NONE',  ( -128.4459734468149179, 0.000000000000000000, 42.56828755692794175 ) ) ;
#40079 = DIRECTION ( 'NONE',  ( 1.000000000000000000, 0.000000000000000000, -4.625929269271542120E-16 ) ) ;
#40080 = ORIENTED_EDGE ( 'NONE', *, *, #12422, .T. ) ;
#40081 = ADVANCED_FACE ( 'NONE', ( #29400 ), #25303, .T. ) ;
#40082 = CARTESIAN_POINT ( 'NONE',  ( -8.445973446814964092, 1.025126265847097207, 39.06828755692796307 ) ) ;
#40083 = ADVANCED_FACE ( 'NONE', ( #21196 ), #36638, .T. ) ;
#40084 = LINE ( 'NONE', #43653, #4986 ) ;
#40085 = ORIENTED_EDGE ( 'NONE', *, *, #48076, .F. ) ;
#40086 = CARTESIAN_POINT ( 'NONE',  ( -84.94597344681494633, 2.143131898507880377E-16, -0.9317124430720247208 ) ) ;
#40087 = DIRECTION ( 'NONE',  ( 0.4055129968046615185, 0.4055129968046615185, -0.8192181753629523833 ) ) ;
#40088 = CARTESIAN_POINT ( 'NONE',  ( 49.89397392339123627, -8.245536726716670373, 7.906207997025717304 ) ) ;
#40089 = DIRECTION ( 'NONE',  ( -0.000000000000000000, -0.000000000000000000, -1.000000000000000000 ) ) ;
#40090 = ORIENTED_EDGE ( 'NONE', *, *, #1295, .F. ) ;
#40091 = EDGE_CURVE ( 'NONE', #31059, #35508, #28902, .T. ) ;
#40092 = ORIENTED_EDGE ( 'NONE', *, *, #1571, .T. ) ;
#40093 = CARTESIAN_POINT ( 'NONE',  ( 195.0540265531851105, 2.143131898507880377E-16, -157.4317124430720582 ) ) ;
#40094 = EDGE_CURVE ( 'NONE', #960, #9715, #48604, .T. ) ;
#40095 = VECTOR ( 'NONE', #5534, 1000.000000000000000 ) ;
#40096 = EDGE_CURVE ( 'NONE', #6290, #26029, #50700, .T. ) ;
#40097 = AXIS2_PLACEMENT_3D ( 'NONE', #27999, #27504, #39311 ) ;
#40098 = EDGE_LOOP ( 'NONE', ( #24461, #36564, #17522, #22869, #42149, #32673 ) ) ;
#40099 = LINE ( 'NONE', #17914, #8579 ) ;
#40100 = LINE ( 'NONE', #848, #34951 ) ;
#40101 = CARTESIAN_POINT ( 'NONE',  ( 350.0000000000001137, 169.0000000000000000, 357.9999999999997726 ) ) ;
#40102 = ORIENTED_EDGE ( 'NONE', *, *, #30711, .F. ) ;
#40104 = VECTOR ( 'NONE', #16518, 1000.000000000000000 ) ;
#40103 = CARTESIAN_POINT ( 'NONE',  ( 30.00000000000029132, 17.00000000000000000, -84.99999999999998579 ) ) ;
#40105 = VECTOR ( 'NONE', #4345, 1000.000000000000000 ) ;
#40106 = EDGE_CURVE ( 'NONE', #37522, #10041, #50391, .T. ) ;
#40107 = CARTESIAN_POINT ( 'NONE',  ( 210.0000000000000568, 0.000000000000000000, -39.18171244307202983 ) ) ;
#40108 = DIRECTION ( 'NONE',  ( -1.000000000000000000, 0.000000000000000000, 0.000000000000000000 ) ) ;
#40109 = AXIS2_PLACEMENT_3D ( 'NONE', #46460, #11351, #32125 ) ;
#40110 = CARTESIAN_POINT ( 'NONE',  ( 177.5000000000000284, -102.5000000000000142, 10.00000000000000000 ) ) ;
#40111 = ORIENTED_EDGE ( 'NONE', *, *, #45596, .F. ) ;
#40112 = ORIENTED_EDGE ( 'NONE', *, *, #44350, .F. ) ;
#40113 = ORIENTED_EDGE ( 'NONE', *, *, #2602, .F. ) ;
#40114 = CARTESIAN_POINT ( 'NONE',  ( -225.0000000000000568, 164.9999999999999716, 352.0000000000000000 ) ) ;
#40115 = DIRECTION ( 'NONE',  ( 1.000000000000000000, 0.000000000000000000, 0.000000000000000000 ) ) ;
#40116 = FACE_OUTER_BOUND ( 'NONE', #25834, .T. ) ;
#40117 = ORIENTED_EDGE ( 'NONE', *, *, #9276, .T. ) ;
#40118 = CARTESIAN_POINT ( 'NONE',  ( -164.9459734468149463, 2.143131898507880377E-16, 165.0000000000000000 ) ) ;
#40119 = ORIENTED_EDGE ( 'NONE', *, *, #3966, .T. ) ;
#40120 = CARTESIAN_POINT ( 'NONE',  ( -44.99506233596265048, -23.32283626942287569, 7.455576670931136185 ) ) ;
#40121 = VERTEX_POINT ( 'NONE', #27095 ) ;
#40122 = LINE ( 'NONE', #32937, #17941 ) ;
#40123 = CARTESIAN_POINT ( 'NONE',  ( -88.44597344681494633, -1.025126265847089213, -160.9317124430720014 ) ) ;
#40124 = CARTESIAN_POINT ( 'NONE',  ( 9.358026734184097251, 0.000000000000000000, 0.000000000000000000 ) ) ;
#40125 = CARTESIAN_POINT ( 'NONE',  ( 1.066995270233474624, -33.23888904628638841, -3.760136334089591248 ) ) ;
#40126 = EDGE_LOOP ( 'NONE', ( #30476, #44706, #23438 ) ) ;
#40127 = PLANE ( 'NONE',  #39512 ) ;
#40128 =( BOUNDED_CURVE ( )  B_SPLINE_CURVE ( 3, ( #32577, #24616, #9201, #8722 ),
 .UNSPECIFIED., .F., .F. ) 
 B_SPLINE_CURVE_WITH_KNOTS ( ( 4, 4 ),
 ( 0.000000000000000000, 1.570796326794896558 ),
 .UNSPECIFIED. ) 
 CURVE ( )  GEOMETRIC_REPRESENTATION_ITEM ( )  RATIONAL_B_SPLINE_CURVE ( ( 1.000000000000000000, 0.8047378541243649375, 0.8047378541243649375, 1.000000000000000000 ) ) 
 REPRESENTATION_ITEM ( '' )  );
#40129 = CARTESIAN_POINT ( 'NONE',  ( 153.3040265531850537, -1.750000000000009992, 160.8182875569279702 ) ) ;
#40130 = CARTESIAN_POINT ( 'NONE',  ( 339.9999999999999432, 183.0000000000000284, -356.0000000000002274 ) ) ;
#40131 = AXIS2_PLACEMENT_3D ( 'NONE', #33403, #48732, #13118 ) ;
#40132 = ADVANCED_FACE ( 'NONE', ( #34288 ), #35325, .F. ) ;
#40133 = VECTOR ( 'NONE', #2009, 1000.000000000000000 ) ;
#40134 = VECTOR ( 'NONE', #16906, 1000.000000000000000 ) ;
#40135 = CYLINDRICAL_SURFACE ( 'NONE', #24779, 1.750000000000015543 ) ;
#40136 = ORIENTED_EDGE ( 'NONE', *, *, #17382, .F. ) ;
#40137 = DIRECTION ( 'NONE',  ( -1.586032892321652236E-16, -1.000000000000000000, -2.288264760618012091E-48 ) ) ;
#40138 = VERTEX_POINT ( 'NONE', #3472 ) ;
#40139 = VECTOR ( 'NONE', #37523, 1000.000000000000000 ) ;
#40140 = LINE ( 'NONE', #1642, #13084 ) ;
#40141 = CARTESIAN_POINT ( 'NONE',  ( -210.0000000000000568, 0.000000000000000000, -117.4317124430720298 ) ) ;
#40142 = EDGE_LOOP ( 'NONE', ( #39253, #27515, #16555, #11512, #22733, #21044, #1505, #50630, #32210, #36119 ) ) ;
#40143 = CARTESIAN_POINT ( 'NONE',  ( -48.98697415750977768, -11.03699497439218646, -8.016098858316199838 ) ) ;
#40144 = CARTESIAN_POINT ( 'NONE',  ( 73.30402655318508209, 0.000000000000000000, 165.0000000000000000 ) ) ;
#40145 = VERTEX_POINT ( 'NONE', #2966 ) ;
#40146 = ORIENTED_EDGE ( 'NONE', *, *, #16221, .F. ) ;
#40147 = CARTESIAN_POINT ( 'NONE',  ( -0.4154044336478688315, 2.070917815000994811, 9.890170120223993777 ) ) ;
#40148 = CARTESIAN_POINT ( 'NONE',  ( -0.3862712429686729343, -1.188820645368946050, 10.00000000000000000 ) ) ;
#40149 = EDGE_CURVE ( 'NONE', #30248, #18098, #42188, .T. ) ;
#40150 = ADVANCED_FACE ( 'NONE', ( #31458 ), #27347, .F. ) ;
#40151 = ORIENTED_EDGE ( 'NONE', *, *, #34310, .T. ) ;
#40152 = EDGE_LOOP ( 'NONE', ( #26180, #17412, #47463, #12055 ) ) ;
#40153 = DIRECTION ( 'NONE',  ( 1.000000000000000000, 0.000000000000000000, 0.000000000000000000 ) ) ;
#40154 = CARTESIAN_POINT ( 'NONE',  ( -205.6708471809678827, 1.750000000000009548, -0.2068387089191121020 ) ) ;
#40155 = ORIENTED_EDGE ( 'NONE', *, *, #42103, .F. ) ;
#40156 = EDGE_LOOP ( 'NONE', ( #18588, #7656, #43244, #27276 ) ) ;
#40157 = EDGE_CURVE ( 'NONE', #5061, #22675, #4879, .T. ) ;
#40158 = EDGE_LOOP ( 'NONE', ( #44533, #22962, #46603 ) ) ;
#40159 = B_SPLINE_CURVE_WITH_KNOTS ( 'NONE', 3,
 ( #31240, #7891, #8141, #7376 ),
 .UNSPECIFIED., .F., .F.,
 ( 4, 4 ),
 ( 0.001152428489661405653, 0.001623376834729593982 ),
 .UNSPECIFIED. ) ;
#40160 = VECTOR ( 'NONE', #34591, 1000.000000000000000 ) ;
#40161 = CARTESIAN_POINT ( 'NONE',  ( -44.94597344681493922, 2.143131898507880377E-16, 165.0000000000000000 ) ) ;
#40162 = AXIS2_PLACEMENT_3D ( 'NONE', #39583, #39086, #3905 ) ;
#40163 = VECTOR ( 'NONE', #33264, 1000.000000000000000 ) ;
#40164 = DIRECTION ( 'NONE',  ( 1.333906992743555050E-23, -1.000000000000000000, 0.000000000000000000 ) ) ;
#40165 = EDGE_LOOP ( 'NONE', ( #13576, #26318, #24512, #36342 ) ) ;
#40166 = ORIENTED_EDGE ( 'NONE', *, *, #10431, .T. ) ;
#40167 = VECTOR ( 'NONE', #37468, 1000.000000000000000 ) ;
#40168 = CARTESIAN_POINT ( 'NONE',  ( -22.69295089195507487, -45.31600496604688999, 7.455576670931136185 ) ) ;
#40169 = VECTOR ( 'NONE', #40049, 1000.000000000000000 ) ;
#40170 = FACE_OUTER_BOUND ( 'NONE', #29492, .T. ) ;
#40171 = ORIENTED_EDGE ( 'NONE', *, *, #50589, .F. ) ;
#40172 = ORIENTED_EDGE ( 'NONE', *, *, #33777, .T. ) ;
#40173 = FACE_OUTER_BOUND ( 'NONE', #13613, .T. ) ;
#40174 = DIRECTION ( 'NONE',  ( -1.000000000000000000, 0.000000000000000000, 0.000000000000000000 ) ) ;
#40175 = ORIENTED_EDGE ( 'NONE', *, *, #16501, .T. ) ;
#40176 = AXIS2_PLACEMENT_3D ( 'NONE', #50047, #43171, #15456 ) ;
#40177 = CARTESIAN_POINT ( 'NONE',  ( -166.6959734468149463, 0.000000000000000000, 165.0000000000000000 ) ) ;
#40178 = FACE_OUTER_BOUND ( 'NONE', #5623, .T. ) ;
#40179 = FACE_OUTER_BOUND ( 'NONE', #12427, .T. ) ;
#40180 = DIRECTION ( 'NONE',  ( 1.000000000000000000, 0.000000000000000000, 0.000000000000000000 ) ) ;
#40181 = ORIENTED_EDGE ( 'NONE', *, *, #2920, .F. ) ;
#40182 = CARTESIAN_POINT ( 'NONE',  ( -5.000000000000000000, -184.7999999999999545, 340.1999999999997044 ) ) ;
#40183 = DIRECTION ( 'NONE',  ( 0.000000000000000000, 0.000000000000000000, 1.000000000000000000 ) ) ;
#40184 = CARTESIAN_POINT ( 'NONE',  ( -165.6708471809677974, 1.750000000000010214, -118.1565861772249519 ) ) ;
#40185 = EDGE_CURVE ( 'NONE', #27664, #13545, #42470, .T. ) ;
#40186 = CARTESIAN_POINT ( 'NONE',  ( -44.99506233596265048, -23.32283626942287569, 7.455576670931136185 ) ) ;
#40187 = CARTESIAN_POINT ( 'NONE',  ( 31.55402655318503236, 0.000000000000000000, 119.0682875569279702 ) ) ;
#40188 = CARTESIAN_POINT ( 'NONE',  ( -1.782521105131510186, 0.3635605703594341209, 9.903764339332088440 ) ) ;
#40189 = CARTESIAN_POINT ( 'NONE',  ( 154.3291528190321458, 1.750000000000009548, -160.2068387089191219 ) ) ;
#40190 = VECTOR ( 'NONE', #36952, 1000.000000000000000 ) ;
#40191 = EDGE_LOOP ( 'NONE', ( #42423, #31842, #28734, #34314 ) ) ;
#40192 = CARTESIAN_POINT ( 'NONE',  ( 32.27890028733795447, 1.750000000000009548, 121.8434138227750623 ) ) ;
#40193 = VECTOR ( 'NONE', #40323, 1000.000000000000000 ) ;
#40194 = PLANE ( 'NONE',  #40994 ) ;
#40195 = VERTEX_POINT ( 'NONE', #7343 ) ;
#40196 = CARTESIAN_POINT ( 'NONE',  ( -24.39427009666018265, -44.07992421011638129, 8.807470649214879543 ) ) ;
#40197 = CARTESIAN_POINT ( 'NONE',  ( 155.0540265531850537, 2.143131898507880377E-16, 39.06828755692798438 ) ) ;
#40198 = AXIS2_PLACEMENT_3D ( 'NONE', #39666, #43747, #24014 ) ;
#40199 = CARTESIAN_POINT ( 'NONE',  ( 30.00000000000029132, 17.00000000000000000, -60.00000000000000000 ) ) ;
#40200 = ORIENTED_EDGE ( 'NONE', *, *, #8710, .T. ) ;
#40201 = DIRECTION ( 'NONE',  ( 1.000000000000000000, -0.000000000000000000, -0.000000000000000000 ) ) ;
#40202 = VECTOR ( 'NONE', #13285, 1000.000000000000000 ) ;
#40203 = ORIENTED_EDGE ( 'NONE', *, *, #47570, .F. ) ;
#40204 = ORIENTED_EDGE ( 'NONE', *, *, #36880, .F. ) ;
#40205 = FACE_OUTER_BOUND ( 'NONE', #4100, .T. ) ;
#40206 = DIRECTION ( 'NONE',  ( -1.000000000000000000, -0.000000000000000000, -0.000000000000000000 ) ) ;
#40207 = VERTEX_POINT ( 'NONE', #38652 ) ;
#40208 = FACE_OUTER_BOUND ( 'NONE', #3686, .T. ) ;
#40209 = LINE ( 'NONE', #28910, #13435 ) ;
#40210 = ORIENTED_EDGE ( 'NONE', *, *, #135, .F. ) ;
#40211 = ORIENTED_EDGE ( 'NONE', *, *, #858, .F. ) ;
#40212 = EDGE_CURVE ( 'NONE', #40007, #37708, #46505, .T. ) ;
#40213 = FACE_OUTER_BOUND ( 'NONE', #18382, .T. ) ;
#40214 = EDGE_LOOP ( 'NONE', ( #13251, #12911, #11895, #16659, #14257, #38460 ) ) ;
#40215 = CARTESIAN_POINT ( 'NONE',  ( 2.499999999999956035, -194.9999999999999716, -240.0000000000000000 ) ) ;
#40216 = CARTESIAN_POINT ( 'NONE',  ( 153.3040265531850537, 1.750000000000009992, 160.8182875569279702 ) ) ;
#40217 = CARTESIAN_POINT ( 'NONE',  ( -1.080000014127418639, -0.7606467978654640749, 9.943883492372872723 ) ) ;
#40218 = ORIENTED_EDGE ( 'NONE', *, *, #45272, .T. ) ;
#40219 = CARTESIAN_POINT ( 'NONE',  ( 14.49999999999999822, 12.98684210526315930, 0.000000000000000000 ) ) ;
#40220 = CARTESIAN_POINT ( 'NONE',  ( 14.48769039275578407, 30.44468701195595983, 8.807470649214879543 ) ) ;
#40221 = ORIENTED_EDGE ( 'NONE', *, *, #9536, .T. ) ;
#40222 = VERTEX_POINT ( 'NONE', #11958 ) ;
#40223 = ORIENTED_EDGE ( 'NONE', *, *, #36494, .T. ) ;
#40224 = CARTESIAN_POINT ( 'NONE',  ( 7.749480817862238524, 14.85497772329518895, 9.403735324607438884 ) ) ;
#40225 = ADVANCED_FACE ( 'NONE', ( #30697 ), #11693, .T. ) ;
#40226 = DIRECTION ( 'NONE',  ( -0.000000000000000000, -1.000000000000000000, -0.000000000000000000 ) ) ;
#40227 = EDGE_LOOP ( 'NONE', ( #39094, #10957 ) ) ;
#40228 = EDGE_CURVE ( 'NONE', #29772, #37058, #7863, .T. ) ;
#40229 = AXIS2_PLACEMENT_3D ( 'NONE', #32261, #32015, #36642 ) ;
#40230 = CARTESIAN_POINT ( 'NONE',  ( -87.72109971266203843, -1.750000000000010214, -120.2068387089191219 ) ) ;
#40231 = FACE_OUTER_BOUND ( 'NONE', #9699, .T. ) ;
#40232 = EDGE_CURVE ( 'NONE', #13622, #25002, #46040, .T. ) ;
#40233 = LINE ( 'NONE', #44304, #39541 ) ;
#40234 = AXIS2_PLACEMENT_3D ( 'NONE', #17737, #43913, #5922 ) ;
#40235 = PLANE ( 'NONE',  #38313 ) ;
#40236 = CARTESIAN_POINT ( 'NONE',  ( -19.99999999999846523, 16.00000000000000000, 60.00000000000000000 ) ) ;
#40237 = LINE ( 'NONE', #8933, #16719 ) ;
#40238 = CYLINDRICAL_SURFACE ( 'NONE', #37416, 2.000000000000001776 ) ;
#40239 = CARTESIAN_POINT ( 'NONE',  ( 113.3040265531850537, 0.000000000000000000, 165.0000000000000000 ) ) ;
#40240 = CARTESIAN_POINT ( 'NONE',  ( -87.72109971266203843, -1.750000000000009548, -158.1565861772249377 ) ) ;
#40241 = VECTOR ( 'NONE', #43466, 1000.000000000000000 ) ;
#40242 = EDGE_CURVE ( 'NONE', #45334, #32429, #30825, .T. ) ;
#40243 = CARTESIAN_POINT ( 'NONE',  ( -27.73884755486766096, 25.23502201956265978, 7.697694107796191787 ) ) ;
#40244 = EDGE_CURVE ( 'NONE', #47433, #13085, #48448, .T. ) ;
#40245 = DIRECTION ( 'NONE',  ( 0.000000000000000000, 0.000000000000000000, 1.000000000000000000 ) ) ;
#40246 = EDGE_CURVE ( 'NONE', #47361, #22212, #8584, .T. ) ;
#40247 = DIRECTION ( 'NONE',  ( 0.000000000000000000, 0.000000000000000000, -1.000000000000000000 ) ) ;
#40248 = VERTEX_POINT ( 'NONE', #44912 ) ;
#40249 = CYLINDRICAL_SURFACE ( 'NONE', #16353, 1.750000000000001554 ) ;
#40250 = DIRECTION ( 'NONE',  ( -0.000000000000000000, 0.000000000000000000, -1.000000000000000000 ) ) ;
#40251 = CARTESIAN_POINT ( 'NONE',  ( -14.99999999999782041, 17.00000000000000000, 115.0000000000000142 ) ) ;
#40252 = DIRECTION ( 'NONE',  ( 0.000000000000000000, 0.000000000000000000, -1.000000000000000000 ) ) ;
#40253 =( BOUNDED_CURVE ( )  B_SPLINE_CURVE ( 3, ( #7764, #22887, #38566, #11344 ),
 .UNSPECIFIED., .F., .F. ) 
 B_SPLINE_CURVE_WITH_KNOTS ( ( 4, 4 ),
 ( 4.712388980384689674, 6.283185307179586232 ),
 .UNSPECIFIED. ) 
 CURVE ( )  GEOMETRIC_REPRESENTATION_ITEM ( )  RATIONAL_B_SPLINE_CURVE ( ( 1.000000000000000000, 0.8047378541243649375, 0.8047378541243649375, 1.000000000000000000 ) ) 
 REPRESENTATION_ITEM ( '' )  );
#40254 = VERTEX_POINT ( 'NONE', #47998 ) ;
#40255 = DIRECTION ( 'NONE',  ( -1.000000000000000000, 0.000000000000000000, 0.000000000000000000 ) ) ;
#40256 = CARTESIAN_POINT ( 'NONE',  ( -210.0000000000000568, 0.000000000000000000, 0.8182875569279768335 ) ) ;
#40257 = ORIENTED_EDGE ( 'NONE', *, *, #4619, .F. ) ;
#40258 = CARTESIAN_POINT ( 'NONE',  ( -32.57680531928949108, -38.13496438397444877, -8.466730184410787174 ) ) ;
#40259 = CARTESIAN_POINT ( 'NONE',  ( 35.00000000000186162, 16.00000000000000000, 65.00000000000000000 ) ) ;
#40260 = CARTESIAN_POINT ( 'NONE',  ( 35.00000000000122213, 16.00000000000000000, 5.000000000000004441 ) ) ;
#40261 =( BOUNDED_CURVE ( )  B_SPLINE_CURVE ( 3, ( #16597, #32256, #4297, #35616 ),
 .UNSPECIFIED., .F., .F. ) 
 B_SPLINE_CURVE_WITH_KNOTS ( ( 4, 4 ),
 ( 4.712388980384689674, 6.283185307179586232 ),
 .UNSPECIFIED. ) 
 CURVE ( )  GEOMETRIC_REPRESENTATION_ITEM ( )  RATIONAL_B_SPLINE_CURVE ( ( 1.000000000000000000, 0.8047378541243649375, 0.8047378541243649375, 1.000000000000000000 ) ) 
 REPRESENTATION_ITEM ( '' )  );
#40262 = EDGE_LOOP ( 'NONE', ( #30076, #1911, #22233, #27083, #36756 ) ) ;
#40263 = DIRECTION ( 'NONE',  ( -1.000000000000000000, 4.996003610813203446E-16, 1.586032878436834529E-16 ) ) ;
#40264 = EDGE_CURVE ( 'NONE', #20298, #40360, #43242, .T. ) ;
#40265 = ORIENTED_EDGE ( 'NONE', *, *, #32471, .T. ) ;
#40266 = ORIENTED_EDGE ( 'NONE', *, *, #47865, .T. ) ;
#40267 = VECTOR ( 'NONE', #28552, 1000.000000000000000 ) ;
#40268 = EDGE_CURVE ( 'NONE', #40908, #40762, #43247, .T. ) ;
#40269 = ADVANCED_FACE ( 'NONE', ( #13882 ), #39421, .F. ) ;
#40270 = ORIENTED_EDGE ( 'NONE', *, *, #9250, .F. ) ;
#40271 = LINE ( 'NONE', #13557, #37673 ) ;
#40272 = FACE_OUTER_BOUND ( 'NONE', #45093, .T. ) ;
#40273 = ORIENTED_EDGE ( 'NONE', *, *, #41003, .T. ) ;
#40274 = CARTESIAN_POINT ( 'NONE',  ( 181.0000000000000284, -174.9999999999999716, -115.0000000000001563 ) ) ;
#40275 = FACE_OUTER_BOUND ( 'NONE', #37357, .T. ) ;
#40276 = EDGE_CURVE ( 'NONE', #41270, #27700, #36384, .T. ) ;
#40277 = CARTESIAN_POINT ( 'NONE',  ( 350.0000000000001137, 167.0000000000000000, 355.9999999999997726 ) ) ;
#40278 =( BOUNDED_CURVE ( )  B_SPLINE_CURVE ( 3, ( #26593, #15802, #47060, #42237 ),
 .UNSPECIFIED., .F., .F. ) 
 B_SPLINE_CURVE_WITH_KNOTS ( ( 4, 4 ),
 ( 0.000000000000000000, 1.570796326794896558 ),
 .UNSPECIFIED. ) 
 CURVE ( )  GEOMETRIC_REPRESENTATION_ITEM ( )  RATIONAL_B_SPLINE_CURVE ( ( 1.000000000000000000, 0.8047378541243649375, 0.8047378541243649375, 1.000000000000000000 ) ) 
 REPRESENTATION_ITEM ( '' )  );
#40279 = CIRCLE ( 'NONE', #25544, 3.749999999999975575 ) ;
#40280 = LINE ( 'NONE', #1027, #24344 ) ;
#40281 = VERTEX_POINT ( 'NONE', #25199 ) ;
#40282 = ADVANCED_FACE ( 'NONE', ( #44179 ), #41103, .T. ) ;
#40283 = DIRECTION ( 'NONE',  ( 2.958228394578794708E-31, 0.000000000000000000, -1.000000000000000000 ) ) ;
#40284 = ORIENTED_EDGE ( 'NONE', *, *, #22527, .F. ) ;
#40285 = DIRECTION ( 'NONE',  ( -0.000000000000000000, -0.000000000000000000, 1.000000000000000000 ) ) ;
#40286 = CARTESIAN_POINT ( 'NONE',  ( 357.1715728752537871, -167.0000000000001137, -342.0000000000002842 ) ) ;
#40287 = ORIENTED_EDGE ( 'NONE', *, *, #30414, .T. ) ;
#40288 = ORIENTED_EDGE ( 'NONE', *, *, #14123, .F. ) ;
#40289 = CARTESIAN_POINT ( 'NONE',  ( 194.3291528190321742, 1.750000000000010214, 81.84341382277507648 ) ) ;
#40290 = DIRECTION ( 'NONE',  ( -0.000000000000000000, -0.000000000000000000, -1.000000000000000000 ) ) ;
#40291 = ORIENTED_EDGE ( 'NONE', *, *, #23730, .T. ) ;
#40292 = CARTESIAN_POINT ( 'NONE',  ( -166.6959734468149463, -1.750000000000009992, 160.8182875569279702 ) ) ;
#40293 = DIRECTION ( 'NONE',  ( 1.000000000000000000, 0.000000000000000000, 0.000000000000000000 ) ) ;
#40294 = CARTESIAN_POINT ( 'NONE',  ( 5.888214538810389698, 16.20866436362417673, 8.727788335465566760 ) ) ;
#40295 = VERTEX_POINT ( 'NONE', #2110 ) ;
#40296 = DIRECTION ( 'NONE',  ( -1.000000000000000000, 0.000000000000000000, 1.860490536778032451E-50 ) ) ;
#40297 = VECTOR ( 'NONE', #33880, 1000.000000000000000 ) ;
#40298 = CARTESIAN_POINT ( 'NONE',  ( 74.32915281903215998, 1.750000000000010214, 79.79316129108087807 ) ) ;
#40299 = EDGE_CURVE ( 'NONE', #3248, #5747, #47027, .T. ) ;
#40300 = ORIENTED_EDGE ( 'NONE', *, *, #20169, .F. ) ;
#40301 = ADVANCED_FACE ( 'NONE', ( #12888 ), #20844, .F. ) ;
#40302 = ORIENTED_EDGE ( 'NONE', *, *, #8586, .F. ) ;
#40303 = SHAPE_DEFINITION_REPRESENTATION ( #34362, #8742 ) ;
#40304 = PLANE ( 'NONE',  #27787 ) ;
#40305 = DIRECTION ( 'NONE',  ( -1.000000000000000000, -0.000000000000000000, -0.000000000000000000 ) ) ;
#40306 = ADVANCED_FACE ( 'NONE', ( #9789 ), #32401, .T. ) ;
#40307 = EDGE_CURVE ( 'NONE', #9722, #28214, #1105, .T. ) ;
#40308 = VECTOR ( 'NONE', #1879, 1000.000000000000000 ) ;
#40309 = CARTESIAN_POINT ( 'NONE',  ( -49.75871208702130133, 40.58472229863599523, -5.000000000000000000 ) ) ;
#40310 = CARTESIAN_POINT ( 'NONE',  ( -164.9459734468149463, 1.025126265847089657, -120.9317124430720440 ) ) ;
#40311 = ORIENTED_EDGE ( 'NONE', *, *, #24387, .T. ) ;
#40312 = EDGE_CURVE ( 'NONE', #42092, #24012, #21595, .T. ) ;
#40313 = CARTESIAN_POINT ( 'NONE',  ( 30.00000000000153833, 17.00000000000000000, 35.00000000000000000 ) ) ;
#40314 = EDGE_CURVE ( 'NONE', #17183, #11317, #5946, .T. ) ;
#40315 = CARTESIAN_POINT ( 'NONE',  ( 350.0000000000000000, 165.0000000000000000, -344.0000000000001705 ) ) ;
#40316 = DIRECTION ( 'NONE',  ( -1.000000000000000000, 0.000000000000000000, -0.000000000000000000 ) ) ;
#40317 = CARTESIAN_POINT ( 'NONE',  ( -0.05286079371165668117, 1.230216489825517234, 9.975326647350888365 ) ) ;
#40318 = EDGE_LOOP ( 'NONE', ( #25468, #2510, #6731, #2478 ) ) ;
#40319 = FACE_OUTER_BOUND ( 'NONE', #38704, .T. ) ;
#40320 = ORIENTED_EDGE ( 'NONE', *, *, #27163, .F. ) ;
#40321 = CARTESIAN_POINT ( 'NONE',  ( 115.0540265531850395, -1.025126265847081886, -40.93171244307202272 ) ) ;
#40322 = EDGE_LOOP ( 'NONE', ( #23705, #11937, #2460, #44436 ) ) ;
#40323 = DIRECTION ( 'NONE',  ( -1.000000000000000000, 0.000000000000000000, -7.793956916774525800E-48 ) ) ;
#40324 = CARTESIAN_POINT ( 'NONE',  ( 168.9999999999999716, -254.5000000000000000, -114.9999999999999574 ) ) ;
#40325 = DIRECTION ( 'NONE',  ( 1.000000000000000000, 0.000000000000000000, 0.000000000000000000 ) ) ;
#40326 = DIRECTION ( 'NONE',  ( -0.000000000000000000, -0.000000000000000000, -1.000000000000000000 ) ) ;
#40327 = VERTEX_POINT ( 'NONE', #37289 ) ;
#40328 = ADVANCED_FACE ( 'NONE', ( #48251 ), #33175, .F. ) ;
#40329 = CARTESIAN_POINT ( 'NONE',  ( -124.9459734468149321, 1.025126265847081442, -0.9317124430720195027 ) ) ;
#40330 = EDGE_CURVE ( 'NONE', #44943, #11648, #5192, .T. ) ;
#40331 = VERTEX_POINT ( 'NONE', #24958 ) ;
#40332 = CARTESIAN_POINT ( 'NONE',  ( 152.2789002873379900, -1.750000000000009548, -160.2068387089191219 ) ) ;
#40333 = CARTESIAN_POINT ( 'NONE',  ( 33.30402655318503946, 0.000000000000000000, 165.0000000000000000 ) ) ;
#40334 = CARTESIAN_POINT ( 'NONE',  ( -6.880036658038815922, -222.4999999999999716, -228.6347188485896140 ) ) ;
#40335 = CARTESIAN_POINT ( 'NONE',  ( 75.05402655318509630, -1.025126265847088991, 159.0682875569279418 ) ) ;
#40336 = AXIS2_PLACEMENT_3D ( 'NONE', #40050, #4873, #43620 ) ;
#40337 = LINE ( 'NONE', #10039, #43517 ) ;
#40338 = ORIENTED_EDGE ( 'NONE', *, *, #18322, .T. ) ;
#40339 = PRODUCT_RELATED_PRODUCT_CATEGORY ( 'part', '', ( #49848 ) ) ;
#40340 = ORIENTED_EDGE ( 'NONE', *, *, #38200, .T. ) ;
#40341 = CARTESIAN_POINT ( 'NONE',  ( -0.2553898474591131396, 1.933866572595240640, 9.896373613412551506 ) ) ;
#40342 = VECTOR ( 'NONE', #31429, 1000.000000000000000 ) ;
#40343 = EDGE_LOOP ( 'NONE', ( #7857, #46462, #31461, #43796, #44537 ) ) ;
#40344 = CIRCLE ( 'NONE', #41134, 2.000000000000001776 ) ;
#40345 = FACE_OUTER_BOUND ( 'NONE', #33650, .T. ) ;
#40346 = CARTESIAN_POINT ( 'NONE',  ( -208.4459734468148611, -1.025126265847089657, -120.9317124430720440 ) ) ;
#40347 = CARTESIAN_POINT ( 'NONE',  ( 35.05402655318504657, 2.143131898507880377E-16, -120.9317124430720725 ) ) ;
#40348 = ORIENTED_EDGE ( 'NONE', *, *, #2519, .T. ) ;
#40349 = CARTESIAN_POINT ( 'NONE',  ( 355.9999999999999432, -185.0000000000001421, 360.0000000000000000 ) ) ;
#40350 = ADVANCED_FACE ( 'NONE', ( #28804, #44668 ), #21345, .T. ) ;
#40351 = CARTESIAN_POINT ( 'NONE',  ( -166.6959734468149463, 0.000000000000000000, 165.0000000000000000 ) ) ;
#40352 = B_SPLINE_SURFACE_WITH_KNOTS ( 'NONE', 3, 3, ( 
 ( #5028, #41451, #18336, #9646 ),
 ( #21191, #49101, #40705, #17343 ),
 ( #37626, #29649, #21691, #1952 ),
 ( #2694, #14241, #2206, #22208 ) ),
 .UNSPECIFIED., .F., .F., .F.,
 ( 4, 4 ),
 ( 4, 4 ),
 ( 0.000000000000000000, 1.000000000000000000 ),
 ( 0.000000000000000000, 1.000000000000000000 ),
 .UNSPECIFIED. ) ;
#40353 = CARTESIAN_POINT ( 'NONE',  ( 1.249999999999999778, -0.000000000000000000, -10.00000000000000000 ) ) ;
#40354 = CARTESIAN_POINT ( 'NONE',  ( -49.46074318306826001, 9.578883844007169301, 8.807470649214879543 ) ) ;
#40355 = DIRECTION ( 'NONE',  ( 0.000000000000000000, 0.000000000000000000, 1.000000000000000000 ) ) ;
#40356 = DIRECTION ( 'NONE',  ( -1.156482317317870492E-16, 1.000000000000000000, 0.000000000000000000 ) ) ;
#40357 = ORIENTED_EDGE ( 'NONE', *, *, #10641, .T. ) ;
#40358 = VERTEX_POINT ( 'NONE', #34686 ) ;
#40359 = EDGE_CURVE ( 'NONE', #4058, #22032, #36079, .T. ) ;
#40360 = VERTEX_POINT ( 'NONE', #2591 ) ;
#40361 = DIRECTION ( 'NONE',  ( 1.000000000000000000, 0.000000000000000000, -0.000000000000000000 ) ) ;
#40362 = CARTESIAN_POINT ( 'NONE',  ( -4.945973446814903696, 2.143131898507912917E-16, 122.5682875569279986 ) ) ;
#40363 = DIRECTION ( 'NONE',  ( -3.172065784643302499E-16, -1.000000000000000000, 2.537652627714642000E-15 ) ) ;
#40364 = AXIS2_PLACEMENT_3D ( 'NONE', #50059, #2887, #7532 ) ;
#40365 = DIRECTION ( 'NONE',  ( 0.000000000000000000, 0.000000000000000000, 1.000000000000000000 ) ) ;
#40366 = VERTEX_POINT ( 'NONE', #26721 ) ;
#40367 = CARTESIAN_POINT ( 'NONE',  ( -48.33712804702535948, -13.03701565032741527, -9.367992836599954742 ) ) ;
#40368 = ORIENTED_EDGE ( 'NONE', *, *, #29300, .T. ) ;
#40369 = SHAPE_REPRESENTATION_RELATIONSHIP ( 'NONE' , 'NONE' ,  #8742, #33210 ) ;
#40370 = CARTESIAN_POINT ( 'NONE',  ( -6.875132362119187768, 33.14667368551891258, 8.356839323120299312 ) ) ;
#40371 = CARTESIAN_POINT ( 'NONE',  ( 1.377509002708426689, -0.6027468487254984408, 9.927319414211227766 ) ) ;
#40372 = PLANE ( 'NONE',  #47927 ) ;
#40373 = ADVANCED_FACE ( 'NONE', ( #6212 ), #19000, .T. ) ;
#40374 = EDGE_CURVE ( 'NONE', #8918, #27492, #11483, .T. ) ;
#40375 = CARTESIAN_POINT ( 'NONE',  ( -166.6959734468149463, 1.750000000000009992, 160.8182875569279702 ) ) ;
#40376 = CARTESIAN_POINT ( 'NONE',  ( 0.000000000000000000, 0.000000000000000000, -240.0000000000000000 ) ) ;
#40377 = AXIS2_PLACEMENT_3D ( 'NONE', #36143, #44060, #4810 ) ;
#40378 = CARTESIAN_POINT ( 'NONE',  ( -0.3370904143228927730, -0.2449105217885335917, 10.00000000000000000 ) ) ;
#40379 = VERTEX_POINT ( 'NONE', #22105 ) ;
#40380 = CARTESIAN_POINT ( 'NONE',  ( 183.0000000000000284, -174.9999999999999716, -111.0000000000001563 ) ) ;
#40381 = AXIS2_PLACEMENT_3D ( 'NONE', #43684, #16253, #35785 ) ;
#40382 = EDGE_CURVE ( 'NONE', #29172, #4462, #44866, .T. ) ;
#40383 = DIRECTION ( 'NONE',  ( 1.000000000000000000, -4.758098676964957447E-16, 2.958228394578795584E-31 ) ) ;
#40384 = DIRECTION ( 'NONE',  ( 0.000000000000000000, 1.000000000000000000, 1.544785076050074834E-48 ) ) ;
#40385 = VECTOR ( 'NONE', #44389, 1000.000000000000000 ) ;
#40386 = EDGE_CURVE ( 'NONE', #20063, #35915, #1307, .T. ) ;
#40387 = EDGE_CURVE ( 'NONE', #4113, #42347, #49254, .T. ) ;
#40388 = PLANE ( 'NONE',  #45316 ) ;
#40389 = EDGE_LOOP ( 'NONE', ( #49242, #49658, #40653, #12389 ) ) ;
#40390 = AXIS2_PLACEMENT_3D ( 'NONE', #19017, #45691, #7498 ) ;
#40391 = CARTESIAN_POINT ( 'NONE',  ( -88.44597344681497475, 0.000000000000000000, 165.0000000000000000 ) ) ;
#40392 = EDGE_LOOP ( 'NONE', ( #29049, #33017, #37441, #21599, #30221, #24079 ) ) ;
#40393 = CARTESIAN_POINT ( 'NONE',  ( -10.49999999999999467, -46.01315789473684248, 5.916985404131813731 ) ) ;
#40394 = EDGE_CURVE ( 'NONE', #20584, #17646, #21866, .T. ) ;
#40395 = CARTESIAN_POINT ( 'NONE',  ( 193.3040265531851105, 1.750000000000009992, 0.8182875569279768335 ) ) ;
#40396 = ORIENTED_EDGE ( 'NONE', *, *, #18689, .F. ) ;
#40397 = VERTEX_POINT ( 'NONE', #37530 ) ;
#40398 = CARTESIAN_POINT ( 'NONE',  ( 2.961022939495062900, -16.59676755884084187, 2.590526750877053086 ) ) ;
#40399 = DIRECTION ( 'NONE',  ( 0.000000000000000000, 1.000000000000000000, 0.000000000000000000 ) ) ;
#40400 = CARTESIAN_POINT ( 'NONE',  ( -45.64490844644706868, -21.32281559348764333, 8.807470649214879543 ) ) ;
#40401 = FACE_OUTER_BOUND ( 'NONE', #34916, .T. ) ;
#40402 = ORIENTED_EDGE ( 'NONE', *, *, #31852, .T. ) ;
#40403 = VERTEX_POINT ( 'NONE', #10805 ) ;
#40404 = CARTESIAN_POINT ( 'NONE',  ( -225.0000000000000568, -175.0000000000000000, 500.0000000000000000 ) ) ;
#40405 = CARTESIAN_POINT ( 'NONE',  ( 13.35436367797824353, 31.26996044524050333, 7.906207997025717304 ) ) ;
#40406 = VERTEX_POINT ( 'NONE', #37779 ) ;
#40407 = VERTEX_POINT ( 'NONE', #6963 ) ;
#40408 = CYLINDRICAL_SURFACE ( 'NONE', #45201, 1.749999999999973799 ) ;
#40409 = CARTESIAN_POINT ( 'NONE',  ( 8.032723559237163968, -41.13077784380362090, 7.544061037322996377 ) ) ;
#40410 = CARTESIAN_POINT ( 'NONE',  ( 193.3040265531851105, -1.750000000000010658, -79.18171244307201562 ) ) ;
#40411 = CARTESIAN_POINT ( 'NONE',  ( 71.55402655318505367, 0.000000000000000000, 119.0682875569279560 ) ) ;
#40412 = ORIENTED_EDGE ( 'NONE', *, *, #47660, .T. ) ;
#40413 = VERTEX_POINT ( 'NONE', #14405 ) ;
#40414 = B_SPLINE_CURVE_WITH_KNOTS ( 'NONE', 3,
 ( #44622, #21302, #1562, #25924 ),
 .UNSPECIFIED., .F., .F.,
 ( 4, 4 ),
 ( 0.0006669682284780709776, 0.0007799402130919361490 ),
 .UNSPECIFIED. ) ;
#40415 = AXIS2_PLACEMENT_3D ( 'NONE', #15880, #47133, #12036 ) ;
#40416 = ORIENTED_EDGE ( 'NONE', *, *, #2916, .T. ) ;
#40418 = ADVANCED_FACE ( 'NONE', ( #17991 ), #41606, .T. ) ;
#40417 = PRESENTATION_LAYER_ASSIGNMENT (  '', '', ( #14986 ) ) ;
#40419 = CARTESIAN_POINT ( 'NONE',  ( 135.0000000000003411, 16.00000000000000000, -84.99999999999998579 ) ) ;
#40420 = CARTESIAN_POINT ( 'NONE',  ( 85.00000000000152056, 17.00000000000000000, 60.00000000000000000 ) ) ;
#40421 = EDGE_LOOP ( 'NONE', ( #22834, #48002, #3199 ) ) ;
#40422 = EDGE_LOOP ( 'NONE', ( #38260, #17784, #3938, #40151 ) ) ;
#40423 = CARTESIAN_POINT ( 'NONE',  ( 358.3431457505076310, 165.0000000000000000, -340.0000000000000568 ) ) ;
#40424 =( BOUNDED_CURVE ( )  B_SPLINE_CURVE ( 3, ( #5015, #48329, #36861, #20671 ),
 .UNSPECIFIED., .F., .F. ) 
 B_SPLINE_CURVE_WITH_KNOTS ( ( 4, 4 ),
 ( 4.712388980384689674, 6.283185307179586232 ),
 .UNSPECIFIED. ) 
 CURVE ( )  GEOMETRIC_REPRESENTATION_ITEM ( )  RATIONAL_B_SPLINE_CURVE ( ( 1.000000000000000000, 0.8047378541243649375, 0.8047378541243649375, 1.000000000000000000 ) ) 
 REPRESENTATION_ITEM ( '' )  );
#40425 = CARTESIAN_POINT ( 'NONE',  ( 115.0540265531850395, 2.143131898507847836E-16, 119.0682875569279844 ) ) ;
#40426 = VERTEX_POINT ( 'NONE', #30072 ) ;
#40427 = ORIENTED_EDGE ( 'NONE', *, *, #20011, .F. ) ;
#40428 = DIRECTION ( 'NONE',  ( 0.000000000000000000, 0.000000000000000000, -1.000000000000000000 ) ) ;
#40429 = CARTESIAN_POINT ( 'NONE',  ( -46.11867747200562206, 19.86470446310265459, -8.016098858316205167 ) ) ;
#40430 = ORIENTED_EDGE ( 'NONE', *, *, #26827, .F. ) ;
#40431 = CARTESIAN_POINT ( 'NONE',  ( -4.999999999999948486, -214.9999999999999716, -234.7500000000000000 ) ) ;
#40432 = DIRECTION ( 'NONE',  ( -0.000000000000000000, -0.000000000000000000, -1.000000000000000000 ) ) ;
#40433 = FACE_OUTER_BOUND ( 'NONE', #50637, .T. ) ;
#40434 = ADVANCED_FACE ( 'NONE', ( #45677 ), #44521, .T. ) ;
#40435 = EDGE_CURVE ( 'NONE', #15793, #30452, #38328, .T. ) ;
#40436 = EDGE_LOOP ( 'NONE', ( #21927, #2079, #46610, #2913, #39297, #9542, #8739, #48804 ) ) ;
#40437 = CARTESIAN_POINT ( 'NONE',  ( 181.0000000000000000, -272.5000000000000000, -98.99999999999990052 ) ) ;
#40438 = CARTESIAN_POINT ( 'NONE',  ( 34.08355720199905647, -2.371364769369109116, 7.455576670931136185 ) ) ;
#40439 = CARTESIAN_POINT ( 'NONE',  ( -25.63461350838931807, 43.17876197216396861, -8.016098858316199838 ) ) ;
#40440 = FACE_OUTER_BOUND ( 'NONE', #15342, .T. ) ;
#40441 = ADVANCED_FACE ( 'NONE', ( #39546 ), #7989, .T. ) ;
#40442 = EDGE_CURVE ( 'NONE', #22825, #43501, #35452, .T. ) ;
#40443 = VECTOR ( 'NONE', #46720, 1000.000000000000000 ) ;
#40444 = ADVANCED_FACE ( 'NONE', ( #23374 ), #34947, .F. ) ;
#40445 = CARTESIAN_POINT ( 'NONE',  ( 344.0000000000000000, -169.0000000000001137, -349.9999999999998863 ) ) ;
#40446 = CARTESIAN_POINT ( 'NONE',  ( -210.0000000000000568, 0.000000000000000000, 40.81828755692798438 ) ) ;
#40447 = CARTESIAN_POINT ( 'NONE',  ( 0.2827943264366570286, -6.852167361307233584, 9.753789706659947711 ) ) ;
#40448 = CARTESIAN_POINT ( 'NONE',  ( -44.94597344681493922, 2.143131898507880377E-16, 79.06828755692797017 ) ) ;
#40449 = MECHANICAL_DESIGN_GEOMETRIC_PRESENTATION_REPRESENTATION (  '', ( #32214 ), #4404 ) ;
#40450 = ORIENTED_EDGE ( 'NONE', *, *, #45303, .T. ) ;
#40451 = CARTESIAN_POINT ( 'NONE',  ( -13.35436367797847801, -31.26996044524040741, 7.906207997025717304 ) ) ;
#40452 = AXIS2_PLACEMENT_3D ( 'NONE', #10896, #19356, #35041 ) ;
#40453 = DIRECTION ( 'NONE',  ( 1.000000000000000000, 0.000000000000000000, -1.586032892321652482E-16 ) ) ;
#40454 = ORIENTED_EDGE ( 'NONE', *, *, #8276, .F. ) ;
#40455 = LINE ( 'NONE', #28897, #15559 ) ;
#40456 = DIRECTION ( 'NONE',  ( -1.000000000000000000, -0.000000000000000000, -0.000000000000000000 ) ) ;
#40457 = DIRECTION ( 'NONE',  ( -1.000000000000000000, -0.000000000000000000, -0.000000000000000000 ) ) ;
#40458 = EDGE_LOOP ( 'NONE', ( #83, #18631, #1088, #32987 ) ) ;
#40459 = DIRECTION ( 'NONE',  ( -1.000000000000000000, -0.000000000000000000, -0.000000000000000000 ) ) ;
#40460 = B_SPLINE_SURFACE_WITH_KNOTS ( 'NONE', 3, 3, ( 
 ( #6969, #30080, #19514, #15176 ),
 ( #3107, #26222, #10816, #38298 ),
 ( #41867, #23381, #22867, #50270 ),
 ( #7226, #7490, #39053, #18754 ) ),
 .UNSPECIFIED., .F., .F., .F.,
 ( 4, 4 ),
 ( 4, 4 ),
 ( 0.000000000000000000, 1.000000000000000000 ),
 ( 0.000000000000000000, 1.000000000000000000 ),
 .UNSPECIFIED. ) ;
#40461 = ORIENTED_EDGE ( 'NONE', *, *, #45961, .F. ) ;
#40462 = CARTESIAN_POINT ( 'NONE',  ( 357.1715728752537871, -183.0000000000001137, -358.0000000000003411 ) ) ;
#40463 = DIRECTION ( 'NONE',  ( -1.000000000000000000, 0.000000000000000000, 0.000000000000000000 ) ) ;
#40464 = CIRCLE ( 'NONE', #29796, 0.5000000000000004441 ) ;
#40465 = EDGE_LOOP ( 'NONE', ( #32784, #24199, #37072, #13496 ) ) ;
#40466 = DIRECTION ( 'NONE',  ( -0.000000000000000000, -0.000000000000000000, -1.000000000000000000 ) ) ;
#40467 = CARTESIAN_POINT ( 'NONE',  ( 166.9999999999999716, -268.4999999999999432, -349.9999999999999432 ) ) ;
#40468 = ORIENTED_EDGE ( 'NONE', *, *, #4965, .T. ) ;
#40469 = VERTEX_POINT ( 'NONE', #46431 ) ;
#40470 = CARTESIAN_POINT ( 'NONE',  ( 1.738880908827871830, 0.9455076376092198531, 9.897807938190494426 ) ) ;
#40471 = ORIENTED_EDGE ( 'NONE', *, *, #17706, .T. ) ;
#40472 = EDGE_CURVE ( 'NONE', #19269, #44210, #6536, .T. ) ;
#40473 = DIRECTION ( 'NONE',  ( 0.000000000000000000, 1.000000000000000000, 6.123233995736766036E-17 ) ) ;
#40474 = CARTESIAN_POINT ( 'NONE',  ( -50.64730461691362962, -42.31198943095992604, 742.8425600500171413 ) ) ;
#40475 = CARTESIAN_POINT ( 'NONE',  ( -12.78770032058971395, -31.68259716188267916, 7.455576670931136185 ) ) ;
#40476 = ORIENTED_EDGE ( 'NONE', *, *, #12928, .F. ) ;
#40477 = FACE_OUTER_BOUND ( 'NONE', #34392, .T. ) ;
#40478 = CARTESIAN_POINT ( 'NONE',  ( -69.99999999999879208, 17.00000000000000000, 5.000000000000004441 ) ) ;
#40479 = AXIS2_PLACEMENT_3D ( 'NONE', #25884, #46088, #42282 ) ;
#40480 = VERTEX_POINT ( 'NONE', #27980 ) ;
#40481 = EDGE_LOOP ( 'NONE', ( #2011, #28522, #21875, #9048 ) ) ;
#40482 = ORIENTED_EDGE ( 'NONE', *, *, #39671, .F. ) ;
#40483 = DIRECTION ( 'NONE',  ( -1.000000000000000000, -0.000000000000000000, -0.000000000000000000 ) ) ;
#40484 = VECTOR ( 'NONE', #42812, 1000.000000000000000 ) ;
#40485 = VERTEX_POINT ( 'NONE', #38786 ) ;
#40486 = VECTOR ( 'NONE', #40459, 1000.000000000000000 ) ;
#40487 = CARTESIAN_POINT ( 'NONE',  ( -88.44597344681497475, 0.000000000000000000, -120.9317124430720725 ) ) ;
#40488 = LINE ( 'NONE', #5324, #50117 ) ;
#40489 = VECTOR ( 'NONE', #24593, 1000.000000000000000 ) ;
#40490 = DIRECTION ( 'NONE',  ( -1.000000000000000000, 0.000000000000000000, 0.000000000000000000 ) ) ;
#40491 = FACE_BOUND ( 'NONE', #38972, .T. ) ;
#40492 = CARTESIAN_POINT ( 'NONE',  ( 210.0000000000000568, 2.143131898507876926E-16, -120.9317124430720582 ) ) ;
#40493 = FACE_OUTER_BOUND ( 'NONE', #24849, .T. ) ;
#40494 = FACE_OUTER_BOUND ( 'NONE', #25189, .T. ) ;
#40495 = CARTESIAN_POINT ( 'NONE',  ( 35.00000000000122213, 17.00000000000000000, 30.00000000000000000 ) ) ;
#40496 = CYLINDRICAL_SURFACE ( 'NONE', #36325, 1.750000000000008438 ) ;
#40497 = CARTESIAN_POINT ( 'NONE',  ( 48.98697415750968531, 11.03699497439252752, -8.016098858316199838 ) ) ;
#40498 = LINE ( 'NONE', #27684, #40489 ) ;
#40499 = AXIS2_PLACEMENT_3D ( 'NONE', #10324, #11270, #5954 ) ;
#40500 =( BOUNDED_CURVE ( )  B_SPLINE_CURVE ( 3, ( #42225, #19196, #19721, #38726 ),
 .UNSPECIFIED., .F., .F. ) 
 B_SPLINE_CURVE_WITH_KNOTS ( ( 4, 4 ),
 ( 0.000000000000000000, 1.570796326794896558 ),
 .UNSPECIFIED. ) 
 CURVE ( )  GEOMETRIC_REPRESENTATION_ITEM ( )  RATIONAL_B_SPLINE_CURVE ( ( 1.000000000000000000, 0.8047378541243649375, 0.8047378541243649375, 1.000000000000000000 ) ) 
 REPRESENTATION_ITEM ( '' )  );
#40501 = DIRECTION ( 'NONE',  ( -1.000000000000000000, 0.000000000000000000, 0.000000000000000000 ) ) ;
#40502 = VERTEX_POINT ( 'NONE', #35713 ) ;
#40503 = ADVANCED_FACE ( 'NONE', ( #38 ), #21197, .T. ) ;
#40504 = LINE ( 'NONE', #28198, #27830 ) ;
#40505 = CARTESIAN_POINT ( 'NONE',  ( -0.5109188679997889171, -1.175605252300625514, 9.967237415621765351 ) ) ;
#40506 = DIRECTION ( 'NONE',  ( 1.000000000000000000, 1.156482317317870492E-16, -0.000000000000000000 ) ) ;
#40507 = CARTESIAN_POINT ( 'NONE',  ( -165.0000000000000284, 16.00000000000000000, 115.0000000000000142 ) ) ;
#40508 = ORIENTED_EDGE ( 'NONE', *, *, #6454, .F. ) ;
#40509 = PLANE ( 'NONE',  #26487 ) ;
#40510 = CARTESIAN_POINT ( 'NONE',  ( -48.44597344681492501, 2.143131898507880377E-16, -160.9317124430720298 ) ) ;
#40511 = VECTOR ( 'NONE', #211, 1000.000000000000000 ) ;
#40512 = VERTEX_POINT ( 'NONE', #46683 ) ;
#40513 = CARTESIAN_POINT ( 'NONE',  ( 0.3370904143228959926, -0.2449105217885284291, -10.00000000000000000 ) ) ;
#40514 = VECTOR ( 'NONE', #327, 1000.000000000000000 ) ;
#40515 = CARTESIAN_POINT ( 'NONE',  ( 31.55402655318503236, 0.000000000000000000, -157.4317124430720014 ) ) ;
#40516 = CARTESIAN_POINT ( 'NONE',  ( 1.456734136748010888, -2.915208416223516785, 9.799352050262463365 ) ) ;
#40517 = VERTEX_POINT ( 'NONE', #11577 ) ;
#40518 = DIRECTION ( 'NONE',  ( 0.000000000000000000, 0.000000000000000000, -1.000000000000000000 ) ) ;
#40519 = ORIENTED_EDGE ( 'NONE', *, *, #43322, .F. ) ;
#40520 = VERTEX_POINT ( 'NONE', #39798 ) ;
#40521 = EDGE_LOOP ( 'NONE', ( #44618, #44848, #34212, #11780, #20639, #15051 ) ) ;
#40522 = CARTESIAN_POINT ( 'NONE',  ( 4.999999999999999112, 175.0000000000000284, 350.0000000000002274 ) ) ;
#40523 = CARTESIAN_POINT ( 'NONE',  ( -23.26005729352344176, -44.90397804740339183, 7.906207997025717304 ) ) ;
#40524 = ORIENTED_EDGE ( 'NONE', *, *, #38465, .T. ) ;
#40525 = DIRECTION ( 'NONE',  ( -2.775557561562891351E-16, -0.7071067811865474617, 0.7071067811865475727 ) ) ;
#40526 = CARTESIAN_POINT ( 'NONE',  ( 1.250000000000000222, 0.000000000000000000, 10.00000000000000000 ) ) ;
#40527 = DIRECTION ( 'NONE',  ( -0.000000000000000000, -0.000000000000000000, -1.000000000000000000 ) ) ;
#40528 = PLANE ( 'NONE',  #48849 ) ;
#40529 = ORIENTED_EDGE ( 'NONE', *, *, #47320, .T. ) ;
#40530 = PLANE ( 'NONE',  #24787 ) ;
#40531 = VECTOR ( 'NONE', #34249, 1000.000000000000000 ) ;
#40532 = ORIENTED_EDGE ( 'NONE', *, *, #39854, .F. ) ;
#40533 = CARTESIAN_POINT ( 'NONE',  ( 0.000000000000000000, 249.9999999999999716, 225.0000000000000000 ) ) ;
#40534 = LINE ( 'NONE', #41037, #22864 ) ;
#40535 = VERTEX_POINT ( 'NONE', #27231 ) ;
#40536 = AXIS2_PLACEMENT_3D ( 'NONE', #26804, #49589, #42689 ) ;
#40537 = ORIENTED_EDGE ( 'NONE', *, *, #12716, .T. ) ;
#40538 = ORIENTED_EDGE ( 'NONE', *, *, #4877, .T. ) ;
#40539 = CARTESIAN_POINT ( 'NONE',  ( -1.096405125442160067, -0.6872074048085232700, 9.947020512645400103 ) ) ;
#40540 = LINE ( 'NONE', #8985, #35703 ) ;
#40541 = EDGE_LOOP ( 'NONE', ( #15953, #48923, #10610, #6823, #39272, #24324 ) ) ;
#40542 = FACE_OUTER_BOUND ( 'NONE', #39984, .T. ) ;
#40543 = PRESENTATION_STYLE_ASSIGNMENT (( #10251 ) ) ;
#40544 = CARTESIAN_POINT ( 'NONE',  ( 8.831420117243668599, 14.12636088103192655, -3.546734833711462365 ) ) ;
#40545 = ORIENTED_EDGE ( 'NONE', *, *, #29517, .T. ) ;
#40546 = PLANE ( 'NONE',  #18755 ) ;
#40547 = DIRECTION ( 'NONE',  ( -1.000000000000000000, 0.000000000000000000, 0.000000000000000000 ) ) ;
#40548 = CARTESIAN_POINT ( 'NONE',  ( 343.9999999999998863, -165.0000000000001137, -90.00000000000018474 ) ) ;
#40549 = EDGE_LOOP ( 'NONE', ( #517, #11112, #26747, #26055 ) ) ;
#40550 = AXIS2_PLACEMENT_3D ( 'NONE', #32990, #33742, #29877 ) ;
#40551 = ORIENTED_EDGE ( 'NONE', *, *, #46595, .T. ) ;
#40552 = APPLICATION_PROTOCOL_DEFINITION ( 'draft international standard', 'automotive_design', 1998, #5289 ) ;
#40553 = CARTESIAN_POINT ( 'NONE',  ( 114.3291528190321173, -1.749999999999996669, 121.8434138227750481 ) ) ;
#40554 =( BOUNDED_CURVE ( )  B_SPLINE_CURVE ( 3, ( #10764, #49219, #14616, #37991 ),
 .UNSPECIFIED., .F., .F. ) 
 B_SPLINE_CURVE_WITH_KNOTS ( ( 4, 4 ),
 ( 4.712388980384689674, 6.283185307179586232 ),
 .UNSPECIFIED. ) 
 CURVE ( )  GEOMETRIC_REPRESENTATION_ITEM ( )  RATIONAL_B_SPLINE_CURVE ( ( 1.000000000000000000, 0.8047378541243649375, 0.8047378541243649375, 1.000000000000000000 ) ) 
 REPRESENTATION_ITEM ( '' )  );
#40555 = FACE_OUTER_BOUND ( 'NONE', #3774, .T. ) ;
#40556 = ADVANCED_FACE ( 'NONE', ( #23113 ), #42857, .T. ) ;
#40557 = LINE ( 'NONE', #33625, #1945 ) ;
#40558 = CARTESIAN_POINT ( 'NONE',  ( -15.45175104485246820, 6.222373774239106758, -2.870787844569587133 ) ) ;
#40559 = EDGE_LOOP ( 'NONE', ( #13809, #21035, #33243, #47103 ) ) ;
#40560 = LINE ( 'NONE', #10012, #41901 ) ;
#40561 = ADVANCED_FACE ( 'NONE', ( #292 ), #16188, .T. ) ;
#40562 =( BOUNDED_CURVE ( )  B_SPLINE_CURVE ( 3, ( #24680, #1075, #48225, #36492 ),
 .UNSPECIFIED., .F., .F. ) 
 B_SPLINE_CURVE_WITH_KNOTS ( ( 4, 4 ),
 ( 1.570796326794896558, 3.141592653589793116 ),
 .UNSPECIFIED. ) 
 CURVE ( )  GEOMETRIC_REPRESENTATION_ITEM ( )  RATIONAL_B_SPLINE_CURVE ( ( 1.000000000000000000, 0.8047378541243649375, 0.8047378541243649375, 1.000000000000000000 ) ) 
 REPRESENTATION_ITEM ( '' )  );
#40563 = CARTESIAN_POINT ( 'NONE',  ( -28.96803024440907137, -18.11533787072017176, 7.455576670931136185 ) ) ;
#40564 = PLANE ( 'NONE',  #404 ) ;
#40565 = EDGE_CURVE ( 'NONE', #12877, #35256, #31603, .T. ) ;
#40566 = CARTESIAN_POINT ( 'NONE',  ( -0.1425549192113998442, 1.238581250503548059, 9.981352469109934233 ) ) ;
#40567 = EDGE_CURVE ( 'NONE', #45555, #49766, #43363, .T. ) ;
#40568 = ORIENTED_EDGE ( 'NONE', *, *, #35942, .F. ) ;
#40569 = AXIS2_PLACEMENT_3D ( 'NONE', #27326, #31185, #11671 ) ;
#40570 = CARTESIAN_POINT ( 'NONE',  ( -70.00000000000002842, 16.00000000000000000, -114.9999999999999858 ) ) ;
#40571 = ORIENTED_EDGE ( 'NONE', *, *, #21838, .T. ) ;
#40572 = CARTESIAN_POINT ( 'NONE',  ( 6.174150299305392053, -50.00000000000000000, 8.807470649214879543 ) ) ;
#40573 = VECTOR ( 'NONE', #36297, 1000.000000000000000 ) ;
#40574 = ORIENTED_EDGE ( 'NONE', *, *, #33903, .F. ) ;
#40575 = DIRECTION ( 'NONE',  ( 0.000000000000000000, 0.000000000000000000, -1.000000000000000000 ) ) ;
#40576 = CARTESIAN_POINT ( 'NONE',  ( 210.0000000000000568, 0.000000000000000000, 160.8182875569279702 ) ) ;
#40577 = EDGE_CURVE ( 'NONE', #28214, #30532, #4870, .T. ) ;
#40578 = CARTESIAN_POINT ( 'NONE',  ( -86.69597344681494633, 1.750000000000010658, -79.18171244307201562 ) ) ;
#40579 = EDGE_LOOP ( 'NONE', ( #47370, #12919 ) ) ;
#40580 = VECTOR ( 'NONE', #34304, 1000.000000000000000 ) ;
#40581 = CARTESIAN_POINT ( 'NONE',  ( -64.99999999999971578, 17.00000000000000000, -60.00000000000000000 ) ) ;
#40582 = VERTEX_POINT ( 'NONE', #21040 ) ;
#40583 = CARTESIAN_POINT ( 'NONE',  ( 85.00000000000213163, 16.00000000000000000, 95.00000000000000000 ) ) ;
#40584 = CARTESIAN_POINT ( 'NONE',  ( 0.7606162131530698201, -1.296876929034913140, 9.953784399990620813 ) ) ;
#40585 = CARTESIAN_POINT ( 'NONE',  ( 33.64889274059390090, -3.704246042440748621, 8.356839323120299312 ) ) ;
#40586 = DIRECTION ( 'NONE',  ( -3.172065745548403743E-16, -1.000000000000000000, 0.000000000000000000 ) ) ;
#40587 = CARTESIAN_POINT ( 'NONE',  ( 28.96803024440893992, 18.11533787072037072, 7.455576670931136185 ) ) ;
#40588 = ORIENTED_EDGE ( 'NONE', *, *, #44865, .F. ) ;
#40590 = ORIENTED_EDGE ( 'NONE', *, *, #23345, .F. ) ;
#40589 = EDGE_CURVE ( 'NONE', #40610, #17293, #50688, .T. ) ;
#40591 = CARTESIAN_POINT ( 'NONE',  ( 130.0000000000002842, 17.00000000000000000, -60.00000000000000000 ) ) ;
#40592 = EDGE_CURVE ( 'NONE', #23977, #3156, #41046, .T. ) ;
#40593 = CIRCLE ( 'NONE', #18448, 2.000000000000001776 ) ;
#40594 = ADVANCED_FACE ( 'NONE', ( #32090 ), #36975, .T. ) ;
#40595 = EDGE_CURVE ( 'NONE', #33462, #10853, #11843, .T. ) ;
#40596 = VERTEX_POINT ( 'NONE', #1548 ) ;
#40597 = DIRECTION ( 'NONE',  ( 0.000000000000000000, 0.000000000000000000, 1.000000000000000000 ) ) ;
#40598 = FACE_OUTER_BOUND ( 'NONE', #42223, .T. ) ;
#40599 = EDGE_LOOP ( 'NONE', ( #7264, #27978, #42441, #6334 ) ) ;
#40600 = CARTESIAN_POINT ( 'NONE',  ( -128.4459734468149179, 0.000000000000000000, 162.5682875569279702 ) ) ;
#40601 = ADVANCED_FACE ( 'NONE', ( #5127 ), #38047, .T. ) ;
#40602 = EDGE_CURVE ( 'NONE', #43849, #9188, #9235, .T. ) ;
#40603 = FACE_OUTER_BOUND ( 'NONE', #23164, .T. ) ;
#40604 = VERTEX_POINT ( 'NONE', #16677 ) ;
#40605 = PLANE ( 'NONE',  #25925 ) ;
#40606 = CARTESIAN_POINT ( 'NONE',  ( -5.000000000000000000, 184.8000000000000114, -359.8000000000002387 ) ) ;
#40607 = CYLINDRICAL_SURFACE ( 'NONE', #8369, 1.749999999999987566 ) ;
#40608 = VECTOR ( 'NONE', #23668, 1000.000000000000000 ) ;
#40609 = ORIENTED_EDGE ( 'NONE', *, *, #14833, .F. ) ;
#40610 = VERTEX_POINT ( 'NONE', #47942 ) ;
#40611 = VERTEX_POINT ( 'NONE', #25395 ) ;
#40612 = VECTOR ( 'NONE', #8712, 1000.000000000000000 ) ;
#40613 = DIRECTION ( 'NONE',  ( -1.000000000000000000, 0.000000000000000000, 0.000000000000000000 ) ) ;
#40614 = FACE_OUTER_BOUND ( 'NONE', #5359, .T. ) ;
#40615 = FACE_OUTER_BOUND ( 'NONE', #5938, .T. ) ;
#40616 = VECTOR ( 'NONE', #30087, 1000.000000000000114 ) ;
#40617 = CARTESIAN_POINT ( 'NONE',  ( 73.30402655318508209, 1.750000000000010658, -79.18171244307201562 ) ) ;
#40618 = ORIENTED_EDGE ( 'NONE', *, *, #18686, .F. ) ;
#40619 = EDGE_CURVE ( 'NONE', #31669, #614, #21535, .T. ) ;
#40620 = CARTESIAN_POINT ( 'NONE',  ( -126.6959734468149321, -1.749999999999996891, 0.8182875569279768335 ) ) ;
#40621 = ORIENTED_EDGE ( 'NONE', *, *, #22812, .F. ) ;
#40622 = DIRECTION ( 'NONE',  ( 0.000000000000000000, 0.000000000000000000, -1.000000000000000000 ) ) ;
#40623 = PRESENTATION_LAYER_ASSIGNMENT (  '', '', ( #29995 ) ) ;
#40624 = DIRECTION ( 'NONE',  ( 0.000000000000000000, 0.000000000000000000, 1.000000000000000000 ) ) ;
#40625 = LINE ( 'NONE', #5461, #41412 ) ;
#40626 = ADVANCED_FACE ( 'NONE', ( #28745 ), #28491, .F. ) ;
#40627 = ADVANCED_FACE ( 'NONE', ( #40542 ), #21287, .F. ) ;
#40628 = LINE ( 'NONE', #43695, #47038 ) ;
#40629 = AXIS2_PLACEMENT_3D ( 'NONE', #2286, #38228, #34612 ) ;
#40630 = CARTESIAN_POINT ( 'NONE',  ( -64.99999999999877787, 17.00000000000000000, 30.00000000000000000 ) ) ;
#40631 = ORIENTED_EDGE ( 'NONE', *, *, #23096, .T. ) ;
#40632 = DIRECTION ( 'NONE',  ( 0.000000000000000000, -1.000000000000000000, 0.000000000000000000 ) ) ;
#40633 = DIRECTION ( 'NONE',  ( 1.000000000000000000, 0.000000000000000000, 0.000000000000000000 ) ) ;
#40634 = FACE_OUTER_BOUND ( 'NONE', #8473, .T. ) ;
#40635 = VECTOR ( 'NONE', #38670, 1000.000000000000000 ) ;
#40636 = EDGE_CURVE ( 'NONE', #48865, #38333, #48186, .T. ) ;
#40637 = CARTESIAN_POINT ( 'NONE',  ( -0.6667118921986187052, 1.119934874655410972, 9.961915419665738014 ) ) ;
#40638 = ORIENTED_EDGE ( 'NONE', *, *, #30354, .T. ) ;
#40639 = DIRECTION ( 'NONE',  ( 1.000000000000000000, 0.000000000000000000, 0.000000000000000000 ) ) ;
#40640 = ORIENTED_EDGE ( 'NONE', *, *, #49886, .T. ) ;
#40641 = LINE ( 'NONE', #44707, #831 ) ;
#40642 = CARTESIAN_POINT ( 'NONE',  ( 165.0000000000000000, -174.9999999999999716, -99.00000000000014211 ) ) ;
#40643 = CARTESIAN_POINT ( 'NONE',  ( 9.999999999999994671, -37.59858392880989442, -7.836098764781824322 ) ) ;
#40644 = EDGE_CURVE ( 'NONE', #7897, #50205, #26200, .T. ) ;
#40645 = ORIENTED_EDGE ( 'NONE', *, *, #18331, .T. ) ;
#40646 = VECTOR ( 'NONE', #19492, 1000.000000000000000 ) ;
#40647 = CARTESIAN_POINT ( 'NONE',  ( 23.26005729352310425, 44.90397804740356236, 7.906207997025717304 ) ) ;
#40648 = CARTESIAN_POINT ( 'NONE',  ( -126.6959734468149321, 1.749999999999996891, 160.8182875569279702 ) ) ;
#40649 = EDGE_CURVE ( 'NONE', #17911, #11545, #23283, .T. ) ;
#40650 = CIRCLE ( 'NONE', #3757, 4.000000000000003553 ) ;
#40651 = CARTESIAN_POINT ( 'NONE',  ( 185.0000000000000568, 165.0000000000000000, 355.9999999999998863 ) ) ;
#40652 = LINE ( 'NONE', #33712, #38166 ) ;
#40653 = ORIENTED_EDGE ( 'NONE', *, *, #536, .F. ) ;
#40654 = ORIENTED_EDGE ( 'NONE', *, *, #35889, .T. ) ;
#40655 = CARTESIAN_POINT ( 'NONE',  ( -5.542614707656985829, -8.340505786370593810, 6.429802539306485265 ) ) ;
#40656 = DIRECTION ( 'NONE',  ( 0.000000000000000000, -1.000000000000000000, 2.537652627714643577E-15 ) ) ;
#40657 = CIRCLE ( 'NONE', #16927, 1.750000000000036193 ) ;
#40658 = EDGE_CURVE ( 'NONE', #40007, #41009, #16726, .T. ) ;
#40659 = EDGE_CURVE ( 'NONE', #34244, #38646, #29747, .T. ) ;
#40660 = ORIENTED_EDGE ( 'NONE', *, *, #49340, .T. ) ;
#40661 = EDGE_LOOP ( 'NONE', ( #36019, #5489, #1887, #48299 ) ) ;
#40662 = CARTESIAN_POINT ( 'NONE',  ( -48.44597344681496054, 1.025126265847089213, -37.43171244307202272 ) ) ;
#40663 = DIRECTION ( 'NONE',  ( 1.000000000000000000, 0.000000000000000000, 0.000000000000000000 ) ) ;
#40664 = CARTESIAN_POINT ( 'NONE',  ( -48.44597344681496054, 1.025126265847089657, -120.9317124430720440 ) ) ;
#40665 = CARTESIAN_POINT ( 'NONE',  ( 32.27890028733795447, 1.750000000000009548, 159.7931612910809065 ) ) ;
#40666 = AXIS2_PLACEMENT_3D ( 'NONE', #25716, #1616, #1866 ) ;
#40667 = ORIENTED_EDGE ( 'NONE', *, *, #31937, .T. ) ;
#40668 = ORIENTED_EDGE ( 'NONE', *, *, #41853, .F. ) ;
#40669 = EDGE_LOOP ( 'NONE', ( #21211, #12990, #25389, #38853, #34373, #32686 ) ) ;
#40670 = ADVANCED_FACE ( 'NONE', ( #18184 ), #41547, .T. ) ;
#40671 = EDGE_CURVE ( 'NONE', #22825, #41411, #38232, .T. ) ;
#40672 = DIRECTION ( 'NONE',  ( 0.000000000000000000, 0.000000000000000000, 1.000000000000000000 ) ) ;
#40673 = CARTESIAN_POINT ( 'NONE',  ( 195.0540265531851105, 2.143131898507880377E-16, 119.0682875569279702 ) ) ;
#40674 = ORIENTED_EDGE ( 'NONE', *, *, #13918, .F. ) ;
#40675 = VERTEX_POINT ( 'NONE', #48936 ) ;
#40676 = DIRECTION ( 'NONE',  ( 0.000000000000000000, 0.000000000000000000, -1.000000000000000000 ) ) ;
#40677 = LINE ( 'NONE', #1429, #34726 ) ;
#40678 = ORIENTED_EDGE ( 'NONE', *, *, #14838, .T. ) ;
#40679 = EDGE_LOOP ( 'NONE', ( #37605, #41466, #14074, #3682, #44642, #10790 ) ) ;
#40680 = CARTESIAN_POINT ( 'NONE',  ( 49.46074318306830975, -9.578883844006833570, 8.807470649214879543 ) ) ;
#40681 = LINE ( 'NONE', #17571, #6732 ) ;
#40682 = ORIENTED_EDGE ( 'NONE', *, *, #39641, .F. ) ;
#40683 = LINE ( 'NONE', #31794, #37350 ) ;
#40684 = FACE_OUTER_BOUND ( 'NONE', #1591, .T. ) ;
#40685 = FACE_OUTER_BOUND ( 'NONE', #42379, .T. ) ;
#40686 = DIRECTION ( 'NONE',  ( -0.000000000000000000, 0.9749645535258953943, 0.2223603367690637489 ) ) ;
#40687 = VECTOR ( 'NONE', #34940, 1000.000000000000000 ) ;
#40688 = EDGE_CURVE ( 'NONE', #28309, #5743, #3039, .T. ) ;
#40689 = LINE ( 'NONE', #40931, #44554 ) ;
#40690 = VECTOR ( 'NONE', #12384, 1000.000000000000000 ) ;
#40691 = EDGE_LOOP ( 'NONE', ( #1404, #13964, #2357, #6320 ) ) ;
#40692 = DIRECTION ( 'NONE',  ( 0.000000000000000000, 0.000000000000000000, 1.000000000000000000 ) ) ;
#40693 = CARTESIAN_POINT ( 'NONE',  ( 16.16402646813543242, -4.033894069732437693, -3.546734833711462365 ) ) ;
#40694 = CARTESIAN_POINT ( 'NONE',  ( 359.9999999999999432, -181.0000000000001137, -356.0000000000003411 ) ) ;
#40695 = CARTESIAN_POINT ( 'NONE',  ( 37.50000000000000000, 4.592425496802574367E-15, 10.00000000000000000 ) ) ;
#40696 = VECTOR ( 'NONE', #47679, 1000.000000000000000 ) ;
#40697 = PLANE ( 'NONE',  #32217 ) ;
#40698 = AXIS2_PLACEMENT_3D ( 'NONE', #16377, #43313, #35147 ) ;
#40699 = CARTESIAN_POINT ( 'NONE',  ( 360.0000000000000000, -174.9999999999999147, 343.9999999999998295 ) ) ;
#40700 = CARTESIAN_POINT ( 'NONE',  ( -127.7210997126620242, 1.749999999999997113, 79.79316129108087807 ) ) ;
#40701 = CARTESIAN_POINT ( 'NONE',  ( 0.9390173899407876501, 1.130417317737878458, 9.958264684458711713 ) ) ;
#40702 = VECTOR ( 'NONE', #11498, 1000.000000000000000 ) ;
#40703 = ORIENTED_EDGE ( 'NONE', *, *, #42406, .F. ) ;
#40704 = CARTESIAN_POINT ( 'NONE',  ( 115.0540265531850395, 2.143131898507847836E-16, -160.9317124430720014 ) ) ;
#40705 = CARTESIAN_POINT ( 'NONE',  ( -16.15814872688569181, -4.048305257546697788, -2.870787844569587133 ) ) ;
#40706 = DIRECTION ( 'NONE',  ( -1.000000000000000000, -0.000000000000000000, -0.000000000000000000 ) ) ;
#40707 = CARTESIAN_POINT ( 'NONE',  ( -126.6959734468149321, 1.749999999999997113, -39.18171244307202983 ) ) ;
#40708 = DIRECTION ( 'NONE',  ( -1.000000000000000000, 0.000000000000000000, 0.000000000000000000 ) ) ;
#40709 = EDGE_LOOP ( 'NONE', ( #40348, #10370, #14880, #49203 ) ) ;
#40710 = DIRECTION ( 'NONE',  ( 0.000000000000000000, 0.000000000000000000, 1.000000000000000000 ) ) ;
#40711 = EDGE_LOOP ( 'NONE', ( #29726, #44093, #25016, #17464, #29471, #33232 ) ) ;
#40712 = CARTESIAN_POINT ( 'NONE',  ( -49.67735855322972327, 8.912210285362091255, 8.356839323120299312 ) ) ;
#40713 = LINE ( 'NONE', #31765, #41832 ) ;
#40714 = EDGE_CURVE ( 'NONE', #10095, #5769, #15077, .T. ) ;
#40715 = EDGE_CURVE ( 'NONE', #26837, #21965, #14852, .T. ) ;
#40716 = VECTOR ( 'NONE', #42533, 1000.000000000000000 ) ;
#40717 = VERTEX_POINT ( 'NONE', #29495 ) ;
#40718 = DIRECTION ( 'NONE',  ( -1.000000000000000000, 0.000000000000000000, 0.000000000000000000 ) ) ;
#40719 = CARTESIAN_POINT ( 'NONE',  ( -168.4459734468149463, 0.000000000000000000, -77.43171244307204404 ) ) ;
#40720 = VERTEX_POINT ( 'NONE', #42046 ) ;
#40721 = EDGE_LOOP ( 'NONE', ( #20073, #45178, #47627, #44224 ) ) ;
#40722 =( BOUNDED_CURVE ( )  B_SPLINE_CURVE ( 3, ( #28540, #40346, #31393, #27542 ),
 .UNSPECIFIED., .F., .F. ) 
 B_SPLINE_CURVE_WITH_KNOTS ( ( 4, 4 ),
 ( 0.000000000000000000, 1.570796326794896558 ),
 .UNSPECIFIED. ) 
 CURVE ( )  GEOMETRIC_REPRESENTATION_ITEM ( )  RATIONAL_B_SPLINE_CURVE ( ( 1.000000000000000000, 0.8047378541243649375, 0.8047378541243649375, 1.000000000000000000 ) ) 
 REPRESENTATION_ITEM ( '' )  );
#40723 = ADVANCED_FACE ( 'NONE', ( #14339 ), #7159, .T. ) ;
#40725 = EDGE_CURVE ( 'NONE', #19163, #34763, #21710, .T. ) ;
#40724 = FACE_OUTER_BOUND ( 'NONE', #46950, .T. ) ;
#40726 = ADVANCED_FACE ( 'NONE', ( #49199 ), #18437, .T. ) ;
#40727 = CYLINDRICAL_SURFACE ( 'NONE', #6266, 1.750000000000015543 ) ;
#40728 = VERTEX_POINT ( 'NONE', #10250 ) ;
#40729 = DIRECTION ( 'NONE',  ( 0.000000000000000000, 0.000000000000000000, 1.000000000000000000 ) ) ;
#40730 = CARTESIAN_POINT ( 'NONE',  ( -84.94597344681493212, 1.025126265847089435, 2.568287556927986159 ) ) ;
#40731 = EDGE_LOOP ( 'NONE', ( #28275, #23009, #44800, #42672, #14451, #33073 ) ) ;
#40732 = ORIENTED_EDGE ( 'NONE', *, *, #1831, .T. ) ;
#40733 = ORIENTED_EDGE ( 'NONE', *, *, #28674, .T. ) ;
#40734 = DIRECTION ( 'NONE',  ( 0.000000000000000000, -0.000000000000000000, 1.000000000000000000 ) ) ;
#40735 = EDGE_CURVE ( 'NONE', #50479, #44495, #18958, .T. ) ;
#40736 = CARTESIAN_POINT ( 'NONE',  ( 0.2778388845795309314, -1.251314014313100520, 9.976582533991681601 ) ) ;
#40737 = ORIENTED_EDGE ( 'NONE', *, *, #22880, .T. ) ;
#40738 = B_SPLINE_CURVE_WITH_KNOTS ( 'NONE', 3,
 ( #39241, #733, #4586, #34889 ),
 .UNSPECIFIED., .F., .F.,
 ( 4, 4 ),
 ( 0.000000000000000000, 0.002217981418809652702 ),
 .UNSPECIFIED. ) ;
#40739 = VECTOR ( 'NONE', #350, 1000.000000000000000 ) ;
#40740 = CARTESIAN_POINT ( 'NONE',  ( 151.5540265531850537, 0.000000000000000000, 42.56828755692798438 ) ) ;
#40741 = CARTESIAN_POINT ( 'NONE',  ( 73.30402655318508209, 1.750000000000009992, 160.8182875569279702 ) ) ;
#40742 = DIRECTION ( 'NONE',  ( 0.000000000000000000, 0.2791762785758810650, -0.9602398687205827565 ) ) ;
#40743 = DIRECTION ( 'NONE',  ( -3.172065784643302499E-16, -1.000000000000000000, 2.537652627714642000E-15 ) ) ;
#40744 = APPLICATION_CONTEXT ( 'automotive_design' ) ;
#40745 = DIRECTION ( 'NONE',  ( -0.000000000000000000, -0.000000000000000000, -1.000000000000000000 ) ) ;
#40746 = FACE_OUTER_BOUND ( 'NONE', #44088, .T. ) ;
#40747 = LINE ( 'NONE', #5334, #2872 ) ;
#40748 = FACE_OUTER_BOUND ( 'NONE', #46787, .T. ) ;
#40749 = FACE_OUTER_BOUND ( 'NONE', #21796, .T. ) ;
#40750 = PLANE ( 'NONE',  #20597 ) ;
#40751 = CIRCLE ( 'NONE', #49708, 33.33601305720110020 ) ;
#40752 = DIRECTION ( 'NONE',  ( -0.000000000000000000, -1.000000000000000000, -0.000000000000000000 ) ) ;
#40753 = ORIENTED_EDGE ( 'NONE', *, *, #873, .F. ) ;
#40754 = CARTESIAN_POINT ( 'NONE',  ( -175.0000000000000000, 15.00000000000000000, 122.5000000000000142 ) ) ;
#40755 = CARTESIAN_POINT ( 'NONE',  ( 168.9999999999999716, 8.000000000000062172, -350.0000000000001705 ) ) ;
#40756 = CARTESIAN_POINT ( 'NONE',  ( 5.551115123125782702E-14, -166.9999999999999432, 343.9999999999997726 ) ) ;
#40757 = CARTESIAN_POINT ( 'NONE',  ( -166.6959734468149463, -1.750000000000009992, 160.8182875569279702 ) ) ;
#40758 = EDGE_CURVE ( 'NONE', #9269, #31049, #13822, .T. ) ;
#40759 = VERTEX_POINT ( 'NONE', #10743 ) ;
#40760 = DIRECTION ( 'NONE',  ( -1.000000000000000000, -0.000000000000000000, -0.000000000000000000 ) ) ;
#40761 = DIRECTION ( 'NONE',  ( 0.000000000000000000, 0.000000000000000000, -1.000000000000000000 ) ) ;
#40762 = VERTEX_POINT ( 'NONE', #37714 ) ;
#40763 = CARTESIAN_POINT ( 'NONE',  ( -50.00000000000000000, -50.00000000000000000, 800.0000000000000000 ) ) ;
#40764 = CARTESIAN_POINT ( 'NONE',  ( 18.38319608353691947, -32.68498281710168385, -8.192531242611265085 ) ) ;
#40765 = CARTESIAN_POINT ( 'NONE',  ( 210.0000000000000568, 0.000000000000000000, 0.8182875569279768335 ) ) ;
#40766 = VERTEX_POINT ( 'NONE', #10497 ) ;
#40767 = CARTESIAN_POINT ( 'NONE',  ( -207.7210997126620384, -1.750000000000010214, 121.8434138227750623 ) ) ;
#40768 = B_SPLINE_SURFACE_WITH_KNOTS ( 'NONE', 3, 3, ( 
 ( #27372, #46061, #7885, #23530 ),
 ( #15328, #30980, #27120, #43005 ),
 ( #38425, #4020, #19667, #14544 ),
 ( #30199, #6857, #10955, #20170 ) ),
 .UNSPECIFIED., .F., .F., .F.,
 ( 4, 4 ),
 ( 4, 4 ),
 ( 0.000000000000000000, 1.000000000000000000 ),
 ( 0.000000000000000000, 1.000000000000000000 ),
 .UNSPECIFIED. ) ;
#40769 = ORIENTED_EDGE ( 'NONE', *, *, #5854, .F. ) ;
#40770 = ORIENTED_EDGE ( 'NONE', *, *, #33414, .T. ) ;
#40771 = ORIENTED_EDGE ( 'NONE', *, *, #11414, .F. ) ;
#40772 = CARTESIAN_POINT ( 'NONE',  ( 85.00000000000123634, 17.00000000000000000, 5.000000000000004441 ) ) ;
#40773 = CARTESIAN_POINT ( 'NONE',  ( -64.99999999999940314, 17.00000000000000000, -54.99999999999999289 ) ) ;
#40774 = ORIENTED_EDGE ( 'NONE', *, *, #29599, .T. ) ;
#40775 = CARTESIAN_POINT ( 'NONE',  ( 14.76429217231961566, 8.192625680377691566, 9.178419661560148768 ) ) ;
#40776 = PLANE ( 'NONE',  #8715 ) ;
#40777 = CARTESIAN_POINT ( 'NONE',  ( -0.9599924130074112272, 0.8495346730527952861, 9.948547179989619238 ) ) ;
#40778 = CARTESIAN_POINT ( 'NONE',  ( -167.7210997126620384, -1.750000000000009548, 159.7931612910809065 ) ) ;
#40779 = EDGE_LOOP ( 'NONE', ( #46102, #11795, #31961, #26898, #10472 ) ) ;
#40780 = DIRECTION ( 'NONE',  ( 1.000000000000000000, 0.000000000000000000, 0.000000000000000000 ) ) ;
#40781 = ORIENTED_EDGE ( 'NONE', *, *, #30292, .F. ) ;
#40782 = B_SPLINE_CURVE_WITH_KNOTS ( 'NONE', 3,
 ( #29730, #10724, #6374, #34102 ),
 .UNSPECIFIED., .F., .F.,
 ( 4, 4 ),
 ( 3.789440921763008408E-16, 0.009762429737398312102 ),
 .UNSPECIFIED. ) ;
#40783 = VECTOR ( 'NONE', #40432, 1000.000000000000000 ) ;
#40784 = CARTESIAN_POINT ( 'NONE',  ( 0.000000000000000000, -184.9999999999999716, -344.0000000000001705 ) ) ;
#40785 = CARTESIAN_POINT ( 'NONE',  ( 339.9999999999999432, 169.0000000000000000, -344.0000000000001137 ) ) ;
#40786 = ORIENTED_EDGE ( 'NONE', *, *, #2118, .T. ) ;
#40787 = VERTEX_POINT ( 'NONE', #21799 ) ;
#40788 = ORIENTED_EDGE ( 'NONE', *, *, #41286, .T. ) ;
#40789 = CARTESIAN_POINT ( 'NONE',  ( 195.9526953830863079, -154.8119894309599260, 472.8425600500171981 ) ) ;
#40790 = ADVANCED_FACE ( 'NONE', ( #6646 ), #37224, .T. ) ;
#40791 = PLANE ( 'NONE',  #39791 ) ;
#40792 = ORIENTED_EDGE ( 'NONE', *, *, #723, .F. ) ;
#40793 = CARTESIAN_POINT ( 'NONE',  ( -25.61277432017861955, 22.36370378792854297, 7.906207997025717304 ) ) ;
#40794 = CARTESIAN_POINT ( 'NONE',  ( 1.250000000000000222, 0.000000000000000000, 3.333333333333333481 ) ) ;
#40795 = CARTESIAN_POINT ( 'NONE',  ( 21.61731705588930907, 25.43568671410602278, -9.367992836599954742 ) ) ;
#40796 = ORIENTED_EDGE ( 'NONE', *, *, #37565, .T. ) ;
#40797 =( BOUNDED_CURVE ( )  B_SPLINE_CURVE ( 3, ( #50704, #47614, #15601, #7918 ),
 .UNSPECIFIED., .F., .F. ) 
 B_SPLINE_CURVE_WITH_KNOTS ( ( 4, 4 ),
 ( 0.000000000000000000, 1.570796326794896558 ),
 .UNSPECIFIED. ) 
 CURVE ( )  GEOMETRIC_REPRESENTATION_ITEM ( )  RATIONAL_B_SPLINE_CURVE ( ( 1.000000000000000000, 0.8047378541243649375, 0.8047378541243649375, 1.000000000000000000 ) ) 
 REPRESENTATION_ITEM ( '' )  );
#40798 = CARTESIAN_POINT ( 'NONE',  ( 344.0000000000000000, -174.9999999999999716, 343.9999999999998295 ) ) ;
#40799 = CARTESIAN_POINT ( 'NONE',  ( 151.5540265531850537, 0.000000000000000000, -80.93171244307201562 ) ) ;
#40800 = VECTOR ( 'NONE', #10124, 1000.000000000000000 ) ;
#40801 = DIRECTION ( 'NONE',  ( 0.000000000000000000, 0.000000000000000000, 1.000000000000000000 ) ) ;
#40802 = ORIENTED_EDGE ( 'NONE', *, *, #31550, .F. ) ;
#40803 = VERTEX_POINT ( 'NONE', #27670 ) ;
#40804 = APPLICATION_PROTOCOL_DEFINITION ( 'draft international standard', 'automotive_design', 1998, #49814 ) ;
#40805 = FACE_OUTER_BOUND ( 'NONE', #20814, .T. ) ;
#40806 = PLANE ( 'NONE',  #6180 ) ;
#40807 = CARTESIAN_POINT ( 'NONE',  ( 0.3862712429686894766, -1.188820645368940276, 10.00000000000000000 ) ) ;
#40808 = ORIENTED_EDGE ( 'NONE', *, *, #41387, .T. ) ;
#40809 = DIRECTION ( 'NONE',  ( 0.000000000000000000, 1.000000000000000000, 0.000000000000000000 ) ) ;
#40810 = DIRECTION ( 'NONE',  ( 0.000000000000000000, -1.000000000000000000, 0.000000000000000000 ) ) ;
#40811 = FACE_OUTER_BOUND ( 'NONE', #39031, .T. ) ;
#40812 = CARTESIAN_POINT ( 'NONE',  ( 0.000000000000000000, 175.0000000000000284, 350.0000000000002274 ) ) ;
#40813 = EDGE_CURVE ( 'NONE', #30497, #44652, #3541, .T. ) ;
#40814 = VERTEX_POINT ( 'NONE', #27170 ) ;
#40815 = CARTESIAN_POINT ( 'NONE',  ( -208.4459734468149463, 0.000000000000000000, -157.4317124430720582 ) ) ;
#40817 = ORIENTED_EDGE ( 'NONE', *, *, #48078, .F. ) ;
#40816 = AXIS2_PLACEMENT_3D ( 'NONE', #28687, #47638, #25343 ) ;
#40818 = DIRECTION ( 'NONE',  ( -4.758098676964957447E-16, -1.000000000000000000, 7.143884938411937192E-48 ) ) ;
#40819 = ORIENTED_EDGE ( 'NONE', *, *, #43264, .T. ) ;
#40820 = CARTESIAN_POINT ( 'NONE',  ( 191.5540265531851105, 0.000000000000000000, -37.43171244307205825 ) ) ;
#40821 = CARTESIAN_POINT ( 'NONE',  ( -208.4459734468149179, 2.143131898507880377E-16, -160.9317124430720298 ) ) ;
#40822 = DIRECTION ( 'NONE',  ( -0.4055129968046615185, 0.4055129968046615185, -0.8192181753629524943 ) ) ;
#40823 = ORIENTED_EDGE ( 'NONE', *, *, #36491, .T. ) ;
#40824 = CARTESIAN_POINT ( 'NONE',  ( -7.721099712662037540, 1.750000000000023315, -78.15658617722490931 ) ) ;
#40825 = ORIENTED_EDGE ( 'NONE', *, *, #37481, .F. ) ;
#40826 = DIRECTION ( 'NONE',  ( -0.000000000000000000, -0.000000000000000000, -1.000000000000000000 ) ) ;
#40827 = CARTESIAN_POINT ( 'NONE',  ( -126.6959734468149321, 1.749999999999997335, -119.1817124430720440 ) ) ;
#40828 = DIRECTION ( 'NONE',  ( -0.000000000000000000, -0.000000000000000000, -1.000000000000000000 ) ) ;
#40829 = LINE ( 'NONE', #2094, #49553 ) ;
#40830 = CARTESIAN_POINT ( 'NONE',  ( -0.3862712429686977478, 1.188820645368937390, 10.00000000000000000 ) ) ;
#40831 = VERTEX_POINT ( 'NONE', #18939 ) ;
#40832 = ORIENTED_EDGE ( 'NONE', *, *, #22858, .T. ) ;
#40833 = DIRECTION ( 'NONE',  ( 0.000000000000000000, 0.000000000000000000, -1.000000000000000000 ) ) ;
#40834 = VERTEX_POINT ( 'NONE', #42793 ) ;
#40835 = CARTESIAN_POINT ( 'NONE',  ( 181.0000000000001705, -184.9999999999999716, -115.0000000000001279 ) ) ;
#40836 = DIRECTION ( 'NONE',  ( -0.000000000000000000, 1.604368532695312981E-16, 1.000000000000000000 ) ) ;
#40837 = ORIENTED_EDGE ( 'NONE', *, *, #14215, .T. ) ;
#40838 = CARTESIAN_POINT ( 'NONE',  ( 7.500000000000000000, 224.9999999999999716, -240.0000000000000000 ) ) ;
#40839 = EDGE_CURVE ( 'NONE', #47564, #40762, #41301, .T. ) ;
#40840 = CARTESIAN_POINT ( 'NONE',  ( 152.2789002873379900, -1.750000000000010214, 79.79316129108087807 ) ) ;
#40841 = VERTEX_POINT ( 'NONE', #23569 ) ;
#40842 = CARTESIAN_POINT ( 'NONE',  ( 339.9999999999998863, -180.9999999999999716, 357.9999999999997726 ) ) ;
#40843 = CARTESIAN_POINT ( 'NONE',  ( -48.34672127938071640, 13.00749071703899773, 3.199614146704519602 ) ) ;
#40844 = DIRECTION ( 'NONE',  ( 1.000000000000000000, 0.000000000000000000, -0.000000000000000000 ) ) ;
#40845 =( BOUNDED_CURVE ( )  B_SPLINE_CURVE ( 3, ( #17421, #22279, #14064, #6125 ),
 .UNSPECIFIED., .F., .F. ) 
 B_SPLINE_CURVE_WITH_KNOTS ( ( 4, 4 ),
 ( 4.712388980384689674, 6.283185307179586232 ),
 .UNSPECIFIED. ) 
 CURVE ( )  GEOMETRIC_REPRESENTATION_ITEM ( )  RATIONAL_B_SPLINE_CURVE ( ( 1.000000000000000000, 0.8047378541243649375, 0.8047378541243649375, 1.000000000000000000 ) ) 
 REPRESENTATION_ITEM ( '' )  );
#40846 = CARTESIAN_POINT ( 'NONE',  ( -8.445973446814976526, 0.000000000000000000, 165.0000000000000000 ) ) ;
#40847 = ORIENTED_EDGE ( 'NONE', *, *, #21954, .F. ) ;
#40848 = CIRCLE ( 'NONE', #19521, 3.749999999999975575 ) ;
#40849 = ORIENTED_EDGE ( 'NONE', *, *, #18699, .T. ) ;
#40850 = ORIENTED_EDGE ( 'NONE', *, *, #7407, .T. ) ;
#40851 = DIRECTION ( 'NONE',  ( -3.172065784643302499E-16, -1.000000000000000000, 2.537652627714642000E-15 ) ) ;
#40852 = FACE_OUTER_BOUND ( 'NONE', #31619, .T. ) ;
#40853 = EDGE_CURVE ( 'NONE', #1381, #45083, #24399, .T. ) ;
#40854 =( BOUNDED_CURVE ( )  B_SPLINE_CURVE ( 3, ( #37571, #29848, #3391, #7255 ),
 .UNSPECIFIED., .F., .F. ) 
 B_SPLINE_CURVE_WITH_KNOTS ( ( 4, 4 ),
 ( 3.141592653589793116, 4.712388980384689674 ),
 .UNSPECIFIED. ) 
 CURVE ( )  GEOMETRIC_REPRESENTATION_ITEM ( )  RATIONAL_B_SPLINE_CURVE ( ( 1.000000000000000000, 0.8047378541243649375, 0.8047378541243649375, 1.000000000000000000 ) ) 
 REPRESENTATION_ITEM ( '' )  );
#40855 = CARTESIAN_POINT ( 'NONE',  ( 355.9999999999999432, -185.0000000000001421, -349.9999999999998863 ) ) ;
#40856 = EDGE_CURVE ( 'NONE', #20400, #40207, #42187, .T. ) ;
#40857 = CARTESIAN_POINT ( 'NONE',  ( -1.249999999999999778, 0.000000000000000000, -3.333333333333333481 ) ) ;
#40858 = ORIENTED_EDGE ( 'NONE', *, *, #1983, .F. ) ;
#40859 = DIRECTION ( 'NONE',  ( 0.000000000000000000, -1.000000000000000000, 1.604368532695312981E-16 ) ) ;
#40860 = ORIENTED_EDGE ( 'NONE', *, *, #21433, .F. ) ;
#40861 =( NAMED_UNIT ( * ) SI_UNIT ( $, .STERADIAN. ) SOLID_ANGLE_UNIT ( ) );
#40862 = EDGE_CURVE ( 'NONE', #11178, #2566, #15871, .T. ) ;
#40863 = CARTESIAN_POINT ( 'NONE',  ( 34.91952936320839740, -13.67027684621004546, -9.422646554964178023 ) ) ;
#40864 = LINE ( 'NONE', #32668, #34264 ) ;
#40865 = CARTESIAN_POINT ( 'NONE',  ( -4.945973446814903696, 2.143131898507912917E-16, 119.0682875569279418 ) ) ;
#40866 = DIRECTION ( 'NONE',  ( 0.000000000000000000, 0.000000000000000000, -1.000000000000000000 ) ) ;
#40867 = CARTESIAN_POINT ( 'NONE',  ( 85.00000000000184741, 16.00000000000000000, 65.00000000000000000 ) ) ;
#40868 = VERTEX_POINT ( 'NONE', #47124 ) ;
#40869 = B_SPLINE_SURFACE_WITH_KNOTS ( 'NONE', 3, 3, ( 
 ( #46537, #39152, #27336, #3980 ),
 ( #20136, #648, #16047, #22964 ),
 ( #148, #16297, #47042, #11945 ),
 ( #27603, #43232, #19113, #12191 ) ),
 .UNSPECIFIED., .F., .F., .F.,
 ( 4, 4 ),
 ( 4, 4 ),
 ( 0.000000000000000000, 1.000000000000000000 ),
 ( 0.000000000000000000, 1.000000000000000000 ),
 .UNSPECIFIED. ) ;
#40870 = DIRECTION ( 'NONE',  ( 0.000000000000000000, 0.000000000000000000, -1.000000000000000000 ) ) ;
#40871 = DIRECTION ( 'NONE',  ( 1.000000000000000000, 0.000000000000000000, 0.000000000000000000 ) ) ;
#40872 = EDGE_CURVE ( 'NONE', #37483, #40254, #11767, .T. ) ;
#40873 = EDGE_CURVE ( 'NONE', #20963, #29505, #46616, .T. ) ;
#40874 = EDGE_CURVE ( 'NONE', #34536, #46541, #13424, .T. ) ;
#40875 = EDGE_CURVE ( 'NONE', #19127, #31678, #35651, .T. ) ;
#40876 = CARTESIAN_POINT ( 'NONE',  ( -0.7606162131530730397, 1.296876929034918691, 9.953784399990622589 ) ) ;
#40877 = ORIENTED_EDGE ( 'NONE', *, *, #17496, .F. ) ;
#40878 = CARTESIAN_POINT ( 'NONE',  ( 31.55402655318503236, 0.000000000000000000, 165.0000000000000000 ) ) ;
#40879 = ORIENTED_EDGE ( 'NONE', *, *, #48957, .F. ) ;
#40880 = CARTESIAN_POINT ( 'NONE',  ( -44.94597344681493922, 2.143131898507880377E-16, 82.56828755692798438 ) ) ;
#40881 = CARTESIAN_POINT ( 'NONE',  ( 1.468624871022813139, 0.3222420739259631572, 9.936141075690079205 ) ) ;
#40882 = EDGE_CURVE ( 'NONE', #41724, #21938, #11514, .T. ) ;
#40883 = CARTESIAN_POINT ( 'NONE',  ( 8.640097307817493189, -14.29292567250784174, -9.458680755252684591 ) ) ;
#40884 = VECTOR ( 'NONE', #21673, 1000.000000000000000 ) ;
#40885 = ORIENTED_EDGE ( 'NONE', *, *, #7409, .F. ) ;
#40886 = VECTOR ( 'NONE', #5907, 1000.000000000000000 ) ;
#40887 = CARTESIAN_POINT ( 'NONE',  ( 46.11867747200574996, -19.86470446310233484, -8.016098858316205167 ) ) ;
#40888 = CARTESIAN_POINT ( 'NONE',  ( 33.89193117067290473, 0.000000000000000000, 910.0000000000000000 ) ) ;
#40890 = VECTOR ( 'NONE', #8566, 1000.000000000000000 ) ;
#40889 = CARTESIAN_POINT ( 'NONE',  ( -46.75893035013464072, -17.89420872045582200, 3.199614146704519602 ) ) ;
#40891 = VECTOR ( 'NONE', #24639, 1000.000000000000000 ) ;
#40892 = CARTESIAN_POINT ( 'NONE',  ( 33.86622497129647513, -3.037805405904928868, 7.906207997025717304 ) ) ;
#40893 = ORIENTED_EDGE ( 'NONE', *, *, #13266, .T. ) ;
#40894 = AXIS2_PLACEMENT_3D ( 'NONE', #23119, #27237, #36729 ) ;
#40895 = ORIENTED_EDGE ( 'NONE', *, *, #18294, .F. ) ;
#40896 = EDGE_CURVE ( 'NONE', #18198, #33857, #12267, .T. ) ;
#40897 = CARTESIAN_POINT ( 'NONE',  ( 151.5540265531850537, 0.000000000000000000, -117.4317124430720725 ) ) ;
#40898 = DIRECTION ( 'NONE',  ( -0.000000000000000000, -0.000000000000000000, -1.000000000000000000 ) ) ;
#40899 = TOROIDAL_SURFACE ( 'NONE', #31090, 27.58190990837850265, 8.000000000000000000 ) ;
#40900 = ADVANCED_FACE ( 'NONE', ( #23302 ), #2788, .T. ) ;
#40901 = ORIENTED_EDGE ( 'NONE', *, *, #12166, .T. ) ;
#40902 = EDGE_CURVE ( 'NONE', #41828, #6375, #50396, .T. ) ;
#40903 = ORIENTED_EDGE ( 'NONE', *, *, #46223, .F. ) ;
#40904 = FACE_OUTER_BOUND ( 'NONE', #10209, .T. ) ;
#40905 = FACE_OUTER_BOUND ( 'NONE', #20089, .T. ) ;
#40906 = CARTESIAN_POINT ( 'NONE',  ( 35.05402655318504657, 1.025126265847089435, 159.0682875569279418 ) ) ;
#40907 = PLANE ( 'NONE',  #5917 ) ;
#40908 = VERTEX_POINT ( 'NONE', #25090 ) ;
#40909 = ORIENTED_EDGE ( 'NONE', *, *, #3194, .F. ) ;
#40910 = EDGE_CURVE ( 'NONE', #5910, #26020, #13264, .T. ) ;
#40911 = ORIENTED_EDGE ( 'NONE', *, *, #10506, .F. ) ;
#40912 = EDGE_CURVE ( 'NONE', #7079, #7012, #24835, .T. ) ;
#40913 = FACE_OUTER_BOUND ( 'NONE', #23862, .T. ) ;
#40914 = DIRECTION ( 'NONE',  ( -1.000000000000000000, -0.000000000000000000, -0.000000000000000000 ) ) ;
#40915 = ORIENTED_EDGE ( 'NONE', *, *, #47606, .F. ) ;
#40916 = ORIENTED_EDGE ( 'NONE', *, *, #2008, .T. ) ;
#40917 = PLANE ( 'NONE',  #24323 ) ;
#40918 = CARTESIAN_POINT ( 'NONE',  ( 44.99506233596247995, 23.32283626942318833, 7.455576670931136185 ) ) ;
#40919 = EDGE_LOOP ( 'NONE', ( #25830, #47040, #34584, #28044 ) ) ;
#40920 = ORIENTED_EDGE ( 'NONE', *, *, #37510, .T. ) ;
#40921 = CARTESIAN_POINT ( 'NONE',  ( -124.9459734468149463, 2.143131898507847836E-16, 39.06828755692798438 ) ) ;
#40922 = DIRECTION ( 'NONE',  ( 0.000000000000000000, 0.000000000000000000, 1.000000000000000000 ) ) ;
#40924 = ORIENTED_EDGE ( 'NONE', *, *, #11709, .F. ) ;
#40923 = CIRCLE ( 'NONE', #29452, 4.000000000000003553 ) ;
#40925 = LINE ( 'NONE', #32993, #20104 ) ;
#40926 = CARTESIAN_POINT ( 'NONE',  ( -19.99999999999940670, 17.00000000000000000, -54.99999999999999289 ) ) ;
#40927 = CARTESIAN_POINT ( 'NONE',  ( -44.94597344681493922, 2.143131898507880377E-16, 165.0000000000000000 ) ) ;
#40928 = LINE ( 'NONE', #36608, #22013 ) ;
#40929 = VECTOR ( 'NONE', #19360, 1000.000000000000000 ) ;
#40930 = EDGE_CURVE ( 'NONE', #6064, #40611, #48147, .T. ) ;
#40931 = CARTESIAN_POINT ( 'NONE',  ( 168.9999999999999716, 8.000000000000062172, -340.0000000000001137 ) ) ;
#40932 = VERTEX_POINT ( 'NONE', #47881 ) ;
#40933 = AXIS2_PLACEMENT_3D ( 'NONE', #44050, #29183, #47874 ) ;
#40935 = AXIS2_PLACEMENT_3D ( 'NONE', #10271, #45129, #5653 ) ;
#40934 = CARTESIAN_POINT ( 'NONE',  ( 151.5540265531850537, 0.000000000000000000, -157.4317124430720582 ) ) ;
#40936 = CARTESIAN_POINT ( 'NONE',  ( 340.0000000000000568, 169.0000000000000000, 357.9999999999997726 ) ) ;
#40937 = CARTESIAN_POINT ( 'NONE',  ( 0.000000000000000000, -175.0000000000000284, -350.0000000000002274 ) ) ;
#40938 = CARTESIAN_POINT ( 'NONE',  ( 80.00000000000061107, 17.00000000000000000, -30.00000000000000000 ) ) ;
#40939 = EDGE_CURVE ( 'NONE', #26375, #48612, #46804, .T. ) ;
#40940 = ADVANCED_FACE ( 'NONE', ( #48127 ), #32038, .T. ) ;
#40941 = EDGE_CURVE ( 'NONE', #36323, #45661, #37724, .T. ) ;
#40942 = DIRECTION ( 'NONE',  ( -1.000000000000000000, 0.000000000000000000, 0.000000000000000000 ) ) ;
#40943 = CARTESIAN_POINT ( 'NONE',  ( -204.9459734468149463, 2.143131898507880377E-16, -117.4317124430720725 ) ) ;
#40944 = B_SPLINE_CURVE_WITH_KNOTS ( 'NONE', 3,
 ( #2870, #30101, #6994, #34983 ),
 .UNSPECIFIED., .F., .F.,
 ( 4, 4 ),
 ( 0.9890644561682331304, 1.000000000000000000 ),
 .UNSPECIFIED. ) ;
#40945 = EDGE_CURVE ( 'NONE', #1639, #28100, #4116, .T. ) ;
#40946 = CARTESIAN_POINT ( 'NONE',  ( -1.250000000000000222, 0.000000000000000000, 10.00000000000000000 ) ) ;
#40947 = CARTESIAN_POINT ( 'NONE',  ( 360.0000000000000568, 3.000000000000085709, 177.9999999999998295 ) ) ;
#40948 = EDGE_CURVE ( 'NONE', #7451, #37196, #36666, .T. ) ;
#40949 = FACE_OUTER_BOUND ( 'NONE', #12141, .T. ) ;
#40950 = ORIENTED_EDGE ( 'NONE', *, *, #32103, .F. ) ;
#40951 = CARTESIAN_POINT ( 'NONE',  ( -13.92102703536724384, -30.85732372859812500, 8.356839323120299312 ) ) ;
#40952 = DIRECTION ( 'NONE',  ( -0.1191452206184307888, 0.000000000000000000, 0.9928768384869220975 ) ) ;
#40953 = CARTESIAN_POINT ( 'NONE',  ( -206.6959734468149463, 0.000000000000000000, 165.0000000000000000 ) ) ;
#40954 = CARTESIAN_POINT ( 'NONE',  ( 48.33712804702525290, 13.03701565032775456, -9.367992836599951190 ) ) ;
#40955 = DIRECTION ( 'NONE',  ( -1.000000000000000000, 0.000000000000000000, -7.793956916774525800E-48 ) ) ;
#40956 = ORIENTED_EDGE ( 'NONE', *, *, #30323, .T. ) ;
#40957 = CARTESIAN_POINT ( 'NONE',  ( -1.578643388466005160, 1.550786058692512182, 9.881002359080275355 ) ) ;
#40958 = ORIENTED_EDGE ( 'NONE', *, *, #31005, .T. ) ;
#40959 = VECTOR ( 'NONE', #38514, 1000.000000000000000 ) ;
#40960 = LINE ( 'NONE', #33517, #43909 ) ;
#40961 = PLANE ( 'NONE',  #14801 ) ;
#40962 = AXIS2_PLACEMENT_3D ( 'NONE', #14813, #11232, #50158 ) ;
#40963 = CIRCLE ( 'NONE', #22134, 2.000000000000001776 ) ;
#40964 = VERTEX_POINT ( 'NONE', #16370 ) ;
#40965 = EDGE_CURVE ( 'NONE', #34447, #9708, #10223, .T. ) ;
#40966 = CARTESIAN_POINT ( 'NONE',  ( 4.763548243873389154, -16.57409059453848599, 8.727788335465566760 ) ) ;
#40967 = CARTESIAN_POINT ( 'NONE',  ( -0.7849184246622071814, 1.242376769534369041, 9.958264684458713489 ) ) ;
#40968 = EDGE_LOOP ( 'NONE', ( #15834, #19157, #21094, #23041 ) ) ;
#40969 = ORIENTED_EDGE ( 'NONE', *, *, #21484, .F. ) ;
#40970 = AXIS2_PLACEMENT_3D ( 'NONE', #45160, #10048, #33658 ) ;
#40971 = CARTESIAN_POINT ( 'NONE',  ( 164.9999999999999716, 16.00000000000000000, -90.00000000000000000 ) ) ;
#40972 = DIRECTION ( 'NONE',  ( 0.000000000000000000, 0.000000000000000000, -1.000000000000000000 ) ) ;
#40973 = CARTESIAN_POINT ( 'NONE',  ( 166.9999999999999716, -168.9999999999999147, -340.0000000000001137 ) ) ;
#40974 = VECTOR ( 'NONE', #13374, 1000.000000000000000 ) ;
#40975 = ORIENTED_EDGE ( 'NONE', *, *, #17673, .T. ) ;
#40976 = DIRECTION ( 'NONE',  ( 1.000000000000000000, 0.000000000000000000, -0.000000000000000000 ) ) ;
#40977 = DIRECTION ( 'NONE',  ( -1.000000000000000000, 0.000000000000000000, 0.000000000000000000 ) ) ;
#40978 = LINE ( 'NONE', #8916, #43369 ) ;
#40979 = ORIENTED_EDGE ( 'NONE', *, *, #17986, .T. ) ;
#40980 = ORIENTED_EDGE ( 'NONE', *, *, #11822, .T. ) ;
#40981 = ORIENTED_EDGE ( 'NONE', *, *, #28450, .T. ) ;
#40982 = DIRECTION ( 'NONE',  ( 0.000000000000000000, -1.000000000000000000, 0.000000000000000000 ) ) ;
#40983 = EDGE_CURVE ( 'NONE', #5197, #8231, #39991, .T. ) ;
#40984 = EDGE_LOOP ( 'NONE', ( #43157, #9865, #18404, #38695 ) ) ;
#40985 = CARTESIAN_POINT ( 'NONE',  ( -208.4459734468148611, -1.025126265847089879, -117.4317124430720156 ) ) ;
#40986 = DIRECTION ( 'NONE',  ( -0.4374820812098816347, -0.3178493372392748872, 0.8411784753765542133 ) ) ;
#40987 = LINE ( 'NONE', #13771, #6319 ) ;
#40988 = LINE ( 'NONE', #37163, #28803 ) ;
#40989 = CARTESIAN_POINT ( 'NONE',  ( -164.4973046169135955, -97.66198943095992036, -17.48025818148969890 ) ) ;
#40990 = LINE ( 'NONE', #16894, #18550 ) ;
#40991 = CARTESIAN_POINT ( 'NONE',  ( 31.55402655318503236, 0.000000000000000000, 42.56828755692798438 ) ) ;
#40992 = CARTESIAN_POINT ( 'NONE',  ( 210.0000000000000568, 0.000000000000000000, -119.1817124430720440 ) ) ;
#40993 = CARTESIAN_POINT ( 'NONE',  ( 183.0000000000000284, -168.9999999999999432, -115.0000000000001847 ) ) ;
#40994 = AXIS2_PLACEMENT_3D ( 'NONE', #20945, #47339, #12231 ) ;
#40995 = CARTESIAN_POINT ( 'NONE',  ( -13.59579750444763668, 10.60877755095910935, 8.727788335465566760 ) ) ;
#40996 =( BOUNDED_CURVE ( )  B_SPLINE_CURVE ( 3, ( #45820, #17404, #29457, #14043 ),
 .UNSPECIFIED., .F., .F. ) 
 B_SPLINE_CURVE_WITH_KNOTS ( ( 4, 4 ),
 ( 4.712388980384689674, 6.283185307179586232 ),
 .UNSPECIFIED. ) 
 CURVE ( )  GEOMETRIC_REPRESENTATION_ITEM ( )  RATIONAL_B_SPLINE_CURVE ( ( 1.000000000000000000, 0.8047378541243649375, 0.8047378541243649375, 1.000000000000000000 ) ) 
 REPRESENTATION_ITEM ( '' )  );
#40997 = ADVANCED_FACE ( 'NONE', ( #1244 ), #28183, .T. ) ;
#40998 = EDGE_CURVE ( 'NONE', #39878, #35427, #20463, .T. ) ;
#40999 = DIRECTION ( 'NONE',  ( 0.000000000000000000, 0.000000000000000000, 1.000000000000000000 ) ) ;
#41000 = ORIENTED_EDGE ( 'NONE', *, *, #42214, .F. ) ;
#41001 = VECTOR ( 'NONE', #2043, 1000.000000000000000 ) ;
#41002 = DIRECTION ( 'NONE',  ( 0.000000000000000000, -1.000000000000000000, 0.000000000000000000 ) ) ;
#41003 = EDGE_CURVE ( 'NONE', #44183, #38646, #985, .T. ) ;
#41004 = LINE ( 'NONE', #41752, #10278 ) ;
#41005 = VECTOR ( 'NONE', #20491, 1000.000000000000000 ) ;
#41006 = DIRECTION ( 'NONE',  ( 1.000000000000000000, 0.000000000000000000, 0.000000000000000000 ) ) ;
#41007 = ADVANCED_FACE ( 'NONE', ( #37160 ), #49879, .F. ) ;
#41008 = EDGE_CURVE ( 'NONE', #36841, #44023, #23922, .T. ) ;
#41009 = VERTEX_POINT ( 'NONE', #2729 ) ;
#41010 = DIRECTION ( 'NONE',  ( 0.000000000000000000, 0.000000000000000000, 1.000000000000000000 ) ) ;
#41011 = CARTESIAN_POINT ( 'NONE',  ( -22.82242230425432439, 2.683863964738837371, 226.0000000000000000 ) ) ;
#41012 = EDGE_LOOP ( 'NONE', ( #30549, #33398, #22337, #46724 ) ) ;
#41013 = FACE_OUTER_BOUND ( 'NONE', #7360, .T. ) ;
#41014 = CARTESIAN_POINT ( 'NONE',  ( 343.9999999999999432, 174.9999999999996589, -356.0000000000003411 ) ) ;
#41015 = LINE ( 'NONE', #25870, #2855 ) ;
#41016 = EDGE_CURVE ( 'NONE', #2518, #7079, #2623, .T. ) ;
#41017 =( BOUNDED_CURVE ( )  B_SPLINE_CURVE ( 3, ( #731, #16133, #27425, #31030 ),
 .UNSPECIFIED., .F., .F. ) 
 B_SPLINE_CURVE_WITH_KNOTS ( ( 4, 4 ),
 ( 0.000000000000000000, 1.570796326794896558 ),
 .UNSPECIFIED. ) 
 CURVE ( )  GEOMETRIC_REPRESENTATION_ITEM ( )  RATIONAL_B_SPLINE_CURVE ( ( 1.000000000000000000, 0.8047378541243649375, 0.8047378541243649375, 1.000000000000000000 ) ) 
 REPRESENTATION_ITEM ( '' )  );
#41018 = ORIENTED_EDGE ( 'NONE', *, *, #130, .T. ) ;
#41019 = DIRECTION ( 'NONE',  ( -1.000000000000000000, 0.000000000000000000, -0.000000000000000000 ) ) ;
#41020 = ORIENTED_EDGE ( 'NONE', *, *, #23279, .F. ) ;
#41021 = VERTEX_POINT ( 'NONE', #45301 ) ;
#41022 = DIRECTION ( 'NONE',  ( 1.000000000000000000, 0.000000000000000000, 0.000000000000000000 ) ) ;
#41023 = ORIENTED_EDGE ( 'NONE', *, *, #2486, .T. ) ;
#41024 = DIRECTION ( 'NONE',  ( -0.000000000000000000, -1.000000000000000000, -0.000000000000000000 ) ) ;
#41025 = DIRECTION ( 'NONE',  ( -1.000000000000000000, 0.000000000000000000, 0.000000000000000000 ) ) ;
#41026 = ORIENTED_EDGE ( 'NONE', *, *, #2626, .T. ) ;
#41027 = CARTESIAN_POINT ( 'NONE',  ( 20.21530556545302559, -31.58467066308217497, -9.422646554964174470 ) ) ;
#41028 = DIRECTION ( 'NONE',  ( 1.000000000000000000, 0.000000000000000000, -0.000000000000000000 ) ) ;
#41029 = LINE ( 'NONE', #17424, #28206 ) ;
#41030 = CARTESIAN_POINT ( 'NONE',  ( 339.9999999999999432, -180.9999999999999716, -342.0000000000001705 ) ) ;
#41031 = ORIENTED_EDGE ( 'NONE', *, *, #18623, .T. ) ;
#41032 = CARTESIAN_POINT ( 'NONE',  ( 432.7825420346616170, 74.83106485270648989, -130.5992382549688955 ) ) ;
#41033 = AXIS2_PLACEMENT_3D ( 'NONE', #31507, #39463, #19937 ) ;
#41034 = VECTOR ( 'NONE', #42574, 1000.000000000000000 ) ;
#41035 = ORIENTED_EDGE ( 'NONE', *, *, #23647, .F. ) ;
#41036 = FACE_OUTER_BOUND ( 'NONE', #35139, .T. ) ;
#41037 = CARTESIAN_POINT ( 'NONE',  ( -7.822422304254325276, -2.816136035261162185, 230.0000000000000000 ) ) ;
#41038 = ORIENTED_EDGE ( 'NONE', *, *, #9656, .T. ) ;
#41039 = ORIENTED_EDGE ( 'NONE', *, *, #595, .T. ) ;
#41040 = VERTEX_POINT ( 'NONE', #49389 ) ;
#41041 = CARTESIAN_POINT ( 'NONE',  ( 0.000000000000000000, 0.000000000000000000, 0.000000000000000000 ) ) ;
#41042 = DIRECTION ( 'NONE',  ( -1.000000000000000000, 0.000000000000000000, -1.612977847700450206E-50 ) ) ;
#41043 = AXIS2_PLACEMENT_3D ( 'NONE', #18332, #30150, #25546 ) ;
#41044 = VERTEX_POINT ( 'NONE', #9679 ) ;
#41045 = ADVANCED_FACE ( 'NONE', ( #29434 ), #18626, .T. ) ;
#41046 = LINE ( 'NONE', #44858, #38072 ) ;
#41047 = CARTESIAN_POINT ( 'NONE',  ( -6.174150299305392053, 33.14591993373988998, 8.807470649214879543 ) ) ;
#41048 = LINE ( 'NONE', #5888, #20657 ) ;
#41049 = CARTESIAN_POINT ( 'NONE',  ( -166.6959734468149463, 1.750000000000010214, -39.18171244307202983 ) ) ;
#41050 = ORIENTED_EDGE ( 'NONE', *, *, #4825, .T. ) ;
#41051 = DIRECTION ( 'NONE',  ( 0.7233555441435721711, 0.6904757466825005574, -0.000000000000000000 ) ) ;
#41052 = CARTESIAN_POINT ( 'NONE',  ( -0.9342132981372995859, -1.950058179216137999, 9.882710035074772748 ) ) ;
#41053 = CARTESIAN_POINT ( 'NONE',  ( -48.33712804702535948, -13.03701565032741527, -9.367992836599954742 ) ) ;
#41054 = ORIENTED_EDGE ( 'NONE', *, *, #11067, .T. ) ;
#41055 = CARTESIAN_POINT ( 'NONE',  ( 114.3291528190321173, 1.749999999999996891, -118.1565861772249661 ) ) ;
#41056 = FACE_OUTER_BOUND ( 'NONE', #6432, .T. ) ;
#41057 = EDGE_CURVE ( 'NONE', #45408, #47482, #18376, .T. ) ;
#41058 = EDGE_CURVE ( 'NONE', #45409, #6771, #27534, .T. ) ;
#41059 = CARTESIAN_POINT ( 'NONE',  ( 0.4401267517947335395, -2.015194695084121079, 9.889206917020302967 ) ) ;
#41060 = CARTESIAN_POINT ( 'NONE',  ( 80.00000000000217426, 17.00000000000000000, 115.0000000000000142 ) ) ;
#41061 = ORIENTED_EDGE ( 'NONE', *, *, #27587, .T. ) ;
#41062 = CARTESIAN_POINT ( 'NONE',  ( 166.9999999999999716, -174.9999999999999716, -344.0000000000001137 ) ) ;
#41063 = CARTESIAN_POINT ( 'NONE',  ( 210.0000000000000568, 0.000000000000000000, -119.1817124430720440 ) ) ;
#41064 = CARTESIAN_POINT ( 'NONE',  ( -4.339432828817248122, -37.24807810779213213, -8.192531242611266862 ) ) ;
#41065 = LINE ( 'NONE', #28516, #28743 ) ;
#41066 = AXIS2_PLACEMENT_3D ( 'NONE', #31028, #14598, #10747 ) ;
#41067 = EDGE_CURVE ( 'NONE', #36298, #44983, #21840, .T. ) ;
#41068 = EDGE_CURVE ( 'NONE', #25245, #30746, #32355, .T. ) ;
#41069 = EDGE_LOOP ( 'NONE', ( #37014, #48522, #21598, #19525 ) ) ;
#41070 = DIRECTION ( 'NONE',  ( -1.000000000000000000, -0.000000000000000000, -0.000000000000000000 ) ) ;
#41071 = ORIENTED_EDGE ( 'NONE', *, *, #48189, .T. ) ;
#41072 = CARTESIAN_POINT ( 'NONE',  ( -3.229232847726260403, 16.57333684275945629, 9.178419661560148768 ) ) ;
#41073 = ORIENTED_EDGE ( 'NONE', *, *, #13650, .F. ) ;
#41074 = EDGE_CURVE ( 'NONE', #8464, #7855, #6339, .T. ) ;
#41075 = CARTESIAN_POINT ( 'NONE',  ( 55.00000000000002132, -52.50000000000000711, 5.000000000000000000 ) ) ;
#41076 = VECTOR ( 'NONE', #25601, 1000.000000000000000 ) ;
#41077 = DIRECTION ( 'NONE',  ( -1.000000000000000000, 0.000000000000000000, 0.000000000000000000 ) ) ;
#41078 = VECTOR ( 'NONE', #10457, 1000.000000000000000 ) ;
#41079 =( NAMED_UNIT ( * ) SI_UNIT ( $, .STERADIAN. ) SOLID_ANGLE_UNIT ( ) );
#41081 = ORIENTED_EDGE ( 'NONE', *, *, #29564, .T. ) ;
#41080 = B_SPLINE_CURVE_WITH_KNOTS ( 'NONE', 3,
 ( #27575, #43210, #38874, #26548 ),
 .UNSPECIFIED., .F., .F.,
 ( 4, 4 ),
 ( 0.7491799374948676649, 1.000000000000000000 ),
 .UNSPECIFIED. ) ;
#41082 = CARTESIAN_POINT ( 'NONE',  ( -21.20039782019574659, 30.97601161206942066, -2.490396854064190979 ) ) ;
#41083 = ORIENTED_EDGE ( 'NONE', *, *, #25875, .T. ) ;
#41084 = CARTESIAN_POINT ( 'NONE',  ( -165.6708471809677974, 1.750000000000009548, 39.79316129108089228 ) ) ;
#41085 = CARTESIAN_POINT ( 'NONE',  ( 0.000000000000000000, -184.9999999999999716, -356.0000000000002274 ) ) ;
#41086 = LINE ( 'NONE', #21577, #5395 ) ;
#41087 = PLANE ( 'NONE',  #30417 ) ;
#41088 = ORIENTED_EDGE ( 'NONE', *, *, #44744, .T. ) ;
#41089 = ORIENTED_EDGE ( 'NONE', *, *, #14123, .T. ) ;
#41090 = DIRECTION ( 'NONE',  ( 0.000000000000000000, 0.000000000000000000, 1.000000000000000000 ) ) ;
#41091 = ORIENTED_EDGE ( 'NONE', *, *, #30649, .F. ) ;
#41092 = DIRECTION ( 'NONE',  ( 0.000000000000000000, 0.000000000000000000, 1.000000000000000000 ) ) ;
#41093 = DIRECTION ( 'NONE',  ( -1.586032880504786307E-16, 1.654361225106055350E-24, -1.000000000000000000 ) ) ;
#41094 =( BOUNDED_CURVE ( )  B_SPLINE_CURVE ( 3, ( #17049, #47803, #32705, #28351 ),
 .UNSPECIFIED., .F., .F. ) 
 B_SPLINE_CURVE_WITH_KNOTS ( ( 4, 4 ),
 ( 3.141592653589793116, 4.712388980384689674 ),
 .UNSPECIFIED. ) 
 CURVE ( )  GEOMETRIC_REPRESENTATION_ITEM ( )  RATIONAL_B_SPLINE_CURVE ( ( 1.000000000000000000, 0.8047378541243649375, 0.8047378541243649375, 1.000000000000000000 ) ) 
 REPRESENTATION_ITEM ( '' )  );
#41095 = VERTEX_POINT ( 'NONE', #21473 ) ;
#41096 = CARTESIAN_POINT ( 'NONE',  ( 10.06660411345801087, 8.486842105263159297, -18.70408263333243326 ) ) ;
#41097 = VECTOR ( 'NONE', #41564, 1000.000000000000000 ) ;
#41098 = CARTESIAN_POINT ( 'NONE',  ( 153.3040265531850537, -1.750000000000010658, 80.81828755692798438 ) ) ;
#41099 = ORIENTED_EDGE ( 'NONE', *, *, #1749, .F. ) ;
#41100 = LINE ( 'NONE', #40842, #7979 ) ;
#41101 = ADVANCED_FACE ( 'NONE', ( #2484 ), #10686, .F. ) ;
#41102 = DIRECTION ( 'NONE',  ( 0.000000000000000000, 0.000000000000000000, -1.000000000000000000 ) ) ;
#41103 = CYLINDRICAL_SURFACE ( 'NONE', #47834, 1.750000000000001554 ) ;
#41104 = CARTESIAN_POINT ( 'NONE',  ( 115.0540265531850395, -1.025126265847081886, 39.06828755692799149 ) ) ;
#41105 = ORIENTED_EDGE ( 'NONE', *, *, #35058, .T. ) ;
#41106 = ORIENTED_EDGE ( 'NONE', *, *, #21797, .T. ) ;
#41107 = ORIENTED_EDGE ( 'NONE', *, *, #46575, .T. ) ;
#41108 = CARTESIAN_POINT ( 'NONE',  ( -0.9602803029231570253, 0.8490247040095960651, 9.976582533991679824 ) ) ;
#41109 = CARTESIAN_POINT ( 'NONE',  ( 33.43156050989131955, -4.370686678976570150, 8.807470649214879543 ) ) ;
#41110 = CARTESIAN_POINT ( 'NONE',  ( -64.99999999999815259, 17.00000000000000000, 90.00000000000000000 ) ) ;
#41111 = CARTESIAN_POINT ( 'NONE',  ( 360.0000000000000000, -166.6568542494923406, 341.6568542494921417 ) ) ;
#41112 = ORIENTED_EDGE ( 'NONE', *, *, #21310, .F. ) ;
#41113 = CARTESIAN_POINT ( 'NONE',  ( 111.5540265531850679, 0.000000000000000000, 42.56828755692795596 ) ) ;
#41114 = ORIENTED_EDGE ( 'NONE', *, *, #21130, .T. ) ;
#41115 = DIRECTION ( 'NONE',  ( 1.000000000000000000, 0.000000000000000000, 0.000000000000000000 ) ) ;
#41116 = LINE ( 'NONE', #32939, #2315 ) ;
#41117 = CARTESIAN_POINT ( 'NONE',  ( 350.0000000000000000, 167.0000000000000000, -344.0000000000001705 ) ) ;
#41118 = CARTESIAN_POINT ( 'NONE',  ( 210.0000000000000568, 0.000000000000000000, -79.18171244307201562 ) ) ;
#41119 = PLANE ( 'NONE',  #15109 ) ;
#41120 = CARTESIAN_POINT ( 'NONE',  ( -126.6959734468149321, -1.749999999999996891, -159.1817124430720298 ) ) ;
#41121 = ORIENTED_EDGE ( 'NONE', *, *, #41265, .F. ) ;
#41122 = CARTESIAN_POINT ( 'NONE',  ( 0.000000000000000000, -168.9999999999999432, -358.0000000000002274 ) ) ;
#41123 = DIRECTION ( 'NONE',  ( -0.000000000000000000, -1.000000000000000000, -0.000000000000000000 ) ) ;
#41124 = CARTESIAN_POINT ( 'NONE',  ( -6.695973446814940111, 0.000000000000000000, 165.0000000000000000 ) ) ;
#41125 = FACE_OUTER_BOUND ( 'NONE', #673, .T. ) ;
#41126 = ORIENTED_EDGE ( 'NONE', *, *, #7416, .T. ) ;
#41127 = DIRECTION ( 'NONE',  ( -1.000000000000000000, 0.000000000000000000, 0.000000000000000000 ) ) ;
#41128 = ORIENTED_EDGE ( 'NONE', *, *, #15627, .F. ) ;
#41129 = EDGE_CURVE ( 'NONE', #23318, #35686, #45557, .T. ) ;
#41130 = DIRECTION ( 'NONE',  ( -1.000000000000000000, -0.000000000000000000, -0.000000000000000000 ) ) ;
#41131 = VECTOR ( 'NONE', #356, 1000.000000000000000 ) ;
#41132 = CARTESIAN_POINT ( 'NONE',  ( 0.3862712429686894766, -1.188820645368940276, 10.00000000000000000 ) ) ;
#41133 = DIRECTION ( 'NONE',  ( -1.000000000000000000, 0.000000000000000000, 0.000000000000000000 ) ) ;
#41134 = AXIS2_PLACEMENT_3D ( 'NONE', #21392, #1906, #7208 ) ;
#41135 = DIRECTION ( 'NONE',  ( -0.000000000000000000, -0.000000000000000000, -1.000000000000000000 ) ) ;
#41136 = CARTESIAN_POINT ( 'NONE',  ( 1.011271242968694084, -0.7347315653655782652, -10.00000000000000000 ) ) ;
#41137 = CARTESIAN_POINT ( 'NONE',  ( -164.9999999999981526, 17.00000000000000000, 65.00000000000000000 ) ) ;
#41138 = DIRECTION ( 'NONE',  ( -1.000000000000000000, 0.000000000000000000, 0.000000000000000000 ) ) ;
#41139 = ORIENTED_EDGE ( 'NONE', *, *, #26331, .T. ) ;
#41140 = EDGE_LOOP ( 'NONE', ( #25733, #47063, #43872, #9607 ) ) ;
#41141 = DIRECTION ( 'NONE',  ( -5.551115123125781470E-17, 0.7071067811865474617, -0.7071067811865474617 ) ) ;
#41142 = LINE ( 'NONE', #9843, #31234 ) ;
#41143 =( BOUNDED_CURVE ( )  B_SPLINE_CURVE ( 3, ( #33549, #17872, #44809, #48883 ),
 .UNSPECIFIED., .F., .F. ) 
 B_SPLINE_CURVE_WITH_KNOTS ( ( 4, 4 ),
 ( 0.000000000000000000, 1.570796326794896558 ),
 .UNSPECIFIED. ) 
 CURVE ( )  GEOMETRIC_REPRESENTATION_ITEM ( )  RATIONAL_B_SPLINE_CURVE ( ( 1.000000000000000000, 0.8047378541243649375, 0.8047378541243649375, 1.000000000000000000 ) ) 
 REPRESENTATION_ITEM ( '' )  );
#41144 = EDGE_LOOP ( 'NONE', ( #24281, #4429, #5649, #38637, #16864 ) ) ;
#41145 = VERTEX_POINT ( 'NONE', #37412 ) ;
#41146 = DIRECTION ( 'NONE',  ( -0.4740998230350174647, -0.3386427307392981256, -0.8127425537743155903 ) ) ;
#41147 = LINE ( 'NONE', #49803, #5303 ) ;
#41148 = CARTESIAN_POINT ( 'NONE',  ( -114.9999999999987779, 17.00000000000000000, 5.000000000000004441 ) ) ;
#41149 = CARTESIAN_POINT ( 'NONE',  ( -84.94597344681494633, 2.143131898507880377E-16, 42.56828755692798438 ) ) ;
#41150 = ORIENTED_EDGE ( 'NONE', *, *, #12107, .T. ) ;
#41151 = VERTEX_POINT ( 'NONE', #14276 ) ;
#41152 =( BOUNDED_CURVE ( )  B_SPLINE_CURVE ( 3, ( #9270, #13108, #28271, #43905 ),
 .UNSPECIFIED., .F., .F. ) 
 B_SPLINE_CURVE_WITH_KNOTS ( ( 4, 4 ),
 ( 0.000000000000000000, 1.570796326794896558 ),
 .UNSPECIFIED. ) 
 CURVE ( )  GEOMETRIC_REPRESENTATION_ITEM ( )  RATIONAL_B_SPLINE_CURVE ( ( 1.000000000000000000, 0.8047378541243649375, 0.8047378541243649375, 1.000000000000000000 ) ) 
 REPRESENTATION_ITEM ( '' )  );
#41153 = CIRCLE ( 'NONE', #19870, 2.000000000000001776 ) ;
#41154 = CARTESIAN_POINT ( 'NONE',  ( -7.721099712662037540, -1.750000000000023315, -40.20683870891912903 ) ) ;
#41155 = CARTESIAN_POINT ( 'NONE',  ( -50.00000000000000000, -50.00000000000000000, 800.0000000000000000 ) ) ;
#41156 = ORIENTED_EDGE ( 'NONE', *, *, #36491, .F. ) ;
#41157 = ORIENTED_EDGE ( 'NONE', *, *, #47123, .T. ) ;
#41158 = LINE ( 'NONE', #18304, #50477 ) ;
#41159 = VECTOR ( 'NONE', #42105, 1000.000000000000000 ) ;
#41160 = DIRECTION ( 'NONE',  ( -0.000000000000000000, -0.000000000000000000, -1.000000000000000000 ) ) ;
#41161 = ORIENTED_EDGE ( 'NONE', *, *, #25079, .F. ) ;
#41162 = ORIENTED_EDGE ( 'NONE', *, *, #33065, .F. ) ;
#41163 = MECHANICAL_DESIGN_GEOMETRIC_PRESENTATION_REPRESENTATION (  '', ( #35483 ), #19038 ) ;
#41164 = CARTESIAN_POINT ( 'NONE',  ( 210.0000000000000568, 0.000000000000000000, 2.568287556927987048 ) ) ;
#41165 = LINE ( 'NONE', #5517, #9187 ) ;
#41166 = VERTEX_POINT ( 'NONE', #33304 ) ;
#41167 = CARTESIAN_POINT ( 'NONE',  ( -0.1265591857321690383, -1.213367045380180809, 9.963925895596192461 ) ) ;
#41168 = DIRECTION ( 'NONE',  ( 0.000000000000000000, 1.000000000000000000, 0.000000000000000000 ) ) ;
#41169 = DIRECTION ( 'NONE',  ( -0.000000000000000000, -0.000000000000000000, -1.000000000000000000 ) ) ;
#41170 = CARTESIAN_POINT ( 'NONE',  ( -165.0000000000000284, 16.00000000000000000, 5.000000000000004441 ) ) ;
#41171 = VECTOR ( 'NONE', #16549, 1000.000000000000000 ) ;
#41172 = CARTESIAN_POINT ( 'NONE',  ( -165.6708471809677974, -1.750000000000010436, 79.79316129108087807 ) ) ;
#41173 = ORIENTED_EDGE ( 'NONE', *, *, #4553, .T. ) ;
#41174 = CARTESIAN_POINT ( 'NONE',  ( -208.4459734468148611, -1.025126265847089657, -80.93171244307201562 ) ) ;
#41175 = LINE ( 'NONE', #1442, #24040 ) ;
#41176 = B_SPLINE_SURFACE_WITH_KNOTS ( 'NONE', 3, 3, ( 
 ( #28941, #48641, #40995, #26094 ),
 ( #21742, #17642, #49403, #36930 ),
 ( #29203, #44552, #44818, #45063 ),
 ( #37924, #18387, #33313, #33560 ) ),
 .UNSPECIFIED., .F., .F., .F.,
 ( 4, 4 ),
 ( 4, 4 ),
 ( 0.000000000000000000, 1.000000000000000000 ),
 ( 0.000000000000000000, 1.000000000000000000 ),
 .UNSPECIFIED. ) ;
#41177 = FACE_BOUND ( 'NONE', #48684, .T. ) ;
#41178 = EDGE_CURVE ( 'NONE', #21466, #20141, #29942, .T. ) ;
#41179 = DIRECTION ( 'NONE',  ( 1.000000000000000000, 0.000000000000000000, -2.958228394578793832E-31 ) ) ;
#41180 = CARTESIAN_POINT ( 'NONE',  ( 71.55402655318505367, -1.025126265847089879, 122.5682875569280128 ) ) ;
#41181 = CARTESIAN_POINT ( 'NONE',  ( 181.0000000000000000, 165.0000000000000000, -358.0000000000001705 ) ) ;
#41182 = EDGE_CURVE ( 'NONE', #42453, #46337, #2923, .T. ) ;
#41183 = CIRCLE ( 'NONE', #7618, 0.4999999999999995559 ) ;
#41184 = LINE ( 'NONE', #13981, #41880 ) ;
#41185 = ADVANCED_FACE ( 'NONE', ( #41227 ), #3193, .T. ) ;
#41186 = ORIENTED_EDGE ( 'NONE', *, *, #1454, .T. ) ;
#41187 = ADVANCED_FACE ( 'NONE', ( #19402 ), #3478, .F. ) ;
#41188 = CARTESIAN_POINT ( 'NONE',  ( 31.55402655318503236, 1.025126265847089435, 122.5682875569280128 ) ) ;
#41189 = DIRECTION ( 'NONE',  ( -0.000000000000000000, -0.000000000000000000, -1.000000000000000000 ) ) ;
#41190 = AXIS2_PLACEMENT_3D ( 'NONE', #19531, #35471, #40070 ) ;
#41191 = CARTESIAN_POINT ( 'NONE',  ( -1.540662627795934769, 1.371465786296043765, 9.894754715216725671 ) ) ;
#41192 = CARTESIAN_POINT ( 'NONE',  ( 164.9999999999999716, -184.9999999999999716, -356.0000000000014211 ) ) ;
#41193 = SPHERICAL_SURFACE ( 'NONE', #6977, 0.5000000000000000000 ) ;
#41194 = VECTOR ( 'NONE', #37981, 1000.000000000000000 ) ;
#41195 = ORIENTED_EDGE ( 'NONE', *, *, #35570, .F. ) ;
#41196 = CARTESIAN_POINT ( 'NONE',  ( -10.49999999999999467, -46.01315789473684248, -5.916985404131814619 ) ) ;
#41197 = EDGE_LOOP ( 'NONE', ( #10531, #8351, #9706, #2114 ) ) ;
#41198 = CARTESIAN_POINT ( 'NONE',  ( -168.4459734468149747, 1.025126265847089213, -37.43171244307202272 ) ) ;
#41199 = VECTOR ( 'NONE', #35102, 1000.000000000000000 ) ;
#41200 = CARTESIAN_POINT ( 'NONE',  ( 112.2789002873379758, -1.749999999999996891, 119.7931612910809065 ) ) ;
#41201 = EDGE_LOOP ( 'NONE', ( #40668, #50006, #32755, #38871, #6645, #33225 ) ) ;
#41202 = AXIS2_PLACEMENT_3D ( 'NONE', #16666, #24880, #44102 ) ;
#41203 = DIRECTION ( 'NONE',  ( 0.000000000000000000, 0.4027858274925602000, 0.9152942571496522906 ) ) ;
#41204 = CYLINDRICAL_SURFACE ( 'NONE', #50264, 1.749999999999973799 ) ;
#41205 = ORIENTED_EDGE ( 'NONE', *, *, #29958, .F. ) ;
#41206 = ORIENTED_EDGE ( 'NONE', *, *, #9251, .T. ) ;
#41207 = ORIENTED_EDGE ( 'NONE', *, *, #3877, .T. ) ;
#41208 = EDGE_CURVE ( 'NONE', #28813, #8288, #38662, .T. ) ;
#41209 = ADVANCED_FACE ( 'NONE', ( #30447 ), #46312, .F. ) ;
#41210 = CARTESIAN_POINT ( 'NONE',  ( -1.158497635116737312, 16.61944452314319420, -3.546734833711462365 ) ) ;
#41211 = FACE_OUTER_BOUND ( 'NONE', #10279, .T. ) ;
#41212 = DIRECTION ( 'NONE',  ( 1.000000000000000000, 0.000000000000000000, 0.000000000000000000 ) ) ;
#41213 = EDGE_CURVE ( 'NONE', #1381, #32520, #7608, .T. ) ;
#41214 = ORIENTED_EDGE ( 'NONE', *, *, #27469, .T. ) ;
#41215 = EDGE_CURVE ( 'NONE', #28163, #35332, #10131, .T. ) ;
#41216 = PLANE ( 'NONE',  #3003 ) ;
#41217 = PLANE ( 'NONE',  #5046 ) ;
#41218 = FILL_AREA_STYLE ('',( #32783 ) ) ;
#41219 = VERTEX_POINT ( 'NONE', #46556 ) ;
#41220 = VERTEX_POINT ( 'NONE', #47065 ) ;
#41221 = DIRECTION ( 'NONE',  ( 0.000000000000000000, 0.000000000000000000, 1.000000000000000000 ) ) ;
#41222 = EDGE_CURVE ( 'NONE', #22458, #25314, #26848, .T. ) ;
#41223 = CARTESIAN_POINT ( 'NONE',  ( 111.5540265531850537, -1.025126265847082108, 122.5682875569279702 ) ) ;
#41224 = EDGE_CURVE ( 'NONE', #40403, #26183, #45161, .T. ) ;
#41225 = CARTESIAN_POINT ( 'NONE',  ( 115.0540265531850395, 2.143131898507847836E-16, -37.43171244307205825 ) ) ;
#41226 = ORIENTED_EDGE ( 'NONE', *, *, #15392, .F. ) ;
#41227 = FACE_OUTER_BOUND ( 'NONE', #30962, .T. ) ;
#41228 = CARTESIAN_POINT ( 'NONE',  ( 2.500000000000050182, -204.9999999999999716, -234.7500000000000000 ) ) ;
#41229 = CARTESIAN_POINT ( 'NONE',  ( 2.052549611693792464, -0.2039603569406628347, 9.894754715216725671 ) ) ;
#41230 = CARTESIAN_POINT ( 'NONE',  ( 48.98697415750967821, 11.03699497439252220, -8.016098858316205167 ) ) ;
#41231 = VECTOR ( 'NONE', #48348, 1000.000000000000000 ) ;
#41232 = LINE ( 'NONE', #32797, #50248 ) ;
#41233 = CARTESIAN_POINT ( 'NONE',  ( -47.72109971266203132, -1.750000000000009548, -0.2068387089191121020 ) ) ;
#41234 = CIRCLE ( 'NONE', #19917, 4.000000000000003553 ) ;
#41235 = CARTESIAN_POINT ( 'NONE',  ( -164.9459734468149463, -1.025126265847089213, -37.43171244307202272 ) ) ;
#41236 = CARTESIAN_POINT ( 'NONE',  ( 210.0000000000000568, 0.000000000000000000, -79.18171244307201562 ) ) ;
#41237 = CARTESIAN_POINT ( 'NONE',  ( 210.0000000000000568, 0.000000000000000000, 80.81828755692798438 ) ) ;
#41238 = EDGE_CURVE ( 'NONE', #1180, #44943, #20324, .T. ) ;
#41239 = LINE ( 'NONE', #41499, #34525 ) ;
#41240 = ADVANCED_FACE ( 'NONE', ( #15556 ), #11703, .F. ) ;
#41241 = ADVANCED_FACE ( 'NONE', ( #23517 ), #39176, .F. ) ;
#41242 = VECTOR ( 'NONE', #6655, 1000.000000000000000 ) ;
#41243 = CARTESIAN_POINT ( 'NONE',  ( -166.6959734468149463, -1.750000000000010658, -79.18171244307201562 ) ) ;
#41244 = VERTEX_POINT ( 'NONE', #4265 ) ;
#41245 = CYLINDRICAL_SURFACE ( 'NONE', #35203, 1.750000000000001554 ) ;
#41246 = FACE_OUTER_BOUND ( 'NONE', #25513, .T. ) ;
#41247 = CARTESIAN_POINT ( 'NONE',  ( -4.945973446814903696, 2.143131898507912917E-16, 39.06828755692792754 ) ) ;
#41248 = EDGE_LOOP ( 'NONE', ( #38386, #49240, #44101, #27989 ) ) ;
#41249 = DIRECTION ( 'NONE',  ( -1.000000000000000000, -0.000000000000000000, -0.000000000000000000 ) ) ;
#41250 = VECTOR ( 'NONE', #46491, 1000.000000000000000 ) ;
#41251 = DIRECTION ( 'NONE',  ( -1.000000000000000000, 0.000000000000000000, 1.860490536778032451E-50 ) ) ;
#41252 = EDGE_LOOP ( 'NONE', ( #47161, #21095, #17602, #6255 ) ) ;
#41253 = DIRECTION ( 'NONE',  ( 1.860490536778032451E-50, 0.000000000000000000, 1.000000000000000000 ) ) ;
#41254 = CARTESIAN_POINT ( 'NONE',  ( -64.99999999999815259, 17.00000000000000000, 65.00000000000000000 ) ) ;
#41256 = ADVANCED_FACE ( 'NONE', ( #17066 ), #4760, .F. ) ;
#41255 = CARTESIAN_POINT ( 'NONE',  ( -125.6708471809678542, 1.749999999999996669, 1.843413822775057609 ) ) ;
#41257 = ORIENTED_EDGE ( 'NONE', *, *, #14651, .T. ) ;
#41258 = B_SPLINE_CURVE_WITH_KNOTS ( 'NONE', 3,
 ( #44938, #2860, #21886, #25990 ),
 .UNSPECIFIED., .F., .F.,
 ( 4, 4 ),
 ( 0.000000000000000000, 0.002368422649471284714 ),
 .UNSPECIFIED. ) ;
#41259 = EDGE_LOOP ( 'NONE', ( #35017, #18664, #35025, #14059 ) ) ;
#41260 = VERTEX_POINT ( 'NONE', #1432 ) ;
#41261 = ORIENTED_EDGE ( 'NONE', *, *, #50266, .T. ) ;
#41262 = PLANE ( 'NONE',  #39325 ) ;
#41263 = CARTESIAN_POINT ( 'NONE',  ( -7.129058724845069861, -15.30620660340479766, 9.178419661560148768 ) ) ;
#41264 = AXIS2_PLACEMENT_3D ( 'NONE', #6682, #11042, #30547 ) ;
#41265 = EDGE_CURVE ( 'NONE', #45334, #37195, #1001, .T. ) ;
#41266 = EDGE_LOOP ( 'NONE', ( #8302, #40609, #31717, #47754 ) ) ;
#41267 = CIRCLE ( 'NONE', #42071, 2.000000000000001776 ) ;
#41268 = LINE ( 'NONE', #12820, #15898 ) ;
#41269 = CARTESIAN_POINT ( 'NONE',  ( 194.9999999999999432, 173.0000000000000000, 372.0000000000000000 ) ) ;
#41270 = VERTEX_POINT ( 'NONE', #47321 ) ;
#41271 = PRESENTATION_LAYER_ASSIGNMENT (  '', '', ( #23252 ) ) ;
#41272 = B_SPLINE_CURVE_WITH_KNOTS ( 'NONE', 3,
 ( #9604, #48555, #25010, #48049 ),
 .UNSPECIFIED., .F., .F.,
 ( 4, 4 ),
 ( 9.305432711149857983E-16, 0.0004154657329515702127 ),
 .UNSPECIFIED. ) ;
#41273 = CARTESIAN_POINT ( 'NONE',  ( -44.94597344681493922, 2.143131898507880377E-16, -77.43171244307198720 ) ) ;
#41274 = DIRECTION ( 'NONE',  ( -0.000000000000000000, 1.000000000000000000, 0.000000000000000000 ) ) ;
#41275 = AXIS2_PLACEMENT_3D ( 'NONE', #1810, #17453, #5644 ) ;
#41276 = CARTESIAN_POINT ( 'NONE',  ( -64.99999999999971578, 17.00000000000000000, -60.00000000000000000 ) ) ;
#41277 = ADVANCED_FACE ( 'NONE', ( #5265 ), #29401, .T. ) ;
#41278 = ORIENTED_EDGE ( 'NONE', *, *, #30414, .F. ) ;
#41279 = ADVANCED_FACE ( 'NONE', ( #48066 ), #12456, .T. ) ;
#41280 = CARTESIAN_POINT ( 'NONE',  ( -48.44597344681495343, 0.000000000000000000, -120.9317124430720725 ) ) ;
#41281 = CARTESIAN_POINT ( 'NONE',  ( 169.0000000000000000, -174.9999999999999716, -111.0000000000001563 ) ) ;
#41282 = EDGE_LOOP ( 'NONE', ( #11363, #9911, #34331, #7861, #40210, #27923, #44634, #879 ) ) ;
#41283 = ORIENTED_EDGE ( 'NONE', *, *, #20547, .T. ) ;
#41284 = VERTEX_POINT ( 'NONE', #32486 ) ;
#41285 = LINE ( 'NONE', #18685, #18827 ) ;
#41286 = EDGE_CURVE ( 'NONE', #49869, #24077, #20401, .T. ) ;
#41287 = DIRECTION ( 'NONE',  ( -0.000000000000000000, -1.000000000000000000, -0.000000000000000000 ) ) ;
#41288 = B_SPLINE_SURFACE_WITH_KNOTS ( 'NONE', 3, 3, ( 
 ( #38310, #18768, #19019, #34448 ),
 ( #56, #27503, #34708, #39065 ),
 ( #14935, #11852, #11083, #30590 ),
 ( #26743, #19526, #35214, #13099 ) ),
 .UNSPECIFIED., .F., .F., .F.,
 ( 4, 4 ),
 ( 4, 4 ),
 ( 0.000000000000000000, 1.000000000000000000 ),
 ( 0.000000000000000000, 1.000000000000000000 ),
 .UNSPECIFIED. ) ;
#41289 = ORIENTED_EDGE ( 'NONE', *, *, #23022, .T. ) ;
#41290 = EDGE_CURVE ( 'NONE', #19053, #42239, #41459, .T. ) ;
#41291 = CARTESIAN_POINT ( 'NONE',  ( 0.000000000000000000, 169.0000000000000000, -356.0000000000002274 ) ) ;
#41292 = CARTESIAN_POINT ( 'NONE',  ( 1.035950918207909632, 50.00000000000000711, -2.408242355805840784 ) ) ;
#41293 = EDGE_CURVE ( 'NONE', #34716, #48470, #24020, .T. ) ;
#41294 =( BOUNDED_CURVE ( )  B_SPLINE_CURVE ( 3, ( #29882, #45502, #26040, #45745 ),
 .UNSPECIFIED., .F., .F. ) 
 B_SPLINE_CURVE_WITH_KNOTS ( ( 4, 4 ),
 ( 4.712388980384689674, 6.283185307179586232 ),
 .UNSPECIFIED. ) 
 CURVE ( )  GEOMETRIC_REPRESENTATION_ITEM ( )  RATIONAL_B_SPLINE_CURVE ( ( 1.000000000000000000, 0.8047378541243649375, 0.8047378541243649375, 1.000000000000000000 ) ) 
 REPRESENTATION_ITEM ( '' )  );
#41295 = FACE_OUTER_BOUND ( 'NONE', #26612, .T. ) ;
#41296 = VECTOR ( 'NONE', #40745, 1000.000000000000000 ) ;
#41297 = DIRECTION ( 'NONE',  ( 1.000000000000000000, 0.000000000000000000, -0.000000000000000000 ) ) ;
#41298 = VERTEX_POINT ( 'NONE', #927 ) ;
#41299 = CARTESIAN_POINT ( 'NONE',  ( 0.000000000000000000, 43.33333333333339255, 790.0000000000000000 ) ) ;
#41300 = CARTESIAN_POINT ( 'NONE',  ( 165.0000000000000000, -174.9999999999999716, -111.0000000000001563 ) ) ;
#41301 =( BOUNDED_CURVE ( )  B_SPLINE_CURVE ( 3, ( #43565, #34614, #39231, #19191 ),
 .UNSPECIFIED., .F., .F. ) 
 B_SPLINE_CURVE_WITH_KNOTS ( ( 4, 4 ),
 ( 0.000000000000000000, 1.570796326794896558 ),
 .UNSPECIFIED. ) 
 CURVE ( )  GEOMETRIC_REPRESENTATION_ITEM ( )  RATIONAL_B_SPLINE_CURVE ( ( 1.000000000000000000, 0.8047378541243649375, 0.8047378541243649375, 1.000000000000000000 ) ) 
 REPRESENTATION_ITEM ( '' )  );
#41302 = ADVANCED_FACE ( 'NONE', ( #21164 ), #1182, .T. ) ;
#41303 = DIRECTION ( 'NONE',  ( 0.000000000000000000, -1.000000000000000000, 0.000000000000000000 ) ) ;
#41304 = EDGE_LOOP ( 'NONE', ( #43617, #4725, #27444, #15271 ) ) ;
#41305 = CONTEXT_DEPENDENT_SHAPE_REPRESENTATION ( #4022, #31097 ) ;
#41306 = CARTESIAN_POINT ( 'NONE',  ( 0.000000000000000000, 164.9999999999999716, 10.00000000000000000 ) ) ;
#41307 = ADVANCED_FACE ( 'NONE', ( #28608 ), #43752, .F. ) ;
#41308 = AXIS2_PLACEMENT_3D ( 'NONE', #25954, #22594, #30553 ) ;
#41309 = CIRCLE ( 'NONE', #19172, 1.750000000000001554 ) ;
#41310 = CARTESIAN_POINT ( 'NONE',  ( 181.0000000000000000, -254.4999999999999432, -349.9999999999999432 ) ) ;
#41311 = FACE_OUTER_BOUND ( 'NONE', #11634, .T. ) ;
#41312 = ORIENTED_EDGE ( 'NONE', *, *, #47152, .F. ) ;
#41313 = PLANE ( 'NONE',  #14875 ) ;
#41314 = AXIS2_PLACEMENT_3D ( 'NONE', #47159, #39012, #15397 ) ;
#41315 = DIRECTION ( 'NONE',  ( 0.000000000000000000, 1.000000000000000000, -2.537652627714642000E-15 ) ) ;
#41316 =( BOUNDED_CURVE ( )  B_SPLINE_CURVE ( 3, ( #23642, #15951, #32360, #19787 ),
 .UNSPECIFIED., .F., .F. ) 
 B_SPLINE_CURVE_WITH_KNOTS ( ( 4, 4 ),
 ( 0.000000000000000000, 1.570796326794896558 ),
 .UNSPECIFIED. ) 
 CURVE ( )  GEOMETRIC_REPRESENTATION_ITEM ( )  RATIONAL_B_SPLINE_CURVE ( ( 1.000000000000000000, 0.8047378541243649375, 0.8047378541243649375, 1.000000000000000000 ) ) 
 REPRESENTATION_ITEM ( '' )  );
#41317 = CARTESIAN_POINT ( 'NONE',  ( -30.12518629743573584, -14.70074613238887551, 1.847720168420772691 ) ) ;
#41318 = CARTESIAN_POINT ( 'NONE',  ( -70.00000000000002842, 17.00000000000000000, -114.9999999999999858 ) ) ;
#41319 = CARTESIAN_POINT ( 'NONE',  ( 356.0000000000002842, 165.0000000000000000, -110.0000000000002132 ) ) ;
#41320 = ORIENTED_EDGE ( 'NONE', *, *, #31861, .F. ) ;
#41321 = CYLINDRICAL_SURFACE ( 'NONE', #9234, 1.750000000000001554 ) ;
#41322 = B_SPLINE_CURVE_WITH_KNOTS ( 'NONE', 3,
 ( #18736, #33416, #18495, #45919 ),
 .UNSPECIFIED., .F., .F.,
 ( 4, 4 ),
 ( 0.000000000000000000, 0.0001252128669263171442 ),
 .UNSPECIFIED. ) ;
#41323 = ORIENTED_EDGE ( 'NONE', *, *, #38374, .T. ) ;
#41324 = LINE ( 'NONE', #6174, #8190 ) ;
#41325 = ORIENTED_EDGE ( 'NONE', *, *, #6572, .T. ) ;
#41326 = LINE ( 'NONE', #11033, #32806 ) ;
#41327 = CARTESIAN_POINT ( 'NONE',  ( -64.99999999999909051, 16.00000000000000000, -24.99999999999999289 ) ) ;
#41328 = CARTESIAN_POINT ( 'NONE',  ( -6.695973446814940111, 1.750000000000024203, -79.18171244307201562 ) ) ;
#41329 = ORIENTED_EDGE ( 'NONE', *, *, #16314, .T. ) ;
#41330 = VECTOR ( 'NONE', #13969, 1000.000000000000000 ) ;
#41331 = DIRECTION ( 'NONE',  ( -1.000000000000000000, 0.000000000000000000, 0.000000000000000000 ) ) ;
#41332 = VERTEX_POINT ( 'NONE', #28371 ) ;
#41333 = LINE ( 'NONE', #29531, #45339 ) ;
#41334 = AXIS2_PLACEMENT_3D ( 'NONE', #25284, #32502, #25538 ) ;
#41335 = CARTESIAN_POINT ( 'NONE',  ( -164.9459734468149463, 2.143131898507880377E-16, -77.43171244307204404 ) ) ;
#41336 = DIRECTION ( 'NONE',  ( -1.000000000000000000, -0.000000000000000000, -0.000000000000000000 ) ) ;
#41337 = CARTESIAN_POINT ( 'NONE',  ( 0.000000000000000000, 0.000000000000000000, 790.0000000000000000 ) ) ;
#41338 = ORIENTED_EDGE ( 'NONE', *, *, #9817, .T. ) ;
#41339 = VERTEX_POINT ( 'NONE', #8862 ) ;
#41340 = CARTESIAN_POINT ( 'NONE',  ( 0.03371980368970583369, 1.221991649883343412, 9.987567862361069970 ) ) ;
#41341 = ADVANCED_FACE ( 'NONE', ( #40173 ), #5009, .T. ) ;
#41342 = ORIENTED_EDGE ( 'NONE', *, *, #43707, .F. ) ;
#41343 = EDGE_CURVE ( 'NONE', #39358, #39539, #6521, .T. ) ;
#41344 = DIRECTION ( 'NONE',  ( 0.000000000000000000, -0.000000000000000000, 1.000000000000000000 ) ) ;
#41345 = AXIS2_PLACEMENT_3D ( 'NONE', #33594, #16491, #49183 ) ;
#41346 = ORIENTED_EDGE ( 'NONE', *, *, #42799, .T. ) ;
#41347 = CARTESIAN_POINT ( 'NONE',  ( -19.99999999999846523, 17.00000000000000000, 35.00000000000000000 ) ) ;
#41348 = ADVANCED_FACE ( 'NONE', ( #25270 ), #49326, .T. ) ;
#41349 = DIRECTION ( 'NONE',  ( 0.000000000000000000, 0.000000000000000000, 1.000000000000000000 ) ) ;
#41350 = VERTEX_POINT ( 'NONE', #21410 ) ;
#41351 = AXIS2_PLACEMENT_3D ( 'NONE', #41486, #30184, #5830 ) ;
#41352 = CARTESIAN_POINT ( 'NONE',  ( -19.99999999999815969, 17.00000000000000000, 65.00000000000000000 ) ) ;
#41353 = FACE_OUTER_BOUND ( 'NONE', #16257, .T. ) ;
#41354 = EDGE_CURVE ( 'NONE', #30042, #17677, #1677, .T. ) ;
#41355 = CARTESIAN_POINT ( 'NONE',  ( -48.44597344681495343, 0.000000000000000000, -157.4317124430720014 ) ) ;
#41356 = CARTESIAN_POINT ( 'NONE',  ( -204.9459734468149747, 0.000000000000000000, 162.5682875569279702 ) ) ;
#41357 = EDGE_CURVE ( 'NONE', #3215, #5399, #6288, .T. ) ;
#41358 = DIRECTION ( 'NONE',  ( -0.000000000000000000, -0.000000000000000000, -1.000000000000000000 ) ) ;
#41359 = ORIENTED_EDGE ( 'NONE', *, *, #32456, .F. ) ;
#41360 = ORIENTED_EDGE ( 'NONE', *, *, #1922, .T. ) ;
#41361 = CARTESIAN_POINT ( 'NONE',  ( 130.0000000000008811, 17.00000000000000000, -24.99999999999999289 ) ) ;
#41362 = ADVANCED_FACE ( 'NONE', ( #41931 ), #10623, .F. ) ;
#41363 = PLANE ( 'NONE',  #40666 ) ;
#41364 = DIRECTION ( 'NONE',  ( -1.000000000000000000, 0.000000000000000000, 0.000000000000000000 ) ) ;
#41365 = ADVANCED_FACE ( 'NONE', ( #33989 ), #41426, .F. ) ;
#41366 = CARTESIAN_POINT ( 'NONE',  ( 9.645054515263739248, -2.693981805359395576, 6.429802539306495035 ) ) ;
#41367 = ORIENTED_EDGE ( 'NONE', *, *, #24874, .T. ) ;
#41368 = CARTESIAN_POINT ( 'NONE',  ( 0.3862712429686815385, 1.188820645368943385, 9.972675548442461846 ) ) ;
#41369 = ORIENTED_EDGE ( 'NONE', *, *, #14430, .T. ) ;
#41370 = CARTESIAN_POINT ( 'NONE',  ( -126.6959734468149321, -1.749999999999996891, 160.8182875569279702 ) ) ;
#41371 = LINE ( 'NONE', #1874, #24460 ) ;
#41372 = CARTESIAN_POINT ( 'NONE',  ( 111.5540265531850679, 0.000000000000000000, 165.0000000000000000 ) ) ;
#41373 = AXIS2_PLACEMENT_3D ( 'NONE', #32254, #32008, #20693 ) ;
#41374 = CARTESIAN_POINT ( 'NONE',  ( -114.9999999999978542, 17.00000000000000000, 95.00000000000000000 ) ) ;
#41375 = DIRECTION ( 'NONE',  ( 0.5038710255240859137, 0.000000000000000000, -0.8637789008984335659 ) ) ;
#41376 = AXIS2_PLACEMENT_3D ( 'NONE', #17526, #4964, #21368 ) ;
#41377 = CARTESIAN_POINT ( 'NONE',  ( -128.4459734468149179, 0.000000000000000000, -0.9317124430719969652 ) ) ;
#41378 = ORIENTED_EDGE ( 'NONE', *, *, #3558, .F. ) ;
#41379 = CARTESIAN_POINT ( 'NONE',  ( 75.05402655318509630, 2.143131898507880377E-16, 39.06828755692795596 ) ) ;
#41380 = DIRECTION ( 'NONE',  ( 0.000000000000000000, 0.000000000000000000, -1.000000000000000000 ) ) ;
#41381 = CARTESIAN_POINT ( 'NONE',  ( 31.55402655318503236, -1.025126265847089435, -157.4317124430720582 ) ) ;
#41382 = FACE_OUTER_BOUND ( 'NONE', #7151, .T. ) ;
#41383 = ORIENTED_EDGE ( 'NONE', *, *, #33534, .T. ) ;
#41384 = VECTOR ( 'NONE', #44708, 1000.000000000000000 ) ;
#41385 = ORIENTED_EDGE ( 'NONE', *, *, #34963, .F. ) ;
#41387 = EDGE_CURVE ( 'NONE', #33331, #13763, #15980, .T. ) ;
#41386 = DIRECTION ( 'NONE',  ( 1.000000000000000000, 0.000000000000000000, 0.000000000000000000 ) ) ;
#41388 = DIRECTION ( 'NONE',  ( -0.000000000000000000, -0.000000000000000000, -1.000000000000000000 ) ) ;
#41389 = AXIS2_PLACEMENT_3D ( 'NONE', #45684, #10563, #10819 ) ;
#41390 = CARTESIAN_POINT ( 'NONE',  ( -239.0000000000000853, -165.6999999999999602, 250.3600000000000136 ) ) ;
#41391 = AXIS2_PLACEMENT_3D ( 'NONE', #37301, #18946, #45179 ) ;
#41392 = EDGE_CURVE ( 'NONE', #10758, #6309, #43271, .T. ) ;
#41393 = CARTESIAN_POINT ( 'NONE',  ( 14.48769039275578407, 30.44468701195595983, 8.807470649214879543 ) ) ;
#41394 = ORIENTED_EDGE ( 'NONE', *, *, #35375, .F. ) ;
#41395 = CARTESIAN_POINT ( 'NONE',  ( 210.0000000000000568, 0.000000000000000000, -157.4317124430720298 ) ) ;
#41396 =( BOUNDED_CURVE ( )  B_SPLINE_CURVE ( 3, ( #21716, #21214, #26077, #26337 ),
 .UNSPECIFIED., .F., .F. ) 
 B_SPLINE_CURVE_WITH_KNOTS ( ( 4, 4 ),
 ( 0.000000000000000000, 1.570796326794896558 ),
 .UNSPECIFIED. ) 
 CURVE ( )  GEOMETRIC_REPRESENTATION_ITEM ( )  RATIONAL_B_SPLINE_CURVE ( ( 1.000000000000000000, 0.8047378541243649375, 0.8047378541243649375, 1.000000000000000000 ) ) 
 REPRESENTATION_ITEM ( '' )  );
#41397 = DIRECTION ( 'NONE',  ( 0.000000000000000000, 0.000000000000000000, 1.000000000000000000 ) ) ;
#41398 = DIRECTION ( 'NONE',  ( -1.000000000000000000, -0.000000000000000000, -0.000000000000000000 ) ) ;
#41399 = EDGE_LOOP ( 'NONE', ( #48059, #21774, #36433, #43750, #37078, #43245 ) ) ;
#41400 = ORIENTED_EDGE ( 'NONE', *, *, #19048, .T. ) ;
#41401 = CARTESIAN_POINT ( 'NONE',  ( -126.6959734468149321, 0.000000000000000000, -165.0000000000000000 ) ) ;
#41402 = CARTESIAN_POINT ( 'NONE',  ( 15.44803555374680393, 6.237487519713364570, -3.546734833711462365 ) ) ;
#41403 = VECTOR ( 'NONE', #47033, 1000.000000000000000 ) ;
#41404 = ORIENTED_EDGE ( 'NONE', *, *, #43268, .F. ) ;
#41405 = VERTEX_POINT ( 'NONE', #37851 ) ;
#41406 = CARTESIAN_POINT ( 'NONE',  ( 35.05402655318504657, 2.143131898507880377E-16, -120.9317124430720725 ) ) ;
#41407 = CARTESIAN_POINT ( 'NONE',  ( -85.67084718096784002, -1.750000000000009548, 41.84341382277508359 ) ) ;
#41408 = VECTOR ( 'NONE', #22000, 1000.000000000000000 ) ;
#41409 = EDGE_LOOP ( 'NONE', ( #30159, #40402 ) ) ;
#41410 = DIRECTION ( 'NONE',  ( 1.000000000000000000, 0.000000000000000000, 0.000000000000000000 ) ) ;
#41411 = VERTEX_POINT ( 'NONE', #2181 ) ;
#41412 = VECTOR ( 'NONE', #21110, 1000.000000000000000 ) ;
#41413 = CARTESIAN_POINT ( 'NONE',  ( -126.6959734468149321, -1.749999999999997113, -39.18171244307202983 ) ) ;
#41415 = VECTOR ( 'NONE', #28060, 1000.000000000000000 ) ;
#41414 = CARTESIAN_POINT ( 'NONE',  ( -164.9999999999997442, 17.00000000000000000, -84.99999999999998579 ) ) ;
#41416 =( GEOMETRIC_REPRESENTATION_CONTEXT ( 3 ) GLOBAL_UNCERTAINTY_ASSIGNED_CONTEXT ( ( #31119 ) ) GLOBAL_UNIT_ASSIGNED_CONTEXT ( ( #19591, #3944, #4209 ) ) REPRESENTATION_CONTEXT ( 'NONE', 'WORKASPACE' ) );
#41417 = VERTEX_POINT ( 'NONE', #45496 ) ;
#41418 = VECTOR ( 'NONE', #37157, 1000.000000000000000 ) ;
#41419 = ORIENTED_EDGE ( 'NONE', *, *, #39050, .F. ) ;
#41420 = EDGE_CURVE ( 'NONE', #26020, #559, #44748, .T. ) ;
#41421 = CARTESIAN_POINT ( 'NONE',  ( -8.445973446814976526, 0.000000000000000000, 122.5682875569279986 ) ) ;
#41422 = CARTESIAN_POINT ( 'NONE',  ( 135.0000000000019043, 16.00000000000000000, 65.00000000000000000 ) ) ;
#41423 = EDGE_LOOP ( 'NONE', ( #28089, #14551, #22619, #31018 ) ) ;
#41424 = LINE ( 'NONE', #45738, #19033 ) ;
#41425 = ORIENTED_EDGE ( 'NONE', *, *, #9613, .F. ) ;
#41426 = PLANE ( 'NONE',  #26630 ) ;
#41427 = FILL_AREA_STYLE_COLOUR ( '', #47715 ) ;
#41428 = ORIENTED_EDGE ( 'NONE', *, *, #42554, .T. ) ;
#41429 = CARTESIAN_POINT ( 'NONE',  ( 31.55402655318503236, -1.025126265847089213, 159.0682875569279418 ) ) ;
#41430 = CARTESIAN_POINT ( 'NONE',  ( 114.3291528190321173, -1.749999999999996669, -38.15658617722495194 ) ) ;
#41431 = DIRECTION ( 'NONE',  ( -1.000000000000000000, 0.000000000000000000, 0.000000000000000000 ) ) ;
#41432 = DIRECTION ( 'NONE',  ( 0.000000000000000000, 0.000000000000000000, 1.000000000000000000 ) ) ;
#41433 = LINE ( 'NONE', #6295, #10200 ) ;
#41434 = EDGE_LOOP ( 'NONE', ( #43983, #4244 ) ) ;
#41435 = CARTESIAN_POINT ( 'NONE',  ( -164.9999999999990905, 17.00000000000000000, -24.99999999999999289 ) ) ;
#41436 = DIRECTION ( 'NONE',  ( 0.000000000000000000, 1.000000000000000000, 0.000000000000000000 ) ) ;
#41437 = DIRECTION ( 'NONE',  ( 0.000000000000000000, -1.000000000000000000, 0.000000000000000000 ) ) ;
#41438 = CARTESIAN_POINT ( 'NONE',  ( 27.73884755486784570, -25.23502201956245017, 7.697694107796188234 ) ) ;
#41439 = VECTOR ( 'NONE', #46028, 1000.000000000000000 ) ;
#41440 = CARTESIAN_POINT ( 'NONE',  ( 185.0000000000000000, -81.49999999999997158, -350.0000000000001705 ) ) ;
#41441 = CARTESIAN_POINT ( 'NONE',  ( -206.6959734468149463, 1.750000000000010658, -119.1817124430720440 ) ) ;
#41442 = VECTOR ( 'NONE', #13455, 1000.000000000000114 ) ;
#41443 = FACE_OUTER_BOUND ( 'NONE', #17347, .T. ) ;
#41444 = VECTOR ( 'NONE', #42558, 1000.000000000000000 ) ;
#41445 = CARTESIAN_POINT ( 'NONE',  ( -556.8973046169135159, 54.43801056904003133, -64.63743994998280584 ) ) ;
#41446 = EDGE_CURVE ( 'NONE', #26878, #23932, #13465, .T. ) ;
#41447 = VERTEX_POINT ( 'NONE', #9622 ) ;
#41448 = CARTESIAN_POINT ( 'NONE',  ( 22.18397680750686263, 25.02304503454544360, -8.917361510505369182 ) ) ;
#41449 =( BOUNDED_CURVE ( )  B_SPLINE_CURVE ( 3, ( #41149, #5999, #41407, #6272 ),
 .UNSPECIFIED., .F., .F. ) 
 B_SPLINE_CURVE_WITH_KNOTS ( ( 4, 4 ),
 ( 3.141592653589793116, 4.712388980384689674 ),
 .UNSPECIFIED. ) 
 CURVE ( )  GEOMETRIC_REPRESENTATION_ITEM ( )  RATIONAL_B_SPLINE_CURVE ( ( 1.000000000000000000, 0.8047378541243649375, 0.8047378541243649375, 1.000000000000000000 ) ) 
 REPRESENTATION_ITEM ( '' )  );
#41450 = AXIS2_PLACEMENT_3D ( 'NONE', #29482, #29994, #10991 ) ;
#41451 = CARTESIAN_POINT ( 'NONE',  ( -33.08717642956897009, -5.870837526464928402, -8.016098858316199838 ) ) ;
#41452 = VECTOR ( 'NONE', #27739, 1000.000000000000000 ) ;
#41453 = CARTESIAN_POINT ( 'NONE',  ( -1.578643388466005160, 1.550786058692512182, 9.881002359080275355 ) ) ;
#41454 = CARTESIAN_POINT ( 'NONE',  ( -124.9459734468149463, 2.143131898507847836E-16, 42.56828755692795596 ) ) ;
#41455 = PLANE ( 'NONE',  #33223 ) ;
#41456 =( BOUNDED_CURVE ( )  B_SPLINE_CURVE ( 3, ( #50081, #2918, #26539, #34766 ),
 .UNSPECIFIED., .F., .F. ) 
 B_SPLINE_CURVE_WITH_KNOTS ( ( 4, 4 ),
 ( 3.141592653589793116, 4.712388980384689674 ),
 .UNSPECIFIED. ) 
 CURVE ( )  GEOMETRIC_REPRESENTATION_ITEM ( )  RATIONAL_B_SPLINE_CURVE ( ( 1.000000000000000000, 0.8047378541243649375, 0.8047378541243649375, 1.000000000000000000 ) ) 
 REPRESENTATION_ITEM ( '' )  );
#41457 = ORIENTED_EDGE ( 'NONE', *, *, #3926, .T. ) ;
#41458 = EDGE_LOOP ( 'NONE', ( #14303, #24337, #27918, #43017 ) ) ;
#41459 = B_SPLINE_CURVE_WITH_KNOTS ( 'NONE', 3,
 ( #27873, #9367, #32227, #43503 ),
 .UNSPECIFIED., .F., .F.,
 ( 4, 4 ),
 ( 0.000000000000000000, 2.647279941188464684E-05 ),
 .UNSPECIFIED. ) ;
#41460 = LINE ( 'NONE', #41961, #16055 ) ;
#41461 = AXIS2_PLACEMENT_3D ( 'NONE', #41401, #26265, #49048 ) ;
#41462 = CARTESIAN_POINT ( 'NONE',  ( -1.437255894074058515, 3.713052624461494755, 6.606856988583542645E-16 ) ) ;
#41463 = ORIENTED_EDGE ( 'NONE', *, *, #36405, .F. ) ;
#41464 = CARTESIAN_POINT ( 'NONE',  ( -11.73320209285699889, 11.96063479729179768, 9.403735324607438884 ) ) ;
#41465 = FACE_OUTER_BOUND ( 'NONE', #7789, .T. ) ;
#41466 = ORIENTED_EDGE ( 'NONE', *, *, #46511, .F. ) ;
#41467 = ORIENTED_EDGE ( 'NONE', *, *, #7095, .F. ) ;
#41468 = VERTEX_POINT ( 'NONE', #14211 ) ;
#41469 = FACE_OUTER_BOUND ( 'NONE', #22709, .T. ) ;
#41470 = DIRECTION ( 'NONE',  ( -1.000000000000000000, 0.000000000000000000, 0.000000000000000000 ) ) ;
#41471 = AXIS2_PLACEMENT_3D ( 'NONE', #33471, #28852, #25503 ) ;
#41472 = VERTEX_POINT ( 'NONE', #17817 ) ;
#41473 = LINE ( 'NONE', #10926, #43959 ) ;
#41474 = CIRCLE ( 'NONE', #26755, 50.00000000000000000 ) ;
#41475 = CARTESIAN_POINT ( 'NONE',  ( 115.0540265531850395, 2.143131898507847836E-16, 39.06828755692798438 ) ) ;
#41476 = CARTESIAN_POINT ( 'NONE',  ( 0.000000000000000000, 389.0218519071287346, 192.5658166940287970 ) ) ;
#41477 = ORIENTED_EDGE ( 'NONE', *, *, #5754, .T. ) ;
#41478 = AXIS2_PLACEMENT_3D ( 'NONE', #31463, #7351, #49874 ) ;
#41479 = EDGE_LOOP ( 'NONE', ( #3348, #22904, #393, #5794 ) ) ;
#41480 = CARTESIAN_POINT ( 'NONE',  ( 155.0540265531850537, -1.025126265847088991, 159.0682875569279418 ) ) ;
#41481 = ADVANCED_FACE ( 'NONE', ( #37098 ), #13715, .F. ) ;
#41482 = CARTESIAN_POINT ( 'NONE',  ( -34.08355720199904226, 2.371364769369340042, 7.455576670931136185 ) ) ;
#41483 = DIRECTION ( 'NONE',  ( 6.938893903907232322E-16, -1.000000000000000000, 0.000000000000000000 ) ) ;
#41484 = ORIENTED_EDGE ( 'NONE', *, *, #47440, .F. ) ;
#41485 = EDGE_CURVE ( 'NONE', #1912, #3402, #1665, .T. ) ;
#41486 = CARTESIAN_POINT ( 'NONE',  ( 181.0000000000000000, -168.9999999999999432, -340.0000000000001137 ) ) ;
#41487 = CARTESIAN_POINT ( 'NONE',  ( 210.0000000000000568, 0.000000000000000000, -157.4317124430720298 ) ) ;
#41488 = EDGE_CURVE ( 'NONE', #1022, #47399, #8200, .T. ) ;
#41489 = CIRCLE ( 'NONE', #22624, 4.000000000000003553 ) ;
#41490 = DIRECTION ( 'NONE',  ( 0.000000000000000000, 1.000000000000000000, 0.000000000000000000 ) ) ;
#41491 = CARTESIAN_POINT ( 'NONE',  ( -88.44597344681494633, 1.025126265847088991, -157.4317124430720582 ) ) ;
#41492 = AXIS2_PLACEMENT_3D ( 'NONE', #13595, #29250, #13087 ) ;
#41493 = CARTESIAN_POINT ( 'NONE',  ( 2.569099690548740877, -50.00000000000000711, 3.199614146704519602 ) ) ;
#41494 = EDGE_CURVE ( 'NONE', #28510, #43275, #50383, .T. ) ;
#41495 = CARTESIAN_POINT ( 'NONE',  ( 164.9999999999999716, 17.00000000000000000, -1.387778780781445676E-14 ) ) ;
#41496 = ADVANCED_FACE ( 'NONE', ( #45240 ), #2425, .F. ) ;
#41497 = DIRECTION ( 'NONE',  ( 0.000000000000000000, -1.000000000000000000, -3.186989995019654210E-49 ) ) ;
#41498 = ADVANCED_FACE ( 'NONE', ( #30912 ), #7041, .T. ) ;
#41499 = CARTESIAN_POINT ( 'NONE',  ( -69.99999999999847944, 16.00000000000000000, 35.00000000000000000 ) ) ;
#41500 = CARTESIAN_POINT ( 'NONE',  ( -25.63461350838931807, 43.17876197216396861, -8.016098858316199838 ) ) ;
#41501 = ORIENTED_EDGE ( 'NONE', *, *, #5889, .F. ) ;
#41502 = DIRECTION ( 'NONE',  ( -0.000000000000000000, 1.000000000000000000, 0.000000000000000000 ) ) ;
#41503 = CARTESIAN_POINT ( 'NONE',  ( 151.5540265531850537, 0.000000000000000000, 165.0000000000000000 ) ) ;
#41504 = ADVANCED_FACE ( 'NONE', ( #11905 ), #15252, .T. ) ;
#41505 = ADVANCED_FACE ( 'NONE', ( #18566 ), #11649, .F. ) ;
#41506 = CARTESIAN_POINT ( 'NONE',  ( -46.11867747200561496, 19.86470446310265103, -8.016098858316205167 ) ) ;
#41508 = EDGE_LOOP ( 'NONE', ( #23950, #4288, #14708, #45954, #7413 ) ) ;
#41507 = EDGE_CURVE ( 'NONE', #35844, #38360, #34762, .T. ) ;
#41509 = LINE ( 'NONE', #30465, #10909 ) ;
#41510 = ADVANCED_FACE ( 'NONE', ( #27036 ), #42174, .T. ) ;
#41511 = VECTOR ( 'NONE', #41780, 1000.000000000000000 ) ;
#41512 = CARTESIAN_POINT ( 'NONE',  ( 154.3291528190321458, 1.750000000000009548, -38.15658617722494483 ) ) ;
#41513 = ORIENTED_EDGE ( 'NONE', *, *, #2147, .T. ) ;
#41514 = CARTESIAN_POINT ( 'NONE',  ( 135.0000000000000000, 17.00000000000000000, -90.00000000000000000 ) ) ;
#41515 = LINE ( 'NONE', #2753, #47547 ) ;
#41516 = CARTESIAN_POINT ( 'NONE',  ( 168.9999999999999716, 10.00000000000006395, -340.0000000000001137 ) ) ;
#41517 = FACE_OUTER_BOUND ( 'NONE', #32527, .T. ) ;
#41518 = EDGE_CURVE ( 'NONE', #36849, #7843, #15742, .T. ) ;
#41519 = EDGE_LOOP ( 'NONE', ( #10345, #8350, #49801, #34669, #3555, #46502 ) ) ;
#41520 = DIRECTION ( 'NONE',  ( -0.000000000000000000, -1.000000000000000000, -0.000000000000000000 ) ) ;
#41521 = EDGE_LOOP ( 'NONE', ( #8758, #25562, #14923, #20623, #6781, #24722 ) ) ;
#41522 = ORIENTED_EDGE ( 'NONE', *, *, #33986, .F. ) ;
#41523 = ORIENTED_EDGE ( 'NONE', *, *, #46982, .F. ) ;
#41524 = DIRECTION ( 'NONE',  ( -1.000000000000000000, 0.000000000000000000, -0.000000000000000000 ) ) ;
#41525 = FACE_OUTER_BOUND ( 'NONE', #33161, .T. ) ;
#41526 = LINE ( 'NONE', #5870, #27791 ) ;
#41527 = CARTESIAN_POINT ( 'NONE',  ( 80.00000000000028422, 16.00000000000000000, -84.99999999999998579 ) ) ;
#41528 = CARTESIAN_POINT ( 'NONE',  ( 341.9999999999999432, 167.8284271247462982, -342.8284271247464972 ) ) ;
#41529 = ADVANCED_FACE ( 'NONE', ( #34499 ), #7550, .F. ) ;
#41530 = VERTEX_POINT ( 'NONE', #27564 ) ;
#41531 = AXIS2_PLACEMENT_3D ( 'NONE', #5047, #32771, #13942 ) ;
#41532 = LINE ( 'NONE', #14579, #29709 ) ;
#41533 = FACE_OUTER_BOUND ( 'NONE', #20825, .T. ) ;
#41534 = CARTESIAN_POINT ( 'NONE',  ( 181.0000000000000568, 175.0000000000000284, 341.9999999999998863 ) ) ;
#41535 = EDGE_CURVE ( 'NONE', #37507, #15868, #11789, .T. ) ;
#41536 = EDGE_LOOP ( 'NONE', ( #17457, #32523, #41150, #9609, #29653, #41915, #10032, #49074 ) ) ;
#41537 = ADVANCED_FACE ( 'NONE', ( #19341 ), #8065, .F. ) ;
#41538 = CARTESIAN_POINT ( 'NONE',  ( 80.00000000000092371, 17.00000000000000000, -24.99999999999999289 ) ) ;
#41539 = ORIENTED_EDGE ( 'NONE', *, *, #4904, .T. ) ;
#41540 = ORIENTED_EDGE ( 'NONE', *, *, #18398, .F. ) ;
#41541 = VERTEX_POINT ( 'NONE', #18815 ) ;
#41542 = CARTESIAN_POINT ( 'NONE',  ( 135.0000000000006253, 17.00000000000000000, -54.99999999999999289 ) ) ;
#41543 = ADVANCED_FACE ( 'NONE', ( #30392 ), #15491, .F. ) ;
#41544 = FACE_OUTER_BOUND ( 'NONE', #18990, .T. ) ;
#41545 = ORIENTED_EDGE ( 'NONE', *, *, #4687, .T. ) ;
#41546 = EDGE_CURVE ( 'NONE', #43135, #11587, #9446, .T. ) ;
#41547 = CYLINDRICAL_SURFACE ( 'NONE', #36435, 1.750000000000001554 ) ;
#41548 = DIRECTION ( 'NONE',  ( -0.000000000000000000, -1.000000000000000000, -0.000000000000000000 ) ) ;
#41549 = CARTESIAN_POINT ( 'NONE',  ( 1.872530400643593440, -0.3103573527826896106, 9.900811091504552408 ) ) ;
#41550 = DIRECTION ( 'NONE',  ( -0.000000000000000000, -0.000000000000000000, -1.000000000000000000 ) ) ;
#41551 = CIRCLE ( 'NONE', #48056, 3.749999999999975575 ) ;
#41552 = ORIENTED_EDGE ( 'NONE', *, *, #21144, .T. ) ;
#41553 = CARTESIAN_POINT ( 'NONE',  ( -114.9999999999997158, 16.00000000000000000, -84.99999999999998579 ) ) ;
#41554 = CARTESIAN_POINT ( 'NONE',  ( -125.6708471809678542, -1.749999999999997113, 79.79316129108087807 ) ) ;
#41555 = CARTESIAN_POINT ( 'NONE',  ( -64.99999999999909051, 16.00000000000000000, -24.99999999999999289 ) ) ;
#41556 = EDGE_CURVE ( 'NONE', #29610, #11124, #9829, .T. ) ;
#41557 = ORIENTED_EDGE ( 'NONE', *, *, #35712, .T. ) ;
#41558 = LINE ( 'NONE', #2301, #30632 ) ;
#41559 = CARTESIAN_POINT ( 'NONE',  ( -1.011271242968677875, -0.7347315653656004697, 3.333333333333333481 ) ) ;
#41560 = ADVANCED_FACE ( 'NONE', ( #19076 ), #50338, .T. ) ;
#41561 = CARTESIAN_POINT ( 'NONE',  ( 0.4400426740873927822, -2.015233077865103972, 9.886433018048071730 ) ) ;
#41562 = CYLINDRICAL_SURFACE ( 'NONE', #6006, 2.000000000000001776 ) ;
#41563 = ORIENTED_EDGE ( 'NONE', *, *, #5835, .T. ) ;
#41564 = DIRECTION ( 'NONE',  ( -1.000000000000000000, 0.000000000000000000, 1.860490536778032451E-50 ) ) ;
#41565 = CARTESIAN_POINT ( 'NONE',  ( 6.508636631827673824, 15.75743548351451295, 8.953103998512858652 ) ) ;
#41566 = FACE_OUTER_BOUND ( 'NONE', #37388, .T. ) ;
#41567 = DIRECTION ( 'NONE',  ( -1.000000000000000000, -0.000000000000000000, -0.000000000000000000 ) ) ;
#41568 = CARTESIAN_POINT ( 'NONE',  ( 111.5540265531850679, 0.000000000000000000, 82.56828755692797017 ) ) ;
#41570 = ORIENTED_EDGE ( 'NONE', *, *, #49121, .F. ) ;
#41569 = EDGE_CURVE ( 'NONE', #325, #26536, #31413, .T. ) ;
#41571 = CARTESIAN_POINT ( 'NONE',  ( 3.525518878623022268, -1.771455639577098395, 6.494306196954933164 ) ) ;
#41572 = ADVANCED_FACE ( 'NONE', ( #8316 ), #31921, .T. ) ;
#41573 = EDGE_LOOP ( 'NONE', ( #25643, #24548, #11557, #48949, #45986, #721, #43394, #25630 ) ) ;
#41574 = DIRECTION ( 'NONE',  ( -1.000000000000000000, 0.000000000000000000, -0.000000000000000000 ) ) ;
#41575 = VERTEX_POINT ( 'NONE', #32665 ) ;
#41576 = ADVANCED_FACE ( 'NONE', ( #39368 ), #48184, .T. ) ;
#41577 = CARTESIAN_POINT ( 'NONE',  ( -119.9999999999984652, 17.00000000000000000, 35.00000000000000000 ) ) ;
#41578 = CARTESIAN_POINT ( 'NONE',  ( 193.3040265531851105, -1.750000000000010214, 40.81828755692798438 ) ) ;
#41579 = EDGE_CURVE ( 'NONE', #23455, #15608, #9064, .T. ) ;
#41580 = CARTESIAN_POINT ( 'NONE',  ( 73.30402655318508209, 1.750000000000010658, 120.8182875569279702 ) ) ;
#41581 = ORIENTED_EDGE ( 'NONE', *, *, #37753, .T. ) ;
#41582 = EDGE_CURVE ( 'NONE', #18090, #38070, #17028, .T. ) ;
#41583 = CARTESIAN_POINT ( 'NONE',  ( 48.98697415750968531, 11.03699497439252752, -8.016098858316199838 ) ) ;
#41584 = VECTOR ( 'NONE', #6018, 1000.000000000000000 ) ;
#41585 = VERTEX_POINT ( 'NONE', #4207 ) ;
#41586 = CARTESIAN_POINT ( 'NONE',  ( 71.55402655318505367, -1.025126265847089657, -37.43171244307202272 ) ) ;
#41587 = CARTESIAN_POINT ( 'NONE',  ( -8.445973446814976526, 0.000000000000000000, 42.56828755692802702 ) ) ;
#41588 = FACE_OUTER_BOUND ( 'NONE', #8962, .T. ) ;
#41589 = CARTESIAN_POINT ( 'NONE',  ( -69.99999999999940314, 17.00000000000000000, -54.99999999999999289 ) ) ;
#41590 = EDGE_LOOP ( 'NONE', ( #37077, #18393, #39447, #26490, #10577, #27275, #41114, #3800, #23079, #45530, #34531, #19105, #26207, #40979 ) ) ;
#41591 = ORIENTED_EDGE ( 'NONE', *, *, #32601, .F. ) ;
#41592 = CARTESIAN_POINT ( 'NONE',  ( 35.05402655318504657, 2.143131898507880377E-16, 122.5682875569279702 ) ) ;
#41593 =( BOUNDED_CURVE ( )  B_SPLINE_CURVE ( 3, ( #27843, #8594, #47036, #39146 ),
 .UNSPECIFIED., .F., .F. ) 
 B_SPLINE_CURVE_WITH_KNOTS ( ( 4, 4 ),
 ( 3.141592653589793116, 4.712388980384689674 ),
 .UNSPECIFIED. ) 
 CURVE ( )  GEOMETRIC_REPRESENTATION_ITEM ( )  RATIONAL_B_SPLINE_CURVE ( ( 1.000000000000000000, 0.8047378541243649375, 0.8047378541243649375, 1.000000000000000000 ) ) 
 REPRESENTATION_ITEM ( '' )  );
#41594 = B_SPLINE_CURVE_WITH_KNOTS ( 'NONE', 3,
 ( #29902, #6310, #10901, #21951 ),
 .UNSPECIFIED., .F., .F.,
 ( 4, 4 ),
 ( 0.7998230999345287140, 0.9869080488566185361 ),
 .UNSPECIFIED. ) ;
#41595 = ORIENTED_EDGE ( 'NONE', *, *, #16221, .T. ) ;
#41596 = EDGE_CURVE ( 'NONE', #25400, #13070, #13155, .T. ) ;
#41597 = FACE_OUTER_BOUND ( 'NONE', #37184, .T. ) ;
#41598 = LINE ( 'NONE', #29043, #10063 ) ;
#41599 = EDGE_LOOP ( 'NONE', ( #14832, #5949, #18613, #33838 ) ) ;
#41600 = CARTESIAN_POINT ( 'NONE',  ( 1.553101183265239493, 0.2460239823947285576, 9.927288994922816912 ) ) ;
#41601 =( BOUNDED_CURVE ( )  B_SPLINE_CURVE ( 3, ( #8132, #3486, #35092, #23249 ),
 .UNSPECIFIED., .F., .F. ) 
 B_SPLINE_CURVE_WITH_KNOTS ( ( 4, 4 ),
 ( 0.000000000000000000, 1.570796326794896558 ),
 .UNSPECIFIED. ) 
 CURVE ( )  GEOMETRIC_REPRESENTATION_ITEM ( )  RATIONAL_B_SPLINE_CURVE ( ( 1.000000000000000000, 0.8047378541243649375, 0.8047378541243649375, 1.000000000000000000 ) ) 
 REPRESENTATION_ITEM ( '' )  );
#41602 = FACE_OUTER_BOUND ( 'NONE', #12415, .T. ) ;
#41603 = B_SPLINE_SURFACE_WITH_KNOTS ( 'NONE', 3, 3, ( 
 ( #40196, #2695, #3190, #49844 ),
 ( #2943, #14755, #50104, #45770 ),
 ( #37877, #14242, #37627, #29906 ),
 ( #34523, #46019, #18337, #13989 ) ),
 .UNSPECIFIED., .F., .F., .F.,
 ( 4, 4 ),
 ( 4, 4 ),
 ( 0.000000000000000000, 1.000000000000000000 ),
 ( 0.000000000000000000, 1.000000000000000000 ),
 .UNSPECIFIED. ) ;
#41604 = EDGE_LOOP ( 'NONE', ( #9764, #48430, #26220, #6564 ) ) ;
#41605 = CARTESIAN_POINT ( 'NONE',  ( -125.6708471809678542, -1.749999999999996669, -118.1565861772249661 ) ) ;
#41606 = CYLINDRICAL_SURFACE ( 'NONE', #46221, 1.750000000000015543 ) ;
#41607 = CARTESIAN_POINT ( 'NONE',  ( 210.0000000000000568, 2.143131898507880377E-16, -160.9317124430720298 ) ) ;
#41608 = CARTESIAN_POINT ( 'NONE',  ( 35.05402655318504657, 2.143131898507880377E-16, 82.56828755692798438 ) ) ;
#41609 = ORIENTED_EDGE ( 'NONE', *, *, #27518, .F. ) ;
#41610 = ORIENTED_EDGE ( 'NONE', *, *, #45870, .T. ) ;
#41611 = LINE ( 'NONE', #41361, #27753 ) ;
#41612 = CARTESIAN_POINT ( 'NONE',  ( 339.9999999999999432, 185.0000000000000284, -344.0000000000001137 ) ) ;
#41613 = EDGE_CURVE ( 'NONE', #7107, #40469, #24469, .T. ) ;
#41614 =( BOUNDED_CURVE ( )  B_SPLINE_CURVE ( 3, ( #10617, #21407, #6010, #9864 ),
 .UNSPECIFIED., .F., .F. ) 
 B_SPLINE_CURVE_WITH_KNOTS ( ( 4, 4 ),
 ( 3.141592653589793116, 4.712388980384689674 ),
 .UNSPECIFIED. ) 
 CURVE ( )  GEOMETRIC_REPRESENTATION_ITEM ( )  RATIONAL_B_SPLINE_CURVE ( ( 1.000000000000000000, 0.8047378541243649375, 0.8047378541243649375, 1.000000000000000000 ) ) 
 REPRESENTATION_ITEM ( '' )  );
#41615 = CARTESIAN_POINT ( 'NONE',  ( 0.000000000000000000, -326.6272189349111841, 136.0946745562129649 ) ) ;
#41616 = VERTEX_POINT ( 'NONE', #617 ) ;
#41617 = B_SPLINE_CURVE_WITH_KNOTS ( 'NONE', 3,
 ( #22313, #10511, #30790, #18704 ),
 .UNSPECIFIED., .F., .F.,
 ( 4, 4 ),
 ( 0.003717759948433960009, 0.009855840375009033635 ),
 .UNSPECIFIED. ) ;
#41618 = CARTESIAN_POINT ( 'NONE',  ( 0.2131239213569732782, 1.205185050113728673, 9.966990753365131184 ) ) ;
#41619 = ORIENTED_EDGE ( 'NONE', *, *, #4340, .F. ) ;
#41620 = CARTESIAN_POINT ( 'NONE',  ( 14.49999999999999822, 12.98684210526315930, -19.37312575500900280 ) ) ;
#41621 = CARTESIAN_POINT ( 'NONE',  ( 340.0000000000000568, 172.0000000000000000, 346.9999999999998863 ) ) ;
#41622 = LINE ( 'NONE', #41372, #16840 ) ;
#41623 = AXIS2_PLACEMENT_3D ( 'NONE', #45184, #10069, #25729 ) ;
#41624 = CARTESIAN_POINT ( 'NONE',  ( 151.5540265531850537, 2.143131898507880377E-16, -160.9317124430720298 ) ) ;
#41625 = DIRECTION ( 'NONE',  ( 1.000000000000000000, -1.331116318405244905E-23, -4.755310728521421461E-16 ) ) ;
#41626 = DIRECTION ( 'NONE',  ( -0.000000000000000000, -0.000000000000000000, -1.000000000000000000 ) ) ;
#41627 = EDGE_LOOP ( 'NONE', ( #21660, #3873, #2190, #34808 ) ) ;
#41628 = LINE ( 'NONE', #26235, #40308 ) ;
#41629 = CARTESIAN_POINT ( 'NONE',  ( 168.9999999999999716, -182.9999999999999716, -115.0000000000001279 ) ) ;
#41630 = CARTESIAN_POINT ( 'NONE',  ( 0.9647733827258516692, 1.276878621148359816, 9.919954374050675483 ) ) ;
#41631 = EDGE_CURVE ( 'NONE', #566, #50289, #7207, .T. ) ;
#41632 = CARTESIAN_POINT ( 'NONE',  ( 344.0000000000000000, -174.9999999999999432, 341.9999999999998295 ) ) ;
#41633 = EDGE_CURVE ( 'NONE', #43082, #10600, #43687, .T. ) ;
#41634 = ORIENTED_EDGE ( 'NONE', *, *, #13144, .T. ) ;
#41635 = DIRECTION ( 'NONE',  ( 0.000000000000000000, 0.000000000000000000, -1.000000000000000000 ) ) ;
#41636 = ORIENTED_EDGE ( 'NONE', *, *, #32456, .T. ) ;
#41637 = FACE_OUTER_BOUND ( 'NONE', #46707, .T. ) ;
#41639 = ADVANCED_FACE ( 'NONE', ( #4453 ), #16758, .T. ) ;
#41638 = CARTESIAN_POINT ( 'NONE',  ( 130.0000000000015064, 16.00000000000000000, 35.00000000000000000 ) ) ;
#41640 = EDGE_CURVE ( 'NONE', #23492, #891, #39796, .T. ) ;
#41641 = DIRECTION ( 'NONE',  ( 0.000000000000000000, 0.000000000000000000, 1.000000000000000000 ) ) ;
#41642 = ORIENTED_EDGE ( 'NONE', *, *, #8363, .T. ) ;
#41643 = EDGE_CURVE ( 'NONE', #15451, #17054, #4710, .T. ) ;
#41644 = EDGE_CURVE ( 'NONE', #29991, #38466, #6247, .T. ) ;
#41645 = FACE_OUTER_BOUND ( 'NONE', #16039, .T. ) ;
#41646 = ORIENTED_EDGE ( 'NONE', *, *, #43112, .T. ) ;
#41647 = CARTESIAN_POINT ( 'NONE',  ( -44.94597344681493922, 2.143131898507880377E-16, 39.06828755692798438 ) ) ;
#41648 = DIRECTION ( 'NONE',  ( 0.000000000000000000, 1.000000000000000000, 7.004339610132985974E-48 ) ) ;
#41649 = CYLINDRICAL_SURFACE ( 'NONE', #5358, 1.750000000000008438 ) ;
#41650 = EDGE_CURVE ( 'NONE', #25327, #18872, #43442, .T. ) ;
#41651 = ORIENTED_EDGE ( 'NONE', *, *, #30342, .T. ) ;
#41652 = VERTEX_POINT ( 'NONE', #9802 ) ;
#41653 = CARTESIAN_POINT ( 'NONE',  ( 80.00000000000122213, 16.00000000000000000, 5.000000000000004441 ) ) ;
#41654 = DIRECTION ( 'NONE',  ( 0.000000000000000000, -1.000000000000000000, 0.000000000000000000 ) ) ;
#41655 = VECTOR ( 'NONE', #31483, 1000.000000000000114 ) ;
#41656 = VERTEX_POINT ( 'NONE', #48513 ) ;
#41657 = VERTEX_POINT ( 'NONE', #25213 ) ;
#41658 = CARTESIAN_POINT ( 'NONE',  ( 33.30402655318503946, 1.750000000000010658, -119.1817124430720440 ) ) ;
#41659 = DIRECTION ( 'NONE',  ( 1.000000000000000000, 0.000000000000000000, -0.000000000000000000 ) ) ;
#41660 = CARTESIAN_POINT ( 'NONE',  ( 111.5540265531850679, 0.000000000000000000, 79.06828755692798438 ) ) ;
#41661 =( BOUNDED_CURVE ( )  B_SPLINE_CURVE ( 3, ( #7495, #23125, #23894, #19519 ),
 .UNSPECIFIED., .F., .F. ) 
 B_SPLINE_CURVE_WITH_KNOTS ( ( 4, 4 ),
 ( 4.712388980384689674, 6.283185307179586232 ),
 .UNSPECIFIED. ) 
 CURVE ( )  GEOMETRIC_REPRESENTATION_ITEM ( )  RATIONAL_B_SPLINE_CURVE ( ( 1.000000000000000000, 0.8047378541243649375, 0.8047378541243649375, 1.000000000000000000 ) ) 
 REPRESENTATION_ITEM ( '' )  );
#41662 = EDGE_LOOP ( 'NONE', ( #19307, #28056, #30443, #27131 ) ) ;
#41663 = FACE_OUTER_BOUND ( 'NONE', #11291, .T. ) ;
#41664 = ORIENTED_EDGE ( 'NONE', *, *, #40264, .F. ) ;
#41665 = AXIS2_PLACEMENT_3D ( 'NONE', #45425, #21601, #44919 ) ;
#41666 = CARTESIAN_POINT ( 'NONE',  ( -127.7210997126620242, -1.749999999999996669, -38.15658617722495194 ) ) ;
#41667 = FACE_OUTER_BOUND ( 'NONE', #7598, .T. ) ;
#41668 = ORIENTED_EDGE ( 'NONE', *, *, #39677, .F. ) ;
#41669 = ORIENTED_EDGE ( 'NONE', *, *, #28887, .T. ) ;
#41670 = CARTESIAN_POINT ( 'NONE',  ( 113.3040265531850537, -1.749999999999996891, 160.8182875569279702 ) ) ;
#41671 = CARTESIAN_POINT ( 'NONE',  ( 193.3040265531851105, -1.750000000000009992, 0.8182875569279768335 ) ) ;
#41672 = ORIENTED_EDGE ( 'NONE', *, *, #15529, .F. ) ;
#41673 = CARTESIAN_POINT ( 'NONE',  ( 50.00000000000000000, -50.00000000000000000, 900.0000000000000000 ) ) ;
#41674 = ORIENTED_EDGE ( 'NONE', *, *, #25844, .T. ) ;
#41675 = EDGE_CURVE ( 'NONE', #8483, #31718, #6225, .T. ) ;
#41676 = DIRECTION ( 'NONE',  ( 0.000000000000000000, 0.000000000000000000, -1.000000000000000000 ) ) ;
#41677 = ORIENTED_EDGE ( 'NONE', *, *, #33361, .T. ) ;
#41678 = FACE_OUTER_BOUND ( 'NONE', #3127, .T. ) ;
#41679 = CYLINDRICAL_SURFACE ( 'NONE', #22770, 1.750000000000015543 ) ;
#41680 = CARTESIAN_POINT ( 'NONE',  ( 115.0540265531850395, -1.025126265847081886, -80.93171244307201562 ) ) ;
#41681 = DIRECTION ( 'NONE',  ( 0.000000000000000000, -1.000000000000000000, -3.186989995019654210E-49 ) ) ;
#41682 = DIRECTION ( 'NONE',  ( 0.000000000000000000, 0.000000000000000000, 1.000000000000000000 ) ) ;
#41683 = ORIENTED_EDGE ( 'NONE', *, *, #8751, .F. ) ;
#41684 = FACE_OUTER_BOUND ( 'NONE', #10783, .T. ) ;
#41685 = DIRECTION ( 'NONE',  ( -1.000000000000000000, -0.000000000000000000, -0.000000000000000000 ) ) ;
#41686 = CARTESIAN_POINT ( 'NONE',  ( 339.9999999999999432, 169.0000000000000000, -356.0000000000002274 ) ) ;
#41687 = LINE ( 'NONE', #3176, #27426 ) ;
#41688 = VECTOR ( 'NONE', #30653, 1000.000000000000000 ) ;
#41689 = VECTOR ( 'NONE', #12535, 1000.000000000000000 ) ;
#41690 = FACE_OUTER_BOUND ( 'NONE', #18848, .T. ) ;
#41691 = CARTESIAN_POINT ( 'NONE',  ( 210.0000000000000568, 0.000000000000000000, 160.8182875569279702 ) ) ;
#41692 = EDGE_CURVE ( 'NONE', #37196, #36547, #13401, .T. ) ;
#41693 =( BOUNDED_CURVE ( )  B_SPLINE_CURVE ( 3, ( #49512, #6706, #19002, #7486 ),
 .UNSPECIFIED., .F., .F. ) 
 B_SPLINE_CURVE_WITH_KNOTS ( ( 4, 4 ),
 ( 4.712388980384689674, 6.283185307179586232 ),
 .UNSPECIFIED. ) 
 CURVE ( )  GEOMETRIC_REPRESENTATION_ITEM ( )  RATIONAL_B_SPLINE_CURVE ( ( 1.000000000000000000, 0.8047378541243649375, 0.8047378541243649375, 1.000000000000000000 ) ) 
 REPRESENTATION_ITEM ( '' )  );
#41694 = CARTESIAN_POINT ( 'NONE',  ( -64.99999999999846523, 17.00000000000000000, 60.00000000000000000 ) ) ;
#41695 = AXIS2_PLACEMENT_3D ( 'NONE', #7288, #7552, #50598 ) ;
#41696 = AXIS2_PLACEMENT_3D ( 'NONE', #46099, #6385, #10994 ) ;
#41697 = DIRECTION ( 'NONE',  ( 0.000000000000000000, 0.000000000000000000, 1.000000000000000000 ) ) ;
#41698 = AXIS2_PLACEMENT_3D ( 'NONE', #555, #28247, #43880 ) ;
#41699 = FACE_OUTER_BOUND ( 'NONE', #37395, .T. ) ;
#41700 = EDGE_CURVE ( 'NONE', #218, #23671, #15208, .T. ) ;
#41701 = ADVANCED_FACE ( 'NONE', ( #15115 ), #33185, .F. ) ;
#41702 = EDGE_LOOP ( 'NONE', ( #37831, #13536, #7599, #29863, #3443, #21039 ) ) ;
#41703 = CARTESIAN_POINT ( 'NONE',  ( 11.54386348672365692, 12.18274641659816915, -9.233365092205394475 ) ) ;
#41704 = VECTOR ( 'NONE', #14383, 1000.000000000000000 ) ;
#41705 = CARTESIAN_POINT ( 'NONE',  ( 0.3862712429686894766, -1.188820645368940276, -3.333333333333333481 ) ) ;
#41706 = CARTESIAN_POINT ( 'NONE',  ( -15.73090589902298042, -29.60029367929041655, 1.847720168420772691 ) ) ;
#41707 = EDGE_CURVE ( 'NONE', #6226, #48323, #6460, .T. ) ;
#41708 = CARTESIAN_POINT ( 'NONE',  ( 342.8284271247461561, -167.0000000000001137, -342.0000000000002842 ) ) ;
#41709 = DIRECTION ( 'NONE',  ( 0.000000000000000000, -1.000000000000000000, -0.000000000000000000 ) ) ;
#41710 = ORIENTED_EDGE ( 'NONE', *, *, #42134, .T. ) ;
#41711 = PRODUCT_DEFINITION_SHAPE ( 'NONE', 'NONE',  #8372 ) ;
#41712 = ORIENTED_EDGE ( 'NONE', *, *, #766, .F. ) ;
#41713 = DIRECTION ( 'NONE',  ( -1.000000000000000000, 0.000000000000000000, -2.958228394578794270E-31 ) ) ;
#41714 = DIRECTION ( 'NONE',  ( -0.9928768384869219865, 0.000000000000000000, -0.1191452206184307611 ) ) ;
#41715 = ORIENTED_EDGE ( 'NONE', *, *, #3888, .F. ) ;
#41716 = DIRECTION ( 'NONE',  ( -1.000000000000000000, 0.000000000000000000, 0.000000000000000000 ) ) ;
#41717 = CARTESIAN_POINT ( 'NONE',  ( 193.3040265531851105, -1.750000000000009992, 0.8182875569279768335 ) ) ;
#41718 = VERTEX_POINT ( 'NONE', #25981 ) ;
#41719 = VERTEX_POINT ( 'NONE', #44687 ) ;
#41720 = ORIENTED_EDGE ( 'NONE', *, *, #21834, .T. ) ;
#41721 = B_SPLINE_CURVE_WITH_KNOTS ( 'NONE', 3,
 ( #7008, #22401, #38073, #42652 ),
 .UNSPECIFIED., .F., .F.,
 ( 4, 4 ),
 ( 0.0006664118838822457149, 0.001081796195657078749 ),
 .UNSPECIFIED. ) ;
#41722 = DIRECTION ( 'NONE',  ( 1.000000000000000000, 0.000000000000000000, -1.586032892321651989E-16 ) ) ;
#41723 = CARTESIAN_POINT ( 'NONE',  ( -46.69597344681494633, 1.750000000000010658, 120.8182875569279702 ) ) ;
#41724 = VERTEX_POINT ( 'NONE', #21355 ) ;
#41725 = CIRCLE ( 'NONE', #27824, 2.000000000000001776 ) ;
#41726 = DIRECTION ( 'NONE',  ( 0.000000000000000000, -1.000000000000000000, -3.186989995019654210E-49 ) ) ;
#41727 = FACE_OUTER_BOUND ( 'NONE', #22679, .T. ) ;
#41728 = EDGE_LOOP ( 'NONE', ( #18287, #45250, #49019, #22951, #21334, #11956 ) ) ;
#41729 = ORIENTED_EDGE ( 'NONE', *, *, #5130, .T. ) ;
#41730 = DIRECTION ( 'NONE',  ( 1.000000000000000000, 0.000000000000000000, -0.000000000000000000 ) ) ;
#41731 = COLOUR_RGB ( '',0.7921568627450980005, 0.8196078431372548767, 0.9333333333333333481 ) ;
#41732 = AXIS2_PLACEMENT_3D ( 'NONE', #33316, #13782, #33061 ) ;
#41733 = CARTESIAN_POINT ( 'NONE',  ( -5.670847180967843570, -1.750000000000023315, -40.20683870891912903 ) ) ;
#41734 = CARTESIAN_POINT ( 'NONE',  ( -10.00000000000000355, -34.54492135858216528, 0.000000000000000000 ) ) ;
#41735 = ORIENTED_EDGE ( 'NONE', *, *, #41631, .T. ) ;
#41736 = EDGE_CURVE ( 'NONE', #16113, #11215, #14149, .T. ) ;
#41737 = CARTESIAN_POINT ( 'NONE',  ( -37.52258785160506704, -18.42740426802361142, 8.846626183609803462 ) ) ;
#41738 = DIRECTION ( 'NONE',  ( 0.000000000000000000, 1.000000000000000000, 0.000000000000000000 ) ) ;
#41739 = VECTOR ( 'NONE', #37070, 999.9999999999998863 ) ;
#41740 = DIRECTION ( 'NONE',  ( -1.000000000000000000, 0.000000000000000000, 0.000000000000000000 ) ) ;
#41741 = CARTESIAN_POINT ( 'NONE',  ( 210.0000000000000568, 2.143131898507881116E-16, -40.93171244307203693 ) ) ;
#41742 = ORIENTED_EDGE ( 'NONE', *, *, #38380, .T. ) ;
#41743 = LINE ( 'NONE', #22247, #443 ) ;
#41744 = CARTESIAN_POINT ( 'NONE',  ( -84.94597344681493212, 1.025126265847089657, 42.56828755692799149 ) ) ;
#41745 = DIRECTION ( 'NONE',  ( 0.000000000000000000, 0.000000000000000000, 1.000000000000000000 ) ) ;
#41746 = CYLINDRICAL_SURFACE ( 'NONE', #18679, 1.750000000000015543 ) ;
#41747 =( BOUNDED_CURVE ( )  B_SPLINE_CURVE ( 3, ( #13966, #18313, #14480, #14734 ),
 .UNSPECIFIED., .F., .F. ) 
 B_SPLINE_CURVE_WITH_KNOTS ( ( 4, 4 ),
 ( 4.712388980384689674, 6.283185307179586232 ),
 .UNSPECIFIED. ) 
 CURVE ( )  GEOMETRIC_REPRESENTATION_ITEM ( )  RATIONAL_B_SPLINE_CURVE ( ( 1.000000000000000000, 0.8047378541243649375, 0.8047378541243649375, 1.000000000000000000 ) ) 
 REPRESENTATION_ITEM ( '' )  );
#41748 = CARTESIAN_POINT ( 'NONE',  ( -2.052581215100349521, 0.2042358160481012597, 9.886433018048073507 ) ) ;
#41749 = ORIENTED_EDGE ( 'NONE', *, *, #49764, .F. ) ;
#41750 = CARTESIAN_POINT ( 'NONE',  ( 167.5000000000000000, -112.5000000000000000, 10.00000000000000000 ) ) ;
#41751 =( BOUNDED_CURVE ( )  B_SPLINE_CURVE ( 3, ( #14226, #13974, #10636, #29384 ),
 .UNSPECIFIED., .F., .F. ) 
 B_SPLINE_CURVE_WITH_KNOTS ( ( 4, 4 ),
 ( 3.141592653589793116, 4.712388980384689674 ),
 .UNSPECIFIED. ) 
 CURVE ( )  GEOMETRIC_REPRESENTATION_ITEM ( )  RATIONAL_B_SPLINE_CURVE ( ( 1.000000000000000000, 0.8047378541243649375, 0.8047378541243649375, 1.000000000000000000 ) ) 
 REPRESENTATION_ITEM ( '' )  );
#41752 = CARTESIAN_POINT ( 'NONE',  ( 4.999999999999999112, 175.0000000000000284, 346.2500000000002274 ) ) ;
#41753 = VECTOR ( 'NONE', #25433, 1000.000000000000000 ) ;
#41754 = AXIS2_PLACEMENT_3D ( 'NONE', #36163, #8718, #24366 ) ;
#41755 = ORIENTED_EDGE ( 'NONE', *, *, #39600, .F. ) ;
#41756 = LINE ( 'NONE', #2252, #26202 ) ;
#41757 = ORIENTED_EDGE ( 'NONE', *, *, #45434, .F. ) ;
#41758 = CARTESIAN_POINT ( 'NONE',  ( 129.9999999999999432, 17.00000000000000000, -90.00000000000000000 ) ) ;
#41759 = CARTESIAN_POINT ( 'NONE',  ( 350.0000000000000000, -180.9999999999999716, -356.0000000000002274 ) ) ;
#41760 = EDGE_CURVE ( 'NONE', #43789, #48660, #49267, .T. ) ;
#41761 = FACE_OUTER_BOUND ( 'NONE', #39590, .T. ) ;
#41762 = CARTESIAN_POINT ( 'NONE',  ( 194.9999999999999432, 173.0000000000000000, 352.0000000000000000 ) ) ;
#41763 = ORIENTED_EDGE ( 'NONE', *, *, #27720, .T. ) ;
#41764 = CARTESIAN_POINT ( 'NONE',  ( -8.445973446814976526, 0.000000000000000000, 165.0000000000000000 ) ) ;
#41765 = ORIENTED_EDGE ( 'NONE', *, *, #48093, .T. ) ;
#41766 = ORIENTED_EDGE ( 'NONE', *, *, #22110, .T. ) ;
#41767 = VERTEX_POINT ( 'NONE', #33435 ) ;
#41768 = FACE_OUTER_BOUND ( 'NONE', #5641, .T. ) ;
#41769 = CARTESIAN_POINT ( 'NONE',  ( -33.01266944765060174, 5.813986777101691317, 1.847720168420772691 ) ) ;
#41770 = CARTESIAN_POINT ( 'NONE',  ( 45.21167770612395742, 22.65616271077811206, 7.906207997025717304 ) ) ;
#41771 = EDGE_CURVE ( 'NONE', #17646, #24955, #32934, .T. ) ;
#41772 = CARTESIAN_POINT ( 'NONE',  ( 210.0000000000000568, 2.143131898507881116E-16, 39.06828755692797728 ) ) ;
#41773 = CARTESIAN_POINT ( 'NONE',  ( 33.30402655318503946, 0.000000000000000000, 165.0000000000000000 ) ) ;
#41774 = ORIENTED_EDGE ( 'NONE', *, *, #36242, .T. ) ;
#41775 = EDGE_CURVE ( 'NONE', #46337, #19548, #32770, .T. ) ;
#41776 = LINE ( 'NONE', #26641, #28908 ) ;
#41777 = CARTESIAN_POINT ( 'NONE',  ( 71.55402655318505367, 0.000000000000000000, 119.0682875569279560 ) ) ;
#41778 = FACE_OUTER_BOUND ( 'NONE', #15642, .T. ) ;
#41779 = ORIENTED_EDGE ( 'NONE', *, *, #26240, .T. ) ;
#41780 = DIRECTION ( 'NONE',  ( 6.203854594147707562E-25, -2.067951531382569187E-25, 1.000000000000000000 ) ) ;
#41781 = CARTESIAN_POINT ( 'NONE',  ( 0.9942667885118371407, -0.7728247605419453770, 9.974012008644013605 ) ) ;
#41782 = VERTEX_POINT ( 'NONE', #40620 ) ;
#41783 = ORIENTED_EDGE ( 'NONE', *, *, #10182, .T. ) ;
#41784 = ORIENTED_EDGE ( 'NONE', *, *, #36641, .T. ) ;
#41785 = CARTESIAN_POINT ( 'NONE',  ( -1.212058008859267177, -0.1697297676669723421, 9.966990753365127631 ) ) ;
#41786 = CARTESIAN_POINT ( 'NONE',  ( -206.6959734468149463, -1.750000000000010658, -79.18171244307201562 ) ) ;
#41787 = ADVANCED_FACE ( 'NONE', ( #9565 ), #22118, .F. ) ;
#41788 = VERTEX_POINT ( 'NONE', #2365 ) ;
#41789 = VECTOR ( 'NONE', #50441, 1000.000000000000000 ) ;
#41790 = VECTOR ( 'NONE', #3389, 1000.000000000000000 ) ;
#41791 = CARTESIAN_POINT ( 'NONE',  ( 73.30402655318508209, -1.750000000000010658, 120.8182875569279702 ) ) ;
#41792 = CARTESIAN_POINT ( 'NONE',  ( -582.5000000000000000, 47.50000000000000000, -58.60000000000003695 ) ) ;
#41793 = DIRECTION ( 'NONE',  ( 1.000000000000000000, 0.000000000000000000, 0.000000000000000000 ) ) ;
#41794 = EDGE_CURVE ( 'NONE', #32061, #25893, #48769, .T. ) ;
#41795 = CIRCLE ( 'NONE', #36108, 1.750000000000036193 ) ;
#41796 = CARTESIAN_POINT ( 'NONE',  ( -5.670847180967843570, 1.750000000000023537, 81.84341382277507648 ) ) ;
#41798 = EDGE_LOOP ( 'NONE', ( #16956, #11295, #39198, #25326, #18267, #11168 ) ) ;
#41797 = VECTOR ( 'NONE', #17576, 1000.000000000000000 ) ;
#41799 = CARTESIAN_POINT ( 'NONE',  ( 10.00000000000000000, -250.0000000000000000, -224.9999999999999716 ) ) ;
#41800 = LINE ( 'NONE', #3550, #530 ) ;
#41801 = VECTOR ( 'NONE', #3807, 1000.000000000000000 ) ;
#41802 = AXIS2_PLACEMENT_3D ( 'NONE', #27232, #6964, #23375 ) ;
#41803 = CARTESIAN_POINT ( 'NONE',  ( 0.000000000000000000, 0.000000000000000000, 5.000000000000000000 ) ) ;
#41804 = VERTEX_POINT ( 'NONE', #21610 ) ;
#41806 = CARTESIAN_POINT ( 'NONE',  ( 73.30402655318508209, 1.750000000000010658, -79.18171244307201562 ) ) ;
#41805 = AXIS2_PLACEMENT_3D ( 'NONE', #24871, #40525, #5363 ) ;
#41807 = CARTESIAN_POINT ( 'NONE',  ( -164.9999999999978400, 17.00000000000000000, 95.00000000000000000 ) ) ;
#41808 = DIRECTION ( 'NONE',  ( -0.000000000000000000, -0.000000000000000000, -1.000000000000000000 ) ) ;
#41809 = CARTESIAN_POINT ( 'NONE',  ( 31.55402655318503236, 0.000000000000000000, 165.0000000000000000 ) ) ;
#41810 = ORIENTED_EDGE ( 'NONE', *, *, #20109, .T. ) ;
#41811 = CARTESIAN_POINT ( 'NONE',  ( -1.011271242968688533, 0.7347315653655859258, 3.333333333333333481 ) ) ;
#41812 = B_SPLINE_CURVE_WITH_KNOTS ( 'NONE', 3,
 ( #8128, #4273, #8380, #35591 ),
 .UNSPECIFIED., .F., .F.,
 ( 4, 4 ),
 ( 8.673617379884035472E-19, 0.002466147708923230146 ),
 .UNSPECIFIED. ) ;
#41813 = CARTESIAN_POINT ( 'NONE',  ( 339.9999999999998863, -180.9999999999999716, 355.9999999999997726 ) ) ;
#41814 = LINE ( 'NONE', #26679, #13834 ) ;
#41815 = CARTESIAN_POINT ( 'NONE',  ( -6.174150299305392053, 50.00000000000000711, 8.807470649214879543 ) ) ;
#41816 = EDGE_CURVE ( 'NONE', #25407, #24059, #2123, .T. ) ;
#41817 = LINE ( 'NONE', #18203, #9866 ) ;
#41818 = ORIENTED_EDGE ( 'NONE', *, *, #45236, .T. ) ;
#41819 = EDGE_CURVE ( 'NONE', #29160, #17906, #50493, .T. ) ;
#41820 = CARTESIAN_POINT ( 'NONE',  ( -210.0000000000000568, 2.143131898507876926E-16, -120.9317124430720582 ) ) ;
#41821 = ORIENTED_EDGE ( 'NONE', *, *, #4563, .F. ) ;
#41822 = EDGE_CURVE ( 'NONE', #39034, #13738, #2603, .T. ) ;
#41823 = CARTESIAN_POINT ( 'NONE',  ( -2.462075149652696027, 16.57295996686994499, 9.403735324607438884 ) ) ;
#41824 = ORIENTED_EDGE ( 'NONE', *, *, #3883, .T. ) ;
#41825 = CARTESIAN_POINT ( 'NONE',  ( -84.94597344681493212, -1.025126265847089213, -37.43171244307202272 ) ) ;
#41826 = ADVANCED_FACE ( 'NONE', ( #21105 ), #1621, .T. ) ;
#41827 = CARTESIAN_POINT ( 'NONE',  ( 210.0000000000000568, 0.000000000000000000, 82.56828755692799859 ) ) ;
#41828 = VERTEX_POINT ( 'NONE', #20233 ) ;
#41829 = LINE ( 'NONE', #49732, #26523 ) ;
#41830 = ORIENTED_EDGE ( 'NONE', *, *, #4593, .F. ) ;
#41831 = EDGE_CURVE ( 'NONE', #6173, #1878, #27680, .T. ) ;
#41832 = VECTOR ( 'NONE', #40206, 1000.000000000000000 ) ;
#41833 = AXIS2_PLACEMENT_3D ( 'NONE', #17657, #2255, #38197 ) ;
#41834 = CARTESIAN_POINT ( 'NONE',  ( -1.332485441698227469, 1.351730126698055479, 9.900811091504548855 ) ) ;
#41835 = ORIENTED_EDGE ( 'NONE', *, *, #9110, .F. ) ;
#41836 = CARTESIAN_POINT ( 'NONE',  ( 74.32915281903215998, 1.750000000000010214, -78.15658617722490931 ) ) ;
#41837 = CARTESIAN_POINT ( 'NONE',  ( 0.000000000000000000, 169.0000000000000000, 355.9999999999997726 ) ) ;
#41838 = SHAPE_REPRESENTATION ( 'housing door', ( #45486 ), #9445 ) ;
#41839 = CARTESIAN_POINT ( 'NONE',  ( -45.67084718096785423, -1.750000000000009326, 1.843413822775066269 ) ) ;
#41840 = CARTESIAN_POINT ( 'NONE',  ( 130.0000000000005684, 17.00000000000000000, -30.00000000000000000 ) ) ;
#41841 = LINE ( 'NONE', #2828, #30663 ) ;
#41842 = VECTOR ( 'NONE', #18120, 1000.000000000000000 ) ;
#41843 = EDGE_LOOP ( 'NONE', ( #10546, #20335, #25008, #23487 ) ) ;
#41844 = AXIS2_PLACEMENT_3D ( 'NONE', #31561, #46641, #43585 ) ;
#41845 = EDGE_LOOP ( 'NONE', ( #45291, #197, #47694, #35323 ) ) ;
#41846 = CARTESIAN_POINT ( 'NONE',  ( 0.000000000000000000, 175.0000000000000284, -350.0000000000002274 ) ) ;
#41847 = ORIENTED_EDGE ( 'NONE', *, *, #39399, .F. ) ;
#41848 = DIRECTION ( 'NONE',  ( 0.000000000000000000, 0.000000000000000000, -1.000000000000000000 ) ) ;
#41849 = DIRECTION ( 'NONE',  ( -1.000000000000000000, 0.000000000000000000, -1.612977847700450206E-50 ) ) ;
#41850 = VERTEX_POINT ( 'NONE', #16378 ) ;
#41851 = DIRECTION ( 'NONE',  ( 0.000000000000000000, 0.000000000000000000, -1.000000000000000000 ) ) ;
#41852 = CARTESIAN_POINT ( 'NONE',  ( 166.9999999999999716, -81.49999999999997158, -340.0000000000001137 ) ) ;
#41853 = EDGE_CURVE ( 'NONE', #29317, #22517, #42942, .T. ) ;
#41854 = ORIENTED_EDGE ( 'NONE', *, *, #16741, .T. ) ;
#41855 = EDGE_CURVE ( 'NONE', #34244, #4629, #21967, .T. ) ;
#41856 = CARTESIAN_POINT ( 'NONE',  ( -126.6959734468149321, -1.749999999999997335, -119.1817124430720440 ) ) ;
#41857 = CARTESIAN_POINT ( 'NONE',  ( -127.7210997126620242, -1.749999999999996891, -78.15658617722492352 ) ) ;
#41858 = CARTESIAN_POINT ( 'NONE',  ( 30.00000000000029132, 17.00000000000000000, -84.99999999999998579 ) ) ;
#41859 = LINE ( 'NONE', #7222, #17361 ) ;
#41860 = ADVANCED_FACE ( 'NONE', ( #35903, #42805 ), #11272, .F. ) ;
#41861 = EDGE_CURVE ( 'NONE', #2423, #43021, #13808, .T. ) ;
#41862 = VERTEX_POINT ( 'NONE', #23835 ) ;
#41863 = ORIENTED_EDGE ( 'NONE', *, *, #49039, .T. ) ;
#41864 = EDGE_CURVE ( 'NONE', #36524, #31257, #40738, .T. ) ;
#41865 = SURFACE_STYLE_USAGE ( .BOTH. , #23380 ) ;
#41866 = EDGE_CURVE ( 'NONE', #12977, #30605, #23650, .T. ) ;
#41867 = CARTESIAN_POINT ( 'NONE',  ( 30.25247992116058526, -39.82368563463805344, -3.760136334089591248 ) ) ;
#41868 = VERTEX_POINT ( 'NONE', #11777 ) ;
#41869 = EDGE_LOOP ( 'NONE', ( #32820, #33837, #25413, #4187 ) ) ;
#41870 = DIRECTION ( 'NONE',  ( 1.047444401652940007E-14, 1.000000000000000000, -3.657132581846951845E-29 ) ) ;
#41871 = LINE ( 'NONE', #2852, #49041 ) ;
#41872 = DIRECTION ( 'NONE',  ( -0.000000000000000000, -0.000000000000000000, -1.000000000000000000 ) ) ;
#41873 = CARTESIAN_POINT ( 'NONE',  ( -23.82716369509181575, -44.49195112875988656, 8.356839323120299312 ) ) ;
#41874 = DIRECTION ( 'NONE',  ( -0.000000000000000000, -0.000000000000000000, 1.000000000000000000 ) ) ;
#41875 = DIRECTION ( 'NONE',  ( 0.000000000000000000, 0.000000000000000000, 1.000000000000000000 ) ) ;
#41876 = DIRECTION ( 'NONE',  ( -1.000000000000000000, -0.000000000000000000, -0.000000000000000000 ) ) ;
#41877 = ORIENTED_EDGE ( 'NONE', *, *, #28938, .F. ) ;
#41878 = CARTESIAN_POINT ( 'NONE',  ( 73.30402655318508209, -1.750000000000010214, 40.81828755692798438 ) ) ;
#41880 = VECTOR ( 'NONE', #17591, 1000.000000000000000 ) ;
#41879 = LINE ( 'NONE', #22884, #26114 ) ;
#41881 = CARTESIAN_POINT ( 'NONE',  ( 31.55402655318503236, 0.000000000000000000, -157.4317124430720014 ) ) ;
#41882 = EDGE_CURVE ( 'NONE', #47214, #24636, #13188, .T. ) ;
#41883 = EDGE_CURVE ( 'NONE', #20298, #29366, #31123, .T. ) ;
#41884 = CARTESIAN_POINT ( 'NONE',  ( -69.99999999999847944, 17.00000000000000000, 35.00000000000000000 ) ) ;
#41885 = VERTEX_POINT ( 'NONE', #19971 ) ;
#41886 = EDGE_CURVE ( 'NONE', #45654, #41447, #35659, .T. ) ;
#41887 = DIRECTION ( 'NONE',  ( -0.000000000000000000, -0.000000000000000000, -1.000000000000000000 ) ) ;
#41888 = ORIENTED_EDGE ( 'NONE', *, *, #44950, .T. ) ;
#41889 = CARTESIAN_POINT ( 'NONE',  ( 350.0000000000000000, 165.0000000000000000, -360.0000000000002274 ) ) ;
#41890 = CARTESIAN_POINT ( 'NONE',  ( 210.0000000000000568, 2.143131898507890731E-16, -160.9317124430720298 ) ) ;
#41891 = CARTESIAN_POINT ( 'NONE',  ( 9.260964247899975632, -13.84230907185609460, -9.683996418299976483 ) ) ;
#41892 = ORIENTED_EDGE ( 'NONE', *, *, #20555, .T. ) ;
#41893 =( BOUNDED_CURVE ( )  B_SPLINE_CURVE ( 3, ( #14786, #27617, #22734, #50132 ),
 .UNSPECIFIED., .F., .F. ) 
 B_SPLINE_CURVE_WITH_KNOTS ( ( 4, 4 ),
 ( 0.000000000000000000, 1.570796326794896558 ),
 .UNSPECIFIED. ) 
 CURVE ( )  GEOMETRIC_REPRESENTATION_ITEM ( )  RATIONAL_B_SPLINE_CURVE ( ( 1.000000000000000000, 0.8047378541243649375, 0.8047378541243649375, 1.000000000000000000 ) ) 
 REPRESENTATION_ITEM ( '' )  );
#41894 = FACE_OUTER_BOUND ( 'NONE', #18431, .T. ) ;
#41895 = VERTEX_POINT ( 'NONE', #50469 ) ;
#41896 = LINE ( 'NONE', #19045, #27121 ) ;
#41897 = CARTESIAN_POINT ( 'NONE',  ( 181.0000000000000000, -174.9999999999999716, -360.0000000000001705 ) ) ;
#41898 = CARTESIAN_POINT ( 'NONE',  ( -6.695973446814940111, 1.750000000000023315, 160.8182875569279702 ) ) ;
#41899 = ADVANCED_FACE ( 'NONE', ( #4077 ), #38730, .F. ) ;
#41900 =( BOUNDED_CURVE ( )  B_SPLINE_CURVE ( 3, ( #17017, #33194, #48269, #41377 ),
 .UNSPECIFIED., .F., .F. ) 
 B_SPLINE_CURVE_WITH_KNOTS ( ( 4, 4 ),
 ( 4.712388980384689674, 6.283185307179586232 ),
 .UNSPECIFIED. ) 
 CURVE ( )  GEOMETRIC_REPRESENTATION_ITEM ( )  RATIONAL_B_SPLINE_CURVE ( ( 1.000000000000000000, 0.8047378541243649375, 0.8047378541243649375, 1.000000000000000000 ) ) 
 REPRESENTATION_ITEM ( '' )  );
#41901 = VECTOR ( 'NONE', #9752, 1000.000000000000000 ) ;
#41902 = VERTEX_POINT ( 'NONE', #15620 ) ;
#41903 = ORIENTED_EDGE ( 'NONE', *, *, #8504, .F. ) ;
#41904 = DIRECTION ( 'NONE',  ( -1.000000000000000000, -0.000000000000000000, -0.000000000000000000 ) ) ;
#41905 = CARTESIAN_POINT ( 'NONE',  ( 339.9999999999998863, -168.9999999999999432, 343.9999999999997726 ) ) ;
#41906 = AXIS2_PLACEMENT_3D ( 'NONE', #16891, #28680, #25843 ) ;
#41907 = VERTEX_POINT ( 'NONE', #19463 ) ;
#41908 = EDGE_LOOP ( 'NONE', ( #40808, #25015 ) ) ;
#41909 = LINE ( 'NONE', #6756, #15939 ) ;
#41910 = DIRECTION ( 'NONE',  ( -1.000000000000000000, 0.000000000000000000, 0.000000000000000000 ) ) ;
#41911 = DIRECTION ( 'NONE',  ( 0.000000000000000000, 0.000000000000000000, 1.000000000000000000 ) ) ;
#41912 = EDGE_CURVE ( 'NONE', #8645, #35844, #31547, .T. ) ;
#41913 = VERTEX_POINT ( 'NONE', #27177 ) ;
#41914 = DIRECTION ( 'NONE',  ( 1.000000000000000000, 0.000000000000000000, -0.000000000000000000 ) ) ;
#41915 = ORIENTED_EDGE ( 'NONE', *, *, #17102, .T. ) ;
#41916 =( BOUNDED_CURVE ( )  B_SPLINE_CURVE ( 3, ( #33181, #49003, #13889, #6220 ),
 .UNSPECIFIED., .F., .F. ) 
 B_SPLINE_CURVE_WITH_KNOTS ( ( 4, 4 ),
 ( 3.141592653589793116, 4.712388980384689674 ),
 .UNSPECIFIED. ) 
 CURVE ( )  GEOMETRIC_REPRESENTATION_ITEM ( )  RATIONAL_B_SPLINE_CURVE ( ( 1.000000000000000000, 0.8047378541243649375, 0.8047378541243649375, 1.000000000000000000 ) ) 
 REPRESENTATION_ITEM ( '' )  );
#41917 = CARTESIAN_POINT ( 'NONE',  ( -10.01251772323708700, 8.486842105263161073, 18.46084505325461578 ) ) ;
#41918 = CARTESIAN_POINT ( 'NONE',  ( 181.0000000000000284, -272.5000000000000000, -112.9999999999999005 ) ) ;
#41919 = ADVANCED_FACE ( 'NONE', ( #46880 ), #32553, .F. ) ;
#41921 = ORIENTED_EDGE ( 'NONE', *, *, #27708, .T. ) ;
#41920 = EDGE_CURVE ( 'NONE', #1975, #14871, #4816, .T. ) ;
#41922 = ORIENTED_EDGE ( 'NONE', *, *, #20221, .F. ) ;
#41923 = ORIENTED_EDGE ( 'NONE', *, *, #16757, .F. ) ;
#41924 = CARTESIAN_POINT ( 'NONE',  ( -4.207128120815918256E-14, 3.058192377181588826E-14, 10.00000000000000000 ) ) ;
#41925 = CARTESIAN_POINT ( 'NONE',  ( 155.0540265531850537, 2.143131898507880377E-16, -0.9317124430720247208 ) ) ;
#41926 = EDGE_CURVE ( 'NONE', #19760, #9972, #40593, .T. ) ;
#41927 = VERTEX_POINT ( 'NONE', #47889 ) ;
#41928 = PLANE ( 'NONE',  #4295 ) ;
#41929 = ORIENTED_EDGE ( 'NONE', *, *, #25848, .T. ) ;
#41930 = EDGE_CURVE ( 'NONE', #42224, #46895, #22268, .T. ) ;
#41931 = FACE_OUTER_BOUND ( 'NONE', #29794, .T. ) ;
#41932 = CARTESIAN_POINT ( 'NONE',  ( 210.0000000000000568, 2.143131898507880377E-16, -0.9317124430720331585 ) ) ;
#41933 = ORIENTED_EDGE ( 'NONE', *, *, #40649, .F. ) ;
#41934 = EDGE_CURVE ( 'NONE', #26648, #7228, #40747, .T. ) ;
#41935 = DIRECTION ( 'NONE',  ( -0.000000000000000000, -1.000000000000000000, -0.000000000000000000 ) ) ;
#41936 = CARTESIAN_POINT ( 'NONE',  ( -86.69597344681496054, 0.000000000000000000, 165.0000000000000000 ) ) ;
#41937 = FACE_OUTER_BOUND ( 'NONE', #50056, .T. ) ;
#41938 = FACE_OUTER_BOUND ( 'NONE', #33530, .T. ) ;
#41939 = CARTESIAN_POINT ( 'NONE',  ( -8.760073316077685135, -222.4999999999999716, -228.6347188485896140 ) ) ;
#41940 = EDGE_LOOP ( 'NONE', ( #24925, #28857, #34548, #16361 ) ) ;
#41941 = CARTESIAN_POINT ( 'NONE',  ( -206.6959734468149463, 1.750000000000010214, 40.81828755692798438 ) ) ;
#41942 = VECTOR ( 'NONE', #18243, 1000.000000000000000 ) ;
#41943 = CARTESIAN_POINT ( 'NONE',  ( -69.99999999999909051, 16.00000000000000000, 0.000000000000000000 ) ) ;
#41944 = EDGE_CURVE ( 'NONE', #35096, #4194, #31601, .T. ) ;
#41945 = DIRECTION ( 'NONE',  ( 0.000000000000000000, 0.000000000000000000, 1.000000000000000000 ) ) ;
#41946 = CARTESIAN_POINT ( 'NONE',  ( 181.0000000000000000, 6.000000000000060396, -350.0000000000001705 ) ) ;
#41947 = CARTESIAN_POINT ( 'NONE',  ( -4.207128120815918256E-14, 3.058192377181588826E-14, 10.00000000000000000 ) ) ;
#41948 = CARTESIAN_POINT ( 'NONE',  ( 164.9999999999999716, -81.49999999999998579, -340.0000000000001137 ) ) ;
#41949 = CARTESIAN_POINT ( 'NONE',  ( 35.05402655318504657, 2.143131898507880377E-16, -80.93171244307204404 ) ) ;
#41950 = LINE ( 'NONE', #10401, #27 ) ;
#41951 = CARTESIAN_POINT ( 'NONE',  ( -168.4459734468149463, 0.000000000000000000, 122.5682875569279702 ) ) ;
#41952 = VERTEX_POINT ( 'NONE', #24843 ) ;
#41953 = DIRECTION ( 'NONE',  ( -1.000000000000000000, 0.000000000000000000, 0.000000000000000000 ) ) ;
#41954 = FACE_OUTER_BOUND ( 'NONE', #47907, .T. ) ;
#41955 = CARTESIAN_POINT ( 'NONE',  ( 0.2459519479918564622, 1.553112592394157110, 9.927288994922816912 ) ) ;
#41956 = CARTESIAN_POINT ( 'NONE',  ( 10.70590866674922204, -12.76446523155706814, -3.546734833711462365 ) ) ;
#41957 = LINE ( 'NONE', #3968, #43006 ) ;
#41958 = B_SPLINE_CURVE_WITH_KNOTS ( 'NONE', 3,
 ( #26866, #42503, #23005, #3497 ),
 .UNSPECIFIED., .F., .F.,
 ( 4, 4 ),
 ( 0.001152428489661398714, 0.001623376834730018555 ),
 .UNSPECIFIED. ) ;
#41959 = ORIENTED_EDGE ( 'NONE', *, *, #15123, .T. ) ;
#41960 = ORIENTED_EDGE ( 'NONE', *, *, #44584, .T. ) ;
#41961 = CARTESIAN_POINT ( 'NONE',  ( 349.9999999999999432, -168.9999999999999432, 359.9999999999997726 ) ) ;
#41962 = EDGE_CURVE ( 'NONE', #1551, #20787, #47636, .T. ) ;
#41963 = DIRECTION ( 'NONE',  ( 0.000000000000000000, 1.000000000000000000, 0.000000000000000000 ) ) ;
#41964 = ORIENTED_EDGE ( 'NONE', *, *, #3857, .T. ) ;
#41965 = FACE_OUTER_BOUND ( 'NONE', #19037, .T. ) ;
#41966 = PLANE ( 'NONE',  #34783 ) ;
#41967 = CARTESIAN_POINT ( 'NONE',  ( 344.0000000000000568, 167.0000000000000000, 341.9999999999998295 ) ) ;
#41968 = COLOUR_RGB ( '',0.7921568627450980005, 0.8196078431372548767, 0.9333333333333333481 ) ;
#41969 = ORIENTED_EDGE ( 'NONE', *, *, #41831, .T. ) ;
#41970 = ORIENTED_EDGE ( 'NONE', *, *, #47028, .F. ) ;
#41971 = ORIENTED_EDGE ( 'NONE', *, *, #49451, .T. ) ;
#41972 = CARTESIAN_POINT ( 'NONE',  ( -1.222012661920452326, 0.2471648704738776681, 9.981352469109934233 ) ) ;
#41973 = LINE ( 'NONE', #3988, #23435 ) ;
#41974 = DIRECTION ( 'NONE',  ( -4.996003610813203446E-16, -1.000000000000000000, 0.000000000000000000 ) ) ;
#41975 = ORIENTED_EDGE ( 'NONE', *, *, #44048, .F. ) ;
#41976 = ADVANCED_FACE ( 'NONE', ( #20731 ), #36150, .F. ) ;
#41977 = LINE ( 'NONE', #26585, #7944 ) ;
#41978 = ADVANCED_FACE ( 'NONE', ( #44067 ), #32299, .F. ) ;
#41979 = CIRCLE ( 'NONE', #14955, 2.000000000000001776 ) ;
#41980 = CYLINDRICAL_SURFACE ( 'NONE', #7521, 1.750000000000015543 ) ;
#41981 = CARTESIAN_POINT ( 'NONE',  ( 355.9999999999999432, -174.9999999999999432, 357.9999999999998295 ) ) ;
#41982 = ORIENTED_EDGE ( 'NONE', *, *, #1170, .F. ) ;
#41983 = ORIENTED_EDGE ( 'NONE', *, *, #47852, .T. ) ;
#41984 = CARTESIAN_POINT ( 'NONE',  ( 0.000000000000000000, 17.00000000000000000, 0.000000000000000000 ) ) ;
#41985 = DIRECTION ( 'NONE',  ( -0.000000000000000000, -0.000000000000000000, -1.000000000000000000 ) ) ;
#41986 = DIRECTION ( 'NONE',  ( 1.000000000000000000, 6.938893903907233308E-16, 0.000000000000000000 ) ) ;
#41987 = EDGE_CURVE ( 'NONE', #33640, #25713, #15388, .T. ) ;
#41988 = ORIENTED_EDGE ( 'NONE', *, *, #9185, .F. ) ;
#41989 = ORIENTED_EDGE ( 'NONE', *, *, #35302, .T. ) ;
#41990 = ADVANCED_FACE ( 'NONE', ( #24352 ), #9687, .T. ) ;
#41991 = CARTESIAN_POINT ( 'NONE',  ( 191.5540265531851105, 0.000000000000000000, 42.56828755692798438 ) ) ;
#41992 = CYLINDRICAL_SURFACE ( 'NONE', #46029, 2.000000000000001776 ) ;
#41993 = EDGE_CURVE ( 'NONE', #33082, #31856, #12522, .T. ) ;
#41994 = CARTESIAN_POINT ( 'NONE',  ( 181.0000000000000284, -9.999999999999953815, -111.0000000000001563 ) ) ;
#41995 = CARTESIAN_POINT ( 'NONE',  ( -84.94597344681494633, 2.143131898507880377E-16, 165.0000000000000000 ) ) ;
#41996 = CARTESIAN_POINT ( 'NONE',  ( 210.0000000000000568, 0.000000000000000000, -157.4317124430720298 ) ) ;
#41997 = EDGE_LOOP ( 'NONE', ( #38001, #23860, #44846, #22434, #12194, #6577, #48427, #23091, #34739, #4846, #8415, #1613, #15906, #38309 ) ) ;
#41999 = ADVANCED_FACE ( 'NONE', ( #21480 ), #17138, .F. ) ;
#41998 = CARTESIAN_POINT ( 'NONE',  ( 195.0540265531851105, 2.143131898507880377E-16, -157.4317124430720582 ) ) ;
#42000 = FACE_OUTER_BOUND ( 'NONE', #15589, .T. ) ;
#42001 = CARTESIAN_POINT ( 'NONE',  ( -48.44597344681496054, 1.025126265847089435, -117.4317124430720156 ) ) ;
#42002 = DIRECTION ( 'NONE',  ( -1.000000000000000000, -0.000000000000000000, -0.000000000000000000 ) ) ;
#42003 = FACE_OUTER_BOUND ( 'NONE', #4908, .T. ) ;
#42004 = FACE_OUTER_BOUND ( 'NONE', #3451, .T. ) ;
#42005 = ORIENTED_EDGE ( 'NONE', *, *, #4896, .T. ) ;
#42006 = CARTESIAN_POINT ( 'NONE',  ( 232.4999999999999716, -169.9999999999999716, 444.9999999999998295 ) ) ;
#42007 = VECTOR ( 'NONE', #50470, 1000.000000000000000 ) ;
#42008 = LINE ( 'NONE', #9949, #36528 ) ;
#42009 = DIRECTION ( 'NONE',  ( -1.000000000000000000, 0.000000000000000000, 0.000000000000000000 ) ) ;
#42010 = ORIENTED_EDGE ( 'NONE', *, *, #50388, .T. ) ;
#42011 = CYLINDRICAL_SURFACE ( 'NONE', #46108, 1.749999999999973799 ) ;
#42012 = AXIS2_PLACEMENT_3D ( 'NONE', #2611, #26983, #34446 ) ;
#42013 = DIRECTION ( 'NONE',  ( 0.000000000000000000, 0.000000000000000000, 1.000000000000000000 ) ) ;
#42014 = ORIENTED_EDGE ( 'NONE', *, *, #5204, .T. ) ;
#42015 = CARTESIAN_POINT ( 'NONE',  ( 33.30402655318503946, 0.000000000000000000, 165.0000000000000000 ) ) ;
#42016 = CARTESIAN_POINT ( 'NONE',  ( 177.5000000000000284, 102.5000000000000142, 10.00000000000000000 ) ) ;
#42017 = EDGE_CURVE ( 'NONE', #24878, #32976, #44816, .T. ) ;
#42018 = ORIENTED_EDGE ( 'NONE', *, *, #17139, .T. ) ;
#42019 = CARTESIAN_POINT ( 'NONE',  ( -6.880036658038815922, -222.4999999999999716, -228.6347188485896140 ) ) ;
#42020 = EDGE_LOOP ( 'NONE', ( #23207, #28464, #25803, #19287 ) ) ;
#42021 = EDGE_LOOP ( 'NONE', ( #37491, #14167, #50024, #41157 ) ) ;
#42022 = ADVANCED_FACE ( 'NONE', ( #44549 ), #991, .F. ) ;
#42023 = CARTESIAN_POINT ( 'NONE',  ( -88.44597344681494633, -1.025126265847089657, -37.43171244307202272 ) ) ;
#42024 = ORIENTED_EDGE ( 'NONE', *, *, #12993, .T. ) ;
#42025 = DIRECTION ( 'NONE',  ( -1.000000000000000000, 0.000000000000000000, -7.793956916774525800E-48 ) ) ;
#42026 = CARTESIAN_POINT ( 'NONE',  ( -14.99999999999970868, 17.00000000000000000, -84.99999999999998579 ) ) ;
#42027 = CARTESIAN_POINT ( 'NONE',  ( -25.79500241909648395, -7.388441598285492518, 230.0000000000000000 ) ) ;
#42028 = CYLINDRICAL_SURFACE ( 'NONE', #17387, 4.000000000000003553 ) ;
#42029 = B_SPLINE_CURVE_WITH_KNOTS ( 'NONE', 3,
 ( #44605, #25910, #9734, #36976 ),
 .UNSPECIFIED., .F., .F.,
 ( 4, 4 ),
 ( 0.000000000000000000, 2.804146970186932266E-05 ),
 .UNSPECIFIED. ) ;
#42030 = CARTESIAN_POINT ( 'NONE',  ( 135.0000000000021600, 17.00000000000000000, 95.00000000000000000 ) ) ;
#42031 = ORIENTED_EDGE ( 'NONE', *, *, #11182, .T. ) ;
#42032 = DIRECTION ( 'NONE',  ( 0.000000000000000000, 1.000000000000000000, 3.186989995019654210E-49 ) ) ;
#42033 = CARTESIAN_POINT ( 'NONE',  ( -127.7210997126620242, -1.749999999999996669, -158.1565861772249377 ) ) ;
#42034 = CARTESIAN_POINT ( 'NONE',  ( 29.99999999999998579, 16.00000000000000000, -90.00000000000000000 ) ) ;
#42035 = ORIENTED_EDGE ( 'NONE', *, *, #9441, .F. ) ;
#42036 = CARTESIAN_POINT ( 'NONE',  ( 358.0000000000001137, 169.0000000000000000, 343.9999999999998863 ) ) ;
#42037 = CARTESIAN_POINT ( 'NONE',  ( 339.9999999999999432, 169.0000000000000000, -344.0000000000001705 ) ) ;
#42038 = VECTOR ( 'NONE', #34021, 1000.000000000000000 ) ;
#42039 = ORIENTED_EDGE ( 'NONE', *, *, #10646, .F. ) ;
#42040 = ORIENTED_EDGE ( 'NONE', *, *, #49933, .T. ) ;
#42041 = ORIENTED_EDGE ( 'NONE', *, *, #27062, .T. ) ;
#42042 = LINE ( 'NONE', #6899, #45067 ) ;
#42043 = PLANE ( 'NONE',  #20106 ) ;
#42044 = EDGE_LOOP ( 'NONE', ( #35557, #4546, #38057, #38513, #2305, #20127 ) ) ;
#42045 = VECTOR ( 'NONE', #36107, 1000.000000000000000 ) ;
#42046 = CARTESIAN_POINT ( 'NONE',  ( 185.0000000000000000, -268.5000000000000000, -114.9999999999999289 ) ) ;
#42047 = FACE_BOUND ( 'NONE', #45492, .T. ) ;
#42048 = PLANE ( 'NONE',  #37475 ) ;
#42049 = LINE ( 'NONE', #14857, #39472 ) ;
#42050 = AXIS2_PLACEMENT_3D ( 'NONE', #42317, #19208, #29763 ) ;
#42051 = LINE ( 'NONE', #3548, #23365 ) ;
#42053 = EDGE_CURVE ( 'NONE', #41350, #41145, #16054, .T. ) ;
#42052 = DIRECTION ( 'NONE',  ( -1.000000000000000000, -0.000000000000000000, -0.000000000000000000 ) ) ;
#42054 =( BOUNDED_CURVE ( )  B_SPLINE_CURVE ( 3, ( #47600, #36368, #8890, #20429 ),
 .UNSPECIFIED., .F., .F. ) 
 B_SPLINE_CURVE_WITH_KNOTS ( ( 4, 4 ),
 ( 1.570796326794896558, 3.141592653589793116 ),
 .UNSPECIFIED. ) 
 CURVE ( )  GEOMETRIC_REPRESENTATION_ITEM ( )  RATIONAL_B_SPLINE_CURVE ( ( 1.000000000000000000, 0.8047378541243649375, 0.8047378541243649375, 1.000000000000000000 ) ) 
 REPRESENTATION_ITEM ( '' )  );
#42055 = CARTESIAN_POINT ( 'NONE',  ( -164.9999999999984936, 17.00000000000000000, 60.00000000000000000 ) ) ;
#42056 = EDGE_LOOP ( 'NONE', ( #28754, #33822, #14641, #23635 ) ) ;
#42057 = CARTESIAN_POINT ( 'NONE',  ( -37.50000000000000000, 0.000000000000000000, 10.00000000000000000 ) ) ;
#42058 = CARTESIAN_POINT ( 'NONE',  ( 15.80799809827373004, -29.65358618225706522, -8.016098858316199838 ) ) ;
#42059 = CARTESIAN_POINT ( 'NONE',  ( 85.00000000000184741, 17.00000000000000000, 65.00000000000000000 ) ) ;
#42060 = CARTESIAN_POINT ( 'NONE',  ( 224.9999999999999716, -164.9999999999999716, 444.9999999999998295 ) ) ;
#42061 = ORIENTED_EDGE ( 'NONE', *, *, #23022, .F. ) ;
#42062 = LINE ( 'NONE', #2805, #9156 ) ;
#42063 = CARTESIAN_POINT ( 'NONE',  ( -24.34206871062976063, -28.53454467304741371, -9.011255500499645521 ) ) ;
#42064 = DIRECTION ( 'NONE',  ( -6.765175596986472868E-16, 0.9749645535258953943, 0.2223603367690637489 ) ) ;
#42065 = PLANE ( 'NONE',  #17596 ) ;
#42066 = ORIENTED_EDGE ( 'NONE', *, *, #48951, .T. ) ;
#42067 = ORIENTED_EDGE ( 'NONE', *, *, #45859, .F. ) ;
#42068 = CARTESIAN_POINT ( 'NONE',  ( -126.6959734468149321, -1.749999999999997335, -119.1817124430720440 ) ) ;
#42069 = ORIENTED_EDGE ( 'NONE', *, *, #12300, .T. ) ;
#42070 = CARTESIAN_POINT ( 'NONE',  ( 339.9999999999998295, -183.3431457505078015, -358.3431457505079152 ) ) ;
#42071 = AXIS2_PLACEMENT_3D ( 'NONE', #36155, #44074, #12529 ) ;
#42072 = DIRECTION ( 'NONE',  ( -1.000000000000000000, 0.000000000000000000, 0.000000000000000000 ) ) ;
#42073 = ORIENTED_EDGE ( 'NONE', *, *, #30574, .F. ) ;
#42074 = VERTEX_POINT ( 'NONE', #6090 ) ;
#42075 = VECTOR ( 'NONE', #34399, 1000.000000000000000 ) ;
#42076 = CARTESIAN_POINT ( 'NONE',  ( 33.30402655318503946, -1.750000000000010214, 40.81828755692798438 ) ) ;
#42077 = VERTEX_POINT ( 'NONE', #22497 ) ;
#42078 = DIRECTION ( 'NONE',  ( -0.1671032855531354999, 0.5142910309547730208, -0.8411784753765541023 ) ) ;
#42079 = CARTESIAN_POINT ( 'NONE',  ( -581.3085477938157055, -62.49999999999998579, -68.52876838486925237 ) ) ;
#42080 = ORIENTED_EDGE ( 'NONE', *, *, #41920, .T. ) ;
#42081 = FACE_OUTER_BOUND ( 'NONE', #27640, .T. ) ;
#42082 = DIRECTION ( 'NONE',  ( 3.172065745548403743E-16, 1.000000000000000000, 0.000000000000000000 ) ) ;
#42083 = DIRECTION ( 'NONE',  ( -1.000000000000000000, -0.000000000000000000, -0.000000000000000000 ) ) ;
#42084 = VERTEX_POINT ( 'NONE', #48888 ) ;
#42085 = ORIENTED_EDGE ( 'NONE', *, *, #35416, .F. ) ;
#42086 = CARTESIAN_POINT ( 'NONE',  ( 181.0000000000000000, -272.4999999999999432, -357.9999999999999432 ) ) ;
#42087 = CARTESIAN_POINT ( 'NONE',  ( -0.6215990105957072132, 1.608617984725374983, 9.928159647716134018 ) ) ;
#42088 = AXIS2_PLACEMENT_3D ( 'NONE', #8370, #28366, #44489 ) ;
#42089 = ORIENTED_EDGE ( 'NONE', *, *, #48665, .T. ) ;
#42090 = CARTESIAN_POINT ( 'NONE',  ( 185.0000000000000000, -272.5000000000000000, -111.0000000000001563 ) ) ;
#42091 = DIRECTION ( 'NONE',  ( -1.000000000000000000, 0.000000000000000000, 0.000000000000000000 ) ) ;
#42092 = VERTEX_POINT ( 'NONE', #41495 ) ;
#42093 = CARTESIAN_POINT ( 'NONE',  ( -206.6959734468149463, 1.750000000000010658, -79.18171244307201562 ) ) ;
#42094 = VERTEX_POINT ( 'NONE', #14798 ) ;
#42095 = CARTESIAN_POINT ( 'NONE',  ( 165.0000000000000000, 6.000000000000060396, 339.9999999999998863 ) ) ;
#42096 = CARTESIAN_POINT ( 'NONE',  ( 0.3370904143228924954, 0.2449105217885333141, 10.00000000000000000 ) ) ;
#42097 = PLANE ( 'NONE',  #41802 ) ;
#42098 = DIRECTION ( 'NONE',  ( -0.000000000000000000, -0.000000000000000000, -1.000000000000000000 ) ) ;
#42099 = VECTOR ( 'NONE', #10535, 1000.000000000000000 ) ;
#42100 = ORIENTED_EDGE ( 'NONE', *, *, #10879, .F. ) ;
#42101 = CARTESIAN_POINT ( 'NONE',  ( -1.647520908219852975, 0.4432416309288251810, 9.912102921405043787 ) ) ;
#42103 = EDGE_CURVE ( 'NONE', #29723, #13307, #45310, .T. ) ;
#42102 = CARTESIAN_POINT ( 'NONE',  ( -12.97493236725075683, 11.05939663307000664, 8.953103998512858652 ) ) ;
#42104 = AXIS2_PLACEMENT_3D ( 'NONE', #18058, #40914, #49315 ) ;
#42105 = DIRECTION ( 'NONE',  ( -1.000000000000000000, -0.000000000000000000, 0.000000000000000000 ) ) ;
#42106 = ORIENTED_EDGE ( 'NONE', *, *, #47342, .F. ) ;
#42107 = AXIS2_PLACEMENT_3D ( 'NONE', #34327, #30475, #29977 ) ;
#42108 = EDGE_CURVE ( 'NONE', #13712, #8918, #37419, .T. ) ;
#42109 = ORIENTED_EDGE ( 'NONE', *, *, #35720, .F. ) ;
#42110 = EDGE_CURVE ( 'NONE', #31887, #27106, #18633, .T. ) ;
#42111 = CYLINDRICAL_SURFACE ( 'NONE', #23684, 1.749999999999973799 ) ;
#42112 = PLANE ( 'NONE',  #38375 ) ;
#42113 = LINE ( 'NONE', #26474, #11935 ) ;
#42114 = LINE ( 'NONE', #15186, #50371 ) ;
#42115 = CARTESIAN_POINT ( 'NONE',  ( -14.49999999999999822, 13.48684210526315930, 20.00000000000000000 ) ) ;
#42116 = FACE_OUTER_BOUND ( 'NONE', #11071, .T. ) ;
#42117 = ORIENTED_EDGE ( 'NONE', *, *, #17390, .F. ) ;
#42118 = LINE ( 'NONE', #26482, #14917 ) ;
#42119 = EDGE_CURVE ( 'NONE', #7169, #34395, #45807, .T. ) ;
#42120 = B_SPLINE_SURFACE_WITH_KNOTS ( 'NONE', 3, 3, ( 
 ( #20540, #20289, #20036, #35959 ),
 ( #15678, #16447, #12579, #27987 ),
 ( #1048, #28500, #8998, #44124 ),
 ( #24655, #35721, #31349, #46940 ) ),
 .UNSPECIFIED., .F., .F., .F.,
 ( 4, 4 ),
 ( 4, 4 ),
 ( 0.000000000000000000, 1.000000000000000000 ),
 ( 0.000000000000000000, 1.000000000000000000 ),
 .UNSPECIFIED. ) ;
#42121 = CARTESIAN_POINT ( 'NONE',  ( 1.377636575563020438, -0.6021164824561170414, 9.953784399990622589 ) ) ;
#42122 = CARTESIAN_POINT ( 'NONE',  ( -168.4459734468149463, 0.000000000000000000, -77.43171244307204404 ) ) ;
#42123 = EDGE_CURVE ( 'NONE', #3878, #44684, #29464, .T. ) ;
#42124 = ORIENTED_EDGE ( 'NONE', *, *, #1188, .F. ) ;
#42125 = LINE ( 'NONE', #30863, #11439 ) ;
#42126 = ORIENTED_EDGE ( 'NONE', *, *, #12042, .T. ) ;
#42127 = CARTESIAN_POINT ( 'NONE',  ( -10.49999999999999467, -46.01315789473684248, -6.315789473684215949 ) ) ;
#42128 = DIRECTION ( 'NONE',  ( 1.000000000000000000, 0.000000000000000000, 0.000000000000000000 ) ) ;
#42129 = EDGE_CURVE ( 'NONE', #24997, #42678, #29689, .T. ) ;
#42130 = LINE ( 'NONE', #22641, #6673 ) ;
#42131 = EDGE_CURVE ( 'NONE', #41850, #5763, #25567, .T. ) ;
#42132 = ORIENTED_EDGE ( 'NONE', *, *, #28133, .T. ) ;
#42133 = EDGE_CURVE ( 'NONE', #19097, #26042, #14285, .T. ) ;
#42134 = EDGE_CURVE ( 'NONE', #13983, #18505, #38023, .T. ) ;
#42135 = LINE ( 'NONE', #38062, #1666 ) ;
#42136 = ORIENTED_EDGE ( 'NONE', *, *, #48777, .F. ) ;
#42137 = CARTESIAN_POINT ( 'NONE',  ( 47.22310614333766665, 16.46562252335956344, -3.760136334089591248 ) ) ;
#42138 = AXIS2_PLACEMENT_3D ( 'NONE', #35764, #25638, #847 ) ;
#42139 = CARTESIAN_POINT ( 'NONE',  ( 355.9999999999998863, -165.0000000000001137, -108.0000000000002132 ) ) ;
#42140 = ADVANCED_FACE ( 'NONE', ( #42000 ), #10443, .F. ) ;
#42141 = CARTESIAN_POINT ( 'NONE',  ( -126.6959734468149321, -1.749999999999996891, 0.8182875569279768335 ) ) ;
#42142 = VECTOR ( 'NONE', #22640, 1000.000000000000000 ) ;
#42143 = EDGE_CURVE ( 'NONE', #23855, #39145, #49648, .T. ) ;
#42144 = ORIENTED_EDGE ( 'NONE', *, *, #22554, .T. ) ;
#42145 = ORIENTED_EDGE ( 'NONE', *, *, #5791, .F. ) ;
#42146 = FACE_OUTER_BOUND ( 'NONE', #39486, .T. ) ;
#42147 = VECTOR ( 'NONE', #29053, 1000.000000000000000 ) ;
#42148 = DIRECTION ( 'NONE',  ( -0.000000000000000000, -6.123233995736766036E-17, 1.000000000000000000 ) ) ;
#42149 = ORIENTED_EDGE ( 'NONE', *, *, #19283, .F. ) ;
#42150 = ORIENTED_EDGE ( 'NONE', *, *, #36864, .T. ) ;
#42151 = DIRECTION ( 'NONE',  ( -0.000000000000000000, -0.000000000000000000, 1.000000000000000000 ) ) ;
#42152 = DIRECTION ( 'NONE',  ( 0.000000000000000000, 0.000000000000000000, 1.000000000000000000 ) ) ;
#42153 = LINE ( 'NONE', #11631, #1828 ) ;
#42154 = ORIENTED_EDGE ( 'NONE', *, *, #25813, .T. ) ;
#42155 = CYLINDRICAL_SURFACE ( 'NONE', #46410, 1.750000000000001554 ) ;
#42156 = EDGE_LOOP ( 'NONE', ( #49600, #15230, #23211, #35574 ) ) ;
#42157 = LINE ( 'NONE', #42407, #4199 ) ;
#42158 = EDGE_CURVE ( 'NONE', #32209, #17157, #46333, .T. ) ;
#42159 = CARTESIAN_POINT ( 'NONE',  ( -168.4459734468149463, 0.000000000000000000, -80.93171244307201562 ) ) ;
#42160 = CARTESIAN_POINT ( 'NONE',  ( 152.2789002873379900, 1.750000000000010436, -80.20683870891910772 ) ) ;
#42161 = VECTOR ( 'NONE', #2435, 1000.000000000000000 ) ;
#42162 = ADVANCED_FACE ( 'NONE', ( #17637 ), #21621, .T. ) ;
#42163 = ORIENTED_EDGE ( 'NONE', *, *, #7993, .T. ) ;
#42164 = EDGE_CURVE ( 'NONE', #39568, #42500, #12219, .T. ) ;
#42165 = ORIENTED_EDGE ( 'NONE', *, *, #40813, .F. ) ;
#42166 = VERTEX_POINT ( 'NONE', #47329 ) ;
#42167 = AXIS2_PLACEMENT_3D ( 'NONE', #39312, #8257, #35470 ) ;
#42168 =( NAMED_UNIT ( * ) SI_UNIT ( $, .STERADIAN. ) SOLID_ANGLE_UNIT ( ) );
#42169 = CARTESIAN_POINT ( 'NONE',  ( -0.1287570809895632329, 0.3962735484563137400, 10.00000000000000000 ) ) ;
#42170 = ORIENTED_EDGE ( 'NONE', *, *, #10948, .T. ) ;
#42171 = DIRECTION ( 'NONE',  ( 0.000000000000000000, -2.969158215481698263E-48, 1.000000000000000000 ) ) ;
#42172 = ORIENTED_EDGE ( 'NONE', *, *, #28728, .T. ) ;
#42173 = EDGE_CURVE ( 'NONE', #39178, #9900, #34563, .T. ) ;
#42174 = CYLINDRICAL_SURFACE ( 'NONE', #4547, 1.750000000000015543 ) ;
#42175 = VERTEX_POINT ( 'NONE', #50664 ) ;
#42176 = CARTESIAN_POINT ( 'NONE',  ( -0.3370904143228943828, -0.2449105217885308716, 10.00000000000000000 ) ) ;
#42177 = DIRECTION ( 'NONE',  ( 0.000000000000000000, 0.000000000000000000, 1.000000000000000000 ) ) ;
#42178 = CARTESIAN_POINT ( 'NONE',  ( 111.5540265531850679, 0.000000000000000000, 39.06828755692798438 ) ) ;
#42179 = LINE ( 'NONE', #7047, #8121 ) ;
#42180 = VECTOR ( 'NONE', #29925, 1000.000000000000000 ) ;
#42181 = CARTESIAN_POINT ( 'NONE',  ( 210.0000000000000568, 0.000000000000000000, 162.5682875569279702 ) ) ;
#42182 = VERTEX_POINT ( 'NONE', #50145 ) ;
#42183 = DIRECTION ( 'NONE',  ( -0.000000000000000000, -1.000000000000000000, -0.000000000000000000 ) ) ;
#42184 = DIRECTION ( 'NONE',  ( 0.000000000000000000, 1.000000000000000000, 3.186989995019654210E-49 ) ) ;
#42185 = CARTESIAN_POINT ( 'NONE',  ( 85.00000000000184741, 17.00000000000000000, 65.00000000000000000 ) ) ;
#42186 = CARTESIAN_POINT ( 'NONE',  ( 48.33712804702525290, 13.03701565032775456, -9.367992836599951190 ) ) ;
#42188 = B_SPLINE_CURVE_WITH_KNOTS ( 'NONE', 3,
 ( #39164, #50643, #23230, #158 ),
 .UNSPECIFIED., .F., .F.,
 ( 4, 4 ),
 ( 0.001152428489661398280, 0.001623376834729610679 ),
 .UNSPECIFIED. ) ;
#42187 = CIRCLE ( 'NONE', #9413, 8.000000000000000000 ) ;
#42189 = EDGE_CURVE ( 'NONE', #49578, #10836, #41601, .T. ) ;
#42190 =( BOUNDED_CURVE ( )  B_SPLINE_CURVE ( 3, ( #10464, #6358, #6612, #7127 ),
 .UNSPECIFIED., .F., .F. ) 
 B_SPLINE_CURVE_WITH_KNOTS ( ( 4, 4 ),
 ( 4.712388980384689674, 6.283185307179586232 ),
 .UNSPECIFIED. ) 
 CURVE ( )  GEOMETRIC_REPRESENTATION_ITEM ( )  RATIONAL_B_SPLINE_CURVE ( ( 1.000000000000000000, 0.8047378541243649375, 0.8047378541243649375, 1.000000000000000000 ) ) 
 REPRESENTATION_ITEM ( '' )  );
#42191 = DIRECTION ( 'NONE',  ( 1.000000000000000000, 0.000000000000000000, 0.000000000000000000 ) ) ;
#42192 = EDGE_CURVE ( 'NONE', #34493, #11678, #38190, .T. ) ;
#42193 = CARTESIAN_POINT ( 'NONE',  ( 129.9999999999999432, 17.00000000000000000, -114.9999999999999858 ) ) ;
#42194 = CARTESIAN_POINT ( 'NONE',  ( 130.0000000000002842, 16.00000000000000000, -84.99999999999998579 ) ) ;
#42195 =( BOUNDED_CURVE ( )  B_SPLINE_CURVE ( 3, ( #44891, #18215, #1582, #33893 ),
 .UNSPECIFIED., .F., .F. ) 
 B_SPLINE_CURVE_WITH_KNOTS ( ( 4, 4 ),
 ( 0.000000000000000000, 1.570796326794896558 ),
 .UNSPECIFIED. ) 
 CURVE ( )  GEOMETRIC_REPRESENTATION_ITEM ( )  RATIONAL_B_SPLINE_CURVE ( ( 1.000000000000000000, 0.8047378541243649375, 0.8047378541243649375, 1.000000000000000000 ) ) 
 REPRESENTATION_ITEM ( '' )  );
#42196 = CARTESIAN_POINT ( 'NONE',  ( 115.0540265531850395, 2.143131898507847836E-16, 165.0000000000000000 ) ) ;
#42197 = VERTEX_POINT ( 'NONE', #43511 ) ;
#42198 = EDGE_CURVE ( 'NONE', #33858, #7870, #23775, .T. ) ;
#42199 = CIRCLE ( 'NONE', #12684, 4.000000000000003553 ) ;
#42200 = ADVANCED_FACE ( 'NONE', ( #50413 ), #181, .T. ) ;
#42201 = CARTESIAN_POINT ( 'NONE',  ( -166.6959734468149463, -1.750000000000010214, 40.81828755692798438 ) ) ;
#42202 = AXIS2_PLACEMENT_3D ( 'NONE', #50215, #47144, #12049 ) ;
#42203 = B_SPLINE_CURVE_WITH_KNOTS ( 'NONE', 3,
 ( #41748, #11223, #45575, #26360 ),
 .UNSPECIFIED., .F., .F.,
 ( 4, 4 ),
 ( 0.001937412222931639196, 0.003978261222106112445 ),
 .UNSPECIFIED. ) ;
#42204 = CARTESIAN_POINT ( 'NONE',  ( 193.3040265531851105, 0.000000000000000000, 165.0000000000000000 ) ) ;
#42205 = EDGE_CURVE ( 'NONE', #45889, #20022, #8924, .T. ) ;
#42206 = CARTESIAN_POINT ( 'NONE',  ( 0.8431937073474478073, -1.111389989013496837, 9.955131761384825140 ) ) ;
#42207 = EDGE_CURVE ( 'NONE', #11313, #42347, #18882, .T. ) ;
#42208 =( BOUNDED_CURVE ( )  B_SPLINE_CURVE ( 3, ( #41413, #41666, #44979, #22166 ),
 .UNSPECIFIED., .F., .F. ) 
 B_SPLINE_CURVE_WITH_KNOTS ( ( 4, 4 ),
 ( 1.570796326794896558, 3.141592653589793116 ),
 .UNSPECIFIED. ) 
 CURVE ( )  GEOMETRIC_REPRESENTATION_ITEM ( )  RATIONAL_B_SPLINE_CURVE ( ( 1.000000000000000000, 0.8047378541243649375, 0.8047378541243649375, 1.000000000000000000 ) ) 
 REPRESENTATION_ITEM ( '' )  );
#42209 = VERTEX_POINT ( 'NONE', #8383 ) ;
#42210 = VERTEX_POINT ( 'NONE', #46566 ) ;
#42211 = DIRECTION ( 'NONE',  ( -1.000000000000000000, -0.000000000000000000, -0.000000000000000000 ) ) ;
#42212 = EDGE_CURVE ( 'NONE', #5114, #2259, #7617, .T. ) ;
#42213 = DIRECTION ( 'NONE',  ( -1.000000000000000000, 0.000000000000000000, 0.000000000000000000 ) ) ;
#42214 = EDGE_CURVE ( 'NONE', #17359, #32354, #43811, .T. ) ;
#42215 = VERTEX_POINT ( 'NONE', #39439 ) ;
#42216 = ORIENTED_EDGE ( 'NONE', *, *, #13339, .T. ) ;
#42217 = CARTESIAN_POINT ( 'NONE',  ( -194.9999999999999432, 173.0000000000000000, 112.0000000000000000 ) ) ;
#42218 = CARTESIAN_POINT ( 'NONE',  ( 0.4277546898748997295, 1.184419892831248378, 9.974012008644017158 ) ) ;
#42219 = DIRECTION ( 'NONE',  ( -0.000000000000000000, -0.000000000000000000, 1.000000000000000000 ) ) ;
#42220 = AXIS2_PLACEMENT_3D ( 'NONE', #3298, #236, #18944 ) ;
#42221 = VECTOR ( 'NONE', #17690, 1000.000000000000000 ) ;
#42222 = ORIENTED_EDGE ( 'NONE', *, *, #23634, .F. ) ;
#42223 = EDGE_LOOP ( 'NONE', ( #8036, #47876, #34805, #48226 ) ) ;
#42224 = VERTEX_POINT ( 'NONE', #43001 ) ;
#42225 = CARTESIAN_POINT ( 'NONE',  ( -168.4459734468149463, 0.000000000000000000, 79.06828755692797017 ) ) ;
#42226 = VECTOR ( 'NONE', #21877, 1000.000000000000000 ) ;
#42227 = LINE ( 'NONE', #15032, #48693 ) ;
#42228 = DIRECTION ( 'NONE',  ( 0.000000000000000000, -1.000000000000000000, 0.000000000000000000 ) ) ;
#42229 = CARTESIAN_POINT ( 'NONE',  ( -47.72109971266203132, -1.750000000000009548, -160.2068387089191219 ) ) ;
#42230 = ORIENTED_EDGE ( 'NONE', *, *, #10486, .F. ) ;
#42231 = CARTESIAN_POINT ( 'NONE',  ( 31.55402655318503236, 0.000000000000000000, 39.06828755692798438 ) ) ;
#42232 = EDGE_CURVE ( 'NONE', #16502, #49251, #7881, .T. ) ;
#42233 = SURFACE_STYLE_FILL_AREA ( #29674 ) ;
#42234 = ORIENTED_EDGE ( 'NONE', *, *, #12642, .T. ) ;
#42235 = ORIENTED_EDGE ( 'NONE', *, *, #28799, .F. ) ;
#42236 = LINE ( 'NONE', #42986, #44241 ) ;
#42237 = CARTESIAN_POINT ( 'NONE',  ( -46.69597344681494633, 1.750000000000010214, -39.18171244307202983 ) ) ;
#42238 = CARTESIAN_POINT ( 'NONE',  ( 71.55402655318505367, -1.025126265847089657, 79.06828755692797017 ) ) ;
#42239 = VERTEX_POINT ( 'NONE', #23524 ) ;
#42240 = ORIENTED_EDGE ( 'NONE', *, *, #10586, .T. ) ;
#42241 = CARTESIAN_POINT ( 'NONE',  ( 75.05402655318509630, 1.025126265847089213, -160.9317124430720014 ) ) ;
#42242 =( NAMED_UNIT ( * ) PLANE_ANGLE_UNIT ( ) SI_UNIT ( $, .RADIAN. ) );
#42243 = CARTESIAN_POINT ( 'NONE',  ( 224.9999999999999716, -175.0000000000000000, 474.9999999999998863 ) ) ;
#42244 = CARTESIAN_POINT ( 'NONE',  ( 34.32915281903212446, -1.750000000000009548, -38.15658617722494483 ) ) ;
#42245 = DIRECTION ( 'NONE',  ( 1.000000000000000000, 0.000000000000000000, 0.000000000000000000 ) ) ;
#42246 = AXIS2_PLACEMENT_3D ( 'NONE', #12942, #12198, #24008 ) ;
#42247 = ORIENTED_EDGE ( 'NONE', *, *, #35896, .F. ) ;
#42248 = PRESENTATION_STYLE_ASSIGNMENT (( #10947 ) ) ;
#42249 = CARTESIAN_POINT ( 'NONE',  ( -85.67084718096784002, 1.750000000000009548, 41.84341382277508359 ) ) ;
#42251 = AXIS2_PLACEMENT_3D ( 'NONE', #48266, #16763, #29068 ) ;
#42250 = FACE_OUTER_BOUND ( 'NONE', #48858, .T. ) ;
#42252 = CARTESIAN_POINT ( 'NONE',  ( 232.4999999999999716, -169.9999999999999716, 62.29650858650038003 ) ) ;
#42253 = B_SPLINE_CURVE_WITH_KNOTS ( 'NONE', 3,
 ( #34386, #18960, #38251, #46396 ),
 .UNSPECIFIED., .F., .F.,
 ( 4, 4 ),
 ( 0.9811748202683390208, 0.9878904167554125593 ),
 .UNSPECIFIED. ) ;
#42254 = DIRECTION ( 'NONE',  ( -1.000000000000000000, 0.000000000000000000, 0.000000000000000000 ) ) ;
#42255 = VECTOR ( 'NONE', #3525, 1000.000000000000000 ) ;
#42256 = FACE_BOUND ( 'NONE', #38334, .T. ) ;
#42257 = EDGE_LOOP ( 'NONE', ( #11069, #16878, #33984, #8792, #31630, #49007 ) ) ;
#42258 = CARTESIAN_POINT ( 'NONE',  ( 0.4166666666666664631, 0.000000000000000000, 10.00000000000000000 ) ) ;
#42259 = CARTESIAN_POINT ( 'NONE',  ( 1.250000000000000222, 0.000000000000000000, 10.00000000000000000 ) ) ;
#42260 = CIRCLE ( 'NONE', #39840, 4.000000000000003553 ) ;
#42261 = CARTESIAN_POINT ( 'NONE',  ( 185.0000000000000284, -174.9999999999999716, -111.0000000000001563 ) ) ;
#42262 = VECTOR ( 'NONE', #15284, 1000.000000000000000 ) ;
#42263 = ORIENTED_EDGE ( 'NONE', *, *, #17143, .T. ) ;
#42264 = FACE_OUTER_BOUND ( 'NONE', #47776, .T. ) ;
#42265 = ADVANCED_FACE ( 'NONE', ( #35594 ), #428, .F. ) ;
#42266 = EDGE_CURVE ( 'NONE', #7200, #357, #16075, .T. ) ;
#42267 = LINE ( 'NONE', #3005, #29494 ) ;
#42268 = ORIENTED_EDGE ( 'NONE', *, *, #31986, .T. ) ;
#42269 = CARTESIAN_POINT ( 'NONE',  ( 168.9999999999999716, 165.0000000000000000, -340.0000000000001705 ) ) ;
#42270 = CARTESIAN_POINT ( 'NONE',  ( 185.0000000000000000, -164.9999999999999432, -344.0000000000001137 ) ) ;
#42271 = CARTESIAN_POINT ( 'NONE',  ( 33.30402655318503946, 0.000000000000000000, 165.0000000000000000 ) ) ;
#42272 = EDGE_CURVE ( 'NONE', #28163, #11666, #3759, .T. ) ;
#42273 = ORIENTED_EDGE ( 'NONE', *, *, #12631, .F. ) ;
#42274 = EDGE_LOOP ( 'NONE', ( #44459, #34112, #10404, #42649, #35437 ) ) ;
#42275 = ORIENTED_EDGE ( 'NONE', *, *, #31574, .F. ) ;
#42276 = ADVANCED_FACE ( 'NONE', ( #11977 ), #31741, .F. ) ;
#42277 = DIRECTION ( 'NONE',  ( -1.000000000000000000, -0.000000000000000000, -0.000000000000000000 ) ) ;
#42278 = EDGE_CURVE ( 'NONE', #41788, #37196, #42260, .T. ) ;
#42279 = AXIS2_PLACEMENT_3D ( 'NONE', #44843, #17422, #45781 ) ;
#42280 = ORIENTED_EDGE ( 'NONE', *, *, #26521, .F. ) ;
#42281 = CARTESIAN_POINT ( 'NONE',  ( -165.0000000000000284, 17.00000000000000000, -114.9999999999999858 ) ) ;
#42282 = DIRECTION ( 'NONE',  ( 0.000000000000000000, 0.000000000000000000, 1.000000000000000000 ) ) ;
#42283 = AXIS2_PLACEMENT_3D ( 'NONE', #853, #28545, #355 ) ;
#42284 = CARTESIAN_POINT ( 'NONE',  ( 113.3040265531850537, -1.749999999999997335, -79.18171244307201562 ) ) ;
#42285 = ADVANCED_FACE ( 'NONE', ( #20674 ), #2375, .T. ) ;
#42286 = CARTESIAN_POINT ( 'NONE',  ( 0.4154044336478738830, -2.070917815000952178, 9.890170120223997330 ) ) ;
#42287 = EDGE_LOOP ( 'NONE', ( #26254, #2779, #1758, #14537 ) ) ;
#42288 = DIRECTION ( 'NONE',  ( 1.000000000000000000, 0.000000000000000000, -0.000000000000000000 ) ) ;
#42289 = CARTESIAN_POINT ( 'NONE',  ( -34.38161489319221431, 14.98878603239709939, -8.600750091277038933 ) ) ;
#42290 = LINE ( 'NONE', #49185, #19326 ) ;
#42291 = AXIS2_PLACEMENT_3D ( 'NONE', #33417, #13642, #41349 ) ;
#42292 = ORIENTED_EDGE ( 'NONE', *, *, #46571, .F. ) ;
#42293 = CARTESIAN_POINT ( 'NONE',  ( 168.9999999999999716, 175.0000000000000284, -342.0000000000001137 ) ) ;
#42294 = CARTESIAN_POINT ( 'NONE',  ( 355.9999999999999432, -183.0000000000000000, 357.9999999999998295 ) ) ;
#42295 = ORIENTED_EDGE ( 'NONE', *, *, #12252, .F. ) ;
#42296 = AXIS2_PLACEMENT_3D ( 'NONE', #24351, #4585, #27176 ) ;
#42297 = ORIENTED_EDGE ( 'NONE', *, *, #29353, .F. ) ;
#42298 = ORIENTED_EDGE ( 'NONE', *, *, #1410, .T. ) ;
#42299 = CARTESIAN_POINT ( 'NONE',  ( 10.69268279052430159, 12.77266927778462779, -2.870787844569587133 ) ) ;
#42300 = CARTESIAN_POINT ( 'NONE',  ( 27.73884755486784570, -25.23502201956245017, 7.697694107796188234 ) ) ;
#42301 = EDGE_LOOP ( 'NONE', ( #2169, #3632, #24226, #23238, #5749 ) ) ;
#42302 = VECTOR ( 'NONE', #34671, 1000.000000000000000 ) ;
#42303 = DIRECTION ( 'NONE',  ( 1.000000000000000000, 0.000000000000000000, 0.000000000000000000 ) ) ;
#42304 = CARTESIAN_POINT ( 'NONE',  ( 111.5540265531850537, 1.025126265847081886, 79.06828755692797017 ) ) ;
#42305 = CARTESIAN_POINT ( 'NONE',  ( 181.0000000000000284, -9.999999999999953815, -115.0000000000001563 ) ) ;
#42306 = CARTESIAN_POINT ( 'NONE',  ( -7.576114424932982594, 33.14742743729794938, 7.906207997025717304 ) ) ;
#42307 = DIRECTION ( 'NONE',  ( 0.000000000000000000, -1.000000000000000000, -0.000000000000000000 ) ) ;
#42308 = PLANE ( 'NONE',  #13417 ) ;
#42309 = CARTESIAN_POINT ( 'NONE',  ( -1.011271242968677875, -0.7347315653656004697, 3.333333333333333481 ) ) ;
#42310 = CARTESIAN_POINT ( 'NONE',  ( 1.011271242968688311, -0.7347315653655855927, -10.00000000000000000 ) ) ;
#42311 = ADVANCED_FACE ( 'NONE', ( #48332 ), #43764, .F. ) ;
#42312 = EDGE_LOOP ( 'NONE', ( #23059, #24442, #37021, #10614, #50017 ) ) ;
#42313 = DIRECTION ( 'NONE',  ( 0.000000000000000000, 0.000000000000000000, 1.000000000000000000 ) ) ;
#42314 = CARTESIAN_POINT ( 'NONE',  ( -7.721099712662037540, -1.750000000000023315, -38.15658617722493062 ) ) ;
#42316 = AXIS2_PLACEMENT_3D ( 'NONE', #45735, #40676, #13955 ) ;
#42315 = CARTESIAN_POINT ( 'NONE',  ( 339.9999999999998863, -182.9999999999999716, 355.9999999999997726 ) ) ;
#42317 = CARTESIAN_POINT ( 'NONE',  ( 14.49999999999999822, -46.01315789473684248, -5.916985404131813731 ) ) ;
#42318 = EDGE_LOOP ( 'NONE', ( #22605, #23669, #28557, #1391 ) ) ;
#42319 = FACE_OUTER_BOUND ( 'NONE', #43912, .T. ) ;
#42320 = CARTESIAN_POINT ( 'NONE',  ( 135.0000000000015632, 17.00000000000000000, 35.00000000000000000 ) ) ;
#42321 = DIRECTION ( 'NONE',  ( 1.132880637372608740E-16, 4.718402560806925739E-50, 1.000000000000000000 ) ) ;
#42322 = CARTESIAN_POINT ( 'NONE',  ( -7.576114424932982594, 33.14742743729794938, 7.906207997025717304 ) ) ;
#42323 = CARTESIAN_POINT ( 'NONE',  ( -0.3910393408547386818, -3.877122853643371947, 9.741991644047244492 ) ) ;
#42324 = ORIENTED_EDGE ( 'NONE', *, *, #40442, .F. ) ;
#42325 = SURFACE_STYLE_USAGE ( .BOTH. , #23074 ) ;
#42326 = ORIENTED_EDGE ( 'NONE', *, *, #12660, .T. ) ;
#42327 = CARTESIAN_POINT ( 'NONE',  ( 358.0000000000000568, 175.0000000000000284, -94.00000000000019895 ) ) ;
#42328 = ORIENTED_EDGE ( 'NONE', *, *, #9041, .T. ) ;
#42329 = DIRECTION ( 'NONE',  ( 0.000000000000000000, 0.000000000000000000, 1.000000000000000000 ) ) ;
#42330 = DIRECTION ( 'NONE',  ( 1.000000000000000000, 0.000000000000000000, 0.000000000000000000 ) ) ;
#42331 = ORIENTED_EDGE ( 'NONE', *, *, #47261, .T. ) ;
#42332 = CARTESIAN_POINT ( 'NONE',  ( 164.9999999999999716, 6.000000000000060396, -350.0000000000001705 ) ) ;
#42333 = ORIENTED_EDGE ( 'NONE', *, *, #30777, .F. ) ;
#42334 = VECTOR ( 'NONE', #38702, 1000.000000000000000 ) ;
#42335 = EDGE_LOOP ( 'NONE', ( #18206, #48792, #12397, #49152 ) ) ;
#42336 = FACE_OUTER_BOUND ( 'NONE', #49877, .T. ) ;
#42337 = DIRECTION ( 'NONE',  ( -0.000000000000000000, -1.000000000000000000, -0.000000000000000000 ) ) ;
#42338 = VERTEX_POINT ( 'NONE', #20166 ) ;
#42339 = CARTESIAN_POINT ( 'NONE',  ( 236.0000000000000000, -169.9999999999999716, 4.999999999999616307 ) ) ;
#42340 = FACE_BOUND ( 'NONE', #37993, .T. ) ;
#42341 = EDGE_CURVE ( 'NONE', #30921, #12217, #24790, .T. ) ;
#42342 = FACE_OUTER_BOUND ( 'NONE', #32531, .T. ) ;
#42343 = ORIENTED_EDGE ( 'NONE', *, *, #48382, .F. ) ;
#42344 = ORIENTED_EDGE ( 'NONE', *, *, #33212, .F. ) ;
#42345 = CARTESIAN_POINT ( 'NONE',  ( 164.9999999999999716, 16.00000000000000000, 115.0000000000000142 ) ) ;
#42346 = DIRECTION ( 'NONE',  ( 0.000000000000000000, 6.123233995736766036E-17, -1.000000000000000000 ) ) ;
#42347 = VERTEX_POINT ( 'NONE', #13221 ) ;
#42348 = CARTESIAN_POINT ( 'NONE',  ( -164.9459734468149463, 1.025126265847089657, -37.43171244307202272 ) ) ;
#42349 = CARTESIAN_POINT ( 'NONE',  ( 185.0000000000000568, 175.0000000000000284, 355.9999999999998863 ) ) ;
#42350 = VERTEX_POINT ( 'NONE', #1441 ) ;
#42351 = CARTESIAN_POINT ( 'NONE',  ( -45.67084718096785423, -1.750000000000009326, -158.1565861772249377 ) ) ;
#42352 = B_SPLINE_CURVE_WITH_KNOTS ( 'NONE', 3,
 ( #35614, #1462, #39455, #43528 ),
 .UNSPECIFIED., .F., .F.,
 ( 4, 4 ),
 ( 3.806817868859629271E-16, 0.009762429722931321996 ),
 .UNSPECIFIED. ) ;
#42353 =( BOUNDED_CURVE ( )  B_SPLINE_CURVE ( 3, ( #35064, #50633, #15534, #31197 ),
 .UNSPECIFIED., .F., .F. ) 
 B_SPLINE_CURVE_WITH_KNOTS ( ( 4, 4 ),
 ( 0.000000000000000000, 1.570796326794896558 ),
 .UNSPECIFIED. ) 
 CURVE ( )  GEOMETRIC_REPRESENTATION_ITEM ( )  RATIONAL_B_SPLINE_CURVE ( ( 1.000000000000000000, 0.8047378541243649375, 0.8047378541243649375, 1.000000000000000000 ) ) 
 REPRESENTATION_ITEM ( '' )  );
#42354 = CARTESIAN_POINT ( 'NONE',  ( 135.0000000000009663, 16.00000000000000000, -24.99999999999999289 ) ) ;
#42355 = ORIENTED_EDGE ( 'NONE', *, *, #8382, .T. ) ;
#42356 = ADVANCED_BREP_SHAPE_REPRESENTATION ( '', ( #5698, #45486 ), #46291 ) ;
#42357 = FACE_BOUND ( 'NONE', #27922, .T. ) ;
#42358 = CARTESIAN_POINT ( 'NONE',  ( 31.55402655318503236, 1.025126265847089435, -117.4317124430720156 ) ) ;
#42359 = CARTESIAN_POINT ( 'NONE',  ( 339.9999999999999432, 167.0000000000000000, -356.0000000000002274 ) ) ;
#42360 = ORIENTED_EDGE ( 'NONE', *, *, #314, .F. ) ;
#42361 = CARTESIAN_POINT ( 'NONE',  ( 50.11058929355270664, -7.578863168071591438, 7.455576670931136185 ) ) ;
#42362 = CARTESIAN_POINT ( 'NONE',  ( -19.99999999999878142, 17.00000000000000000, 30.00000000000000000 ) ) ;
#42363 = EDGE_LOOP ( 'NONE', ( #262, #30004, #38520, #10536 ) ) ;
#42364 = EDGE_CURVE ( 'NONE', #49806, #22181, #5017, .T. ) ;
#42365 = ORIENTED_EDGE ( 'NONE', *, *, #22080, .T. ) ;
#42366 = DIRECTION ( 'NONE',  ( -1.744890010039029680E-14, 3.027509557426970260E-18, -1.000000000000000000 ) ) ;
#42367 = CARTESIAN_POINT ( 'NONE',  ( 164.9999999999999716, -164.9999999999999432, 355.9999999999998863 ) ) ;
#42368 = DIRECTION ( 'NONE',  ( 0.000000000000000000, 1.000000000000000000, -2.537652627714643577E-15 ) ) ;
#42369 = CARTESIAN_POINT ( 'NONE',  ( 169.0000000000000000, -174.9999999999999716, -111.0000000000001563 ) ) ;
#42370 = SURFACE_STYLE_FILL_AREA ( #30586 ) ;
#42371 = CARTESIAN_POINT ( 'NONE',  ( 30.00000000000153833, 17.00000000000000000, 60.00000000000000000 ) ) ;
#42372 = APPLICATION_CONTEXT ( 'automotive_design' ) ;
#42373 = DIRECTION ( 'NONE',  ( -0.000000000000000000, -1.000000000000000000, -0.000000000000000000 ) ) ;
#42374 = ORIENTED_EDGE ( 'NONE', *, *, #48789, .F. ) ;
#42375 = CARTESIAN_POINT ( 'NONE',  ( -14.99999999999937472, 16.00000000000000000, -54.99999999999999289 ) ) ;
#42376 = DIRECTION ( 'NONE',  ( 0.000000000000000000, 0.000000000000000000, -1.000000000000000000 ) ) ;
#42377 = SURFACE_SIDE_STYLE ('',( #45697 ) ) ;
#42379 = EDGE_LOOP ( 'NONE', ( #42298, #12360 ) ) ;
#42378 = VECTOR ( 'NONE', #16160, 1000.000000000000000 ) ;
#42380 = DIRECTION ( 'NONE',  ( 0.000000000000000000, 1.000000000000000000, 0.000000000000000000 ) ) ;
#42381 = CARTESIAN_POINT ( 'NONE',  ( 24.39427009665985224, 44.07992421011656603, 8.807470649214879543 ) ) ;
#42382 = ORIENTED_EDGE ( 'NONE', *, *, #24326, .F. ) ;
#42383 = CARTESIAN_POINT ( 'NONE',  ( 113.3040265531850537, 0.000000000000000000, 165.0000000000000000 ) ) ;
#42384 = LINE ( 'NONE', #46457, #33957 ) ;
#42385 = CARTESIAN_POINT ( 'NONE',  ( -14.99999999999812594, 16.00000000000000000, 90.00000000000000000 ) ) ;
#42386 = ORIENTED_EDGE ( 'NONE', *, *, #2878, .F. ) ;
#42387 = LINE ( 'NONE', #74, #32701 ) ;
#42388 = CARTESIAN_POINT ( 'NONE',  ( 181.0000000000000000, -93.49999999999998579, -340.0000000000001137 ) ) ;
#42389 = VERTEX_POINT ( 'NONE', #32733 ) ;
#42390 = DIRECTION ( 'NONE',  ( 1.000000000000000000, 0.000000000000000000, 0.000000000000000000 ) ) ;
#42391 = LINE ( 'NONE', #18787, #15223 ) ;
#42392 = ADVANCED_FACE ( 'NONE', ( #9379 ), #32498, .F. ) ;
#42393 = VERTEX_POINT ( 'NONE', #24531 ) ;
#42394 = ORIENTED_EDGE ( 'NONE', *, *, #38681, .T. ) ;
#42395 = DIRECTION ( 'NONE',  ( -1.586032892321652236E-16, -1.000000000000000000, -2.288264760618012091E-48 ) ) ;
#42396 = DIRECTION ( 'NONE',  ( 0.000000000000000000, 0.000000000000000000, -1.000000000000000000 ) ) ;
#42397 = ORIENTED_EDGE ( 'NONE', *, *, #6251, .F. ) ;
#42398 = ORIENTED_EDGE ( 'NONE', *, *, #11534, .F. ) ;
#42399 = CARTESIAN_POINT ( 'NONE',  ( 74.32915281903215998, 1.750000000000009548, -0.2068387089191121020 ) ) ;
#42400 = CARTESIAN_POINT ( 'NONE',  ( -64.99999999999783995, 17.00000000000000000, 95.00000000000000000 ) ) ;
#42401 = DIRECTION ( 'NONE',  ( -1.000000000000000000, 0.000000000000000000, 0.000000000000000000 ) ) ;
#42402 = ORIENTED_EDGE ( 'NONE', *, *, #37480, .F. ) ;
#42403 = DIRECTION ( 'NONE',  ( 0.000000000000000000, 0.000000000000000000, -1.000000000000000000 ) ) ;
#42404 = ORIENTED_EDGE ( 'NONE', *, *, #8393, .T. ) ;
#42405 = EDGE_CURVE ( 'NONE', #43021, #16274, #937, .T. ) ;
#42406 = EDGE_CURVE ( 'NONE', #38030, #19831, #25042, .T. ) ;
#42407 = CARTESIAN_POINT ( 'NONE',  ( -64.99999999999877787, 17.00000000000000000, 30.00000000000000000 ) ) ;
#42408 = CARTESIAN_POINT ( 'NONE',  ( 195.0540265531851105, -1.025126265847089435, 82.56828755692798438 ) ) ;
#42409 = EDGE_CURVE ( 'NONE', #4194, #35096, #20954, .T. ) ;
#42410 = CARTESIAN_POINT ( 'NONE',  ( 4.763548243873389154, -16.57409059453848599, 8.727788335465566760 ) ) ;
#42411 = VERTEX_POINT ( 'NONE', #17327 ) ;
#42412 = VECTOR ( 'NONE', #24219, 1000.000000000000114 ) ;
#42413 = VERTEX_POINT ( 'NONE', #35850 ) ;
#42414 = EDGE_LOOP ( 'NONE', ( #36118, #45489, #39403, #39861, #46226, #32488 ) ) ;
#42415 = CARTESIAN_POINT ( 'NONE',  ( -8.445973446814962315, 1.025126265847096985, 162.5682875569279986 ) ) ;
#42416 = CARTESIAN_POINT ( 'NONE',  ( -64.99999999999783995, 16.00000000000000000, 95.00000000000000000 ) ) ;
#42417 = VERTEX_POINT ( 'NONE', #16578 ) ;
#42418 = CARTESIAN_POINT ( 'NONE',  ( -1.419290803332700523, -0.2086015876293249582, 9.950105812514305370 ) ) ;
#42419 = ADVANCED_FACE ( 'NONE', ( #28127 ), #24290, .F. ) ;
#42420 = ADVANCED_FACE ( 'NONE', ( #8633 ), #12719, .T. ) ;
#42421 = VERTEX_POINT ( 'NONE', #21677 ) ;
#42422 = DIRECTION ( 'NONE',  ( -1.000000000000000000, -0.000000000000000000, -0.000000000000000000 ) ) ;
#42423 = ORIENTED_EDGE ( 'NONE', *, *, #26469, .T. ) ;
#42424 = DIRECTION ( 'NONE',  ( 1.000000000000000000, -4.758098676964957447E-16, 1.642146637880645005E-47 ) ) ;
#42425 = ADVANCED_FACE ( 'NONE', ( #49586 ), #5779, .T. ) ;
#42426 = DIRECTION ( 'NONE',  ( -0.000000000000000000, -0.000000000000000000, -1.000000000000000000 ) ) ;
#42427 = CARTESIAN_POINT ( 'NONE',  ( -17.23491422248386584, 0.5912720620001978844, 8.727788335465566760 ) ) ;
#42428 = DIRECTION ( 'NONE',  ( 1.000000000000000000, 0.000000000000000000, -0.000000000000000000 ) ) ;
#42429 = EDGE_CURVE ( 'NONE', #15426, #28175, #3734, .T. ) ;
#42430 =( BOUNDED_CURVE ( )  B_SPLINE_CURVE ( 3, ( #12066, #31321, #16408, #7969 ),
 .UNSPECIFIED., .F., .F. ) 
 B_SPLINE_CURVE_WITH_KNOTS ( ( 4, 4 ),
 ( 0.000000000000000000, 1.570796326794896558 ),
 .UNSPECIFIED. ) 
 CURVE ( )  GEOMETRIC_REPRESENTATION_ITEM ( )  RATIONAL_B_SPLINE_CURVE ( ( 1.000000000000000000, 0.8047378541243649375, 0.8047378541243649375, 1.000000000000000000 ) ) 
 REPRESENTATION_ITEM ( '' )  );
#42431 = CARTESIAN_POINT ( 'NONE',  ( 0.7849184246612691540, -1.242376769536456704, 9.958264684458541183 ) ) ;
#42432 = VERTEX_POINT ( 'NONE', #6534 ) ;
#42433 = CARTESIAN_POINT ( 'NONE',  ( -30.67467450244469873, 28.55398182363574122, 7.544061037322996377 ) ) ;
#42434 = EDGE_CURVE ( 'NONE', #49222, #29784, #16859, .T. ) ;
#42435 = FACE_OUTER_BOUND ( 'NONE', #26062, .T. ) ;
#42436 = B_SPLINE_SURFACE_WITH_KNOTS ( 'NONE', 3, 3, ( 
 ( #18508, #46436, #49515, #34187 ),
 ( #23120, #49763, #30322, #42610 ),
 ( #10814, #26465, #42102, #6968 ),
 ( #22617, #18752, #34436, #46175 ) ),
 .UNSPECIFIED., .F., .F., .F.,
 ( 4, 4 ),
 ( 4, 4 ),
 ( 0.000000000000000000, 1.000000000000000000 ),
 ( 0.000000000000000000, 1.000000000000000000 ),
 .UNSPECIFIED. ) ;
#42437 = DIRECTION ( 'NONE',  ( 0.000000000000000000, 1.000000000000000000, 0.000000000000000000 ) ) ;
#42438 = CARTESIAN_POINT ( 'NONE',  ( -210.0000000000000568, 0.000000000000000000, -119.1817124430720440 ) ) ;
#42439 = PLANE ( 'NONE',  #40452 ) ;
#42440 = CARTESIAN_POINT ( 'NONE',  ( -114.9999999999981526, 16.00000000000000000, 65.00000000000000000 ) ) ;
#42441 = ORIENTED_EDGE ( 'NONE', *, *, #13978, .T. ) ;
#42442 = DIRECTION ( 'NONE',  ( 4.755310728521421461E-16, 0.000000000000000000, 1.000000000000000000 ) ) ;
#42443 = EDGE_CURVE ( 'NONE', #40582, #17018, #27223, .T. ) ;
#42444 = CYLINDRICAL_SURFACE ( 'NONE', #30419, 1.750000000000001554 ) ;
#42445 = VERTEX_POINT ( 'NONE', #48836 ) ;
#42446 = EDGE_CURVE ( 'NONE', #47543, #48228, #49829, .T. ) ;
#42447 = VECTOR ( 'NONE', #10196, 1000.000000000000000 ) ;
#42448 = EDGE_CURVE ( 'NONE', #40485, #30782, #18656, .T. ) ;
#42449 = DIRECTION ( 'NONE',  ( -1.000000000000000000, 0.000000000000000000, -0.000000000000000000 ) ) ;
#42450 = CARTESIAN_POINT ( 'NONE',  ( 0.000000000000000000, -184.7999999999999545, 359.7999999999997840 ) ) ;
#42451 = CARTESIAN_POINT ( 'NONE',  ( 181.0000000000000284, -174.9999999999999716, -115.0000000000001563 ) ) ;
#42452 = ADVANCED_FACE ( 'NONE', ( #13726 ), #45251, .T. ) ;
#42453 = VERTEX_POINT ( 'NONE', #17581 ) ;
#42454 = VERTEX_POINT ( 'NONE', #21419 ) ;
#42455 = LINE ( 'NONE', #2456, #20995 ) ;
#42456 = EDGE_CURVE ( 'NONE', #16943, #19122, #36553, .T. ) ;
#42457 = DIRECTION ( 'NONE',  ( -0.000000000000000000, -0.000000000000000000, -1.000000000000000000 ) ) ;
#42458 = ORIENTED_EDGE ( 'NONE', *, *, #16397, .T. ) ;
#42459 = VERTEX_POINT ( 'NONE', #14223 ) ;
#42460 = CARTESIAN_POINT ( 'NONE',  ( 0.3862712429686894766, -1.188820645368940276, 10.00000000000000000 ) ) ;
#42461 = CARTESIAN_POINT ( 'NONE',  ( -4.763548243873389154, 16.57409059453848599, 8.727788335465566760 ) ) ;
#42462 = CYLINDRICAL_SURFACE ( 'NONE', #29981, 1.750000000000015543 ) ;
#42463 = EDGE_LOOP ( 'NONE', ( #45698, #17920, #19497, #46452 ) ) ;
#42464 = VERTEX_POINT ( 'NONE', #29886 ) ;
#42465 = ORIENTED_EDGE ( 'NONE', *, *, #7218, .T. ) ;
#42466 = DIRECTION ( 'NONE',  ( -3.172065784643302499E-16, -1.000000000000000000, 2.537652627714642000E-15 ) ) ;
#42467 = DIRECTION ( 'NONE',  ( 0.000000000000000000, -0.000000000000000000, -1.000000000000000000 ) ) ;
#42468 = ORIENTED_EDGE ( 'NONE', *, *, #7538, .F. ) ;
#42469 = DIRECTION ( 'NONE',  ( 0.000000000000000000, 0.000000000000000000, -1.000000000000000000 ) ) ;
#42470 = LINE ( 'NONE', #7091, #20038 ) ;
#42471 = DIRECTION ( 'NONE',  ( -1.156482317317870492E-16, 1.000000000000000000, 0.000000000000000000 ) ) ;
#42472 = ORIENTED_EDGE ( 'NONE', *, *, #25370, .F. ) ;
#42473 = ADVANCED_FACE ( 'NONE', ( #37109 ), #34001, .F. ) ;
#42474 = VERTEX_POINT ( 'NONE', #30142 ) ;
#42475 = CARTESIAN_POINT ( 'NONE',  ( 33.30402655318503946, 1.750000000000010214, -39.18171244307202983 ) ) ;
#42476 = CARTESIAN_POINT ( 'NONE',  ( 175.0000000000000000, 15.00000000000000000, -122.5000000000000000 ) ) ;
#42477 = CARTESIAN_POINT ( 'NONE',  ( -5.000000000000000000, -165.1999999999999602, -359.8000000000002387 ) ) ;
#42478 = ORIENTED_EDGE ( 'NONE', *, *, #34394, .T. ) ;
#42479 = ADVANCED_FACE ( 'NONE', ( #33255 ), #30398, .F. ) ;
#42480 = VERTEX_POINT ( 'NONE', #29382 ) ;
#42481 = CARTESIAN_POINT ( 'NONE',  ( 111.5540265531850679, 0.000000000000000000, 42.56828755692795596 ) ) ;
#42482 = CARTESIAN_POINT ( 'NONE',  ( 155.0540265531850537, 2.143131898507880377E-16, 2.568287556927978166 ) ) ;
#42483 =( BOUNDED_CURVE ( )  B_SPLINE_CURVE ( 3, ( #10967, #8145, #24052, #23265 ),
 .UNSPECIFIED., .F., .F. ) 
 B_SPLINE_CURVE_WITH_KNOTS ( ( 4, 4 ),
 ( 3.141592653589793116, 4.712388980384689674 ),
 .UNSPECIFIED. ) 
 CURVE ( )  GEOMETRIC_REPRESENTATION_ITEM ( )  RATIONAL_B_SPLINE_CURVE ( ( 1.000000000000000000, 0.8047378541243649375, 0.8047378541243649375, 1.000000000000000000 ) ) 
 REPRESENTATION_ITEM ( '' )  );
#42484 = EDGE_CURVE ( 'NONE', #49918, #23986, #32480, .T. ) ;
#42485 = LINE ( 'NONE', #18628, #35059 ) ;
#42486 = CARTESIAN_POINT ( 'NONE',  ( -69.99999999999972999, 16.00000000000000000, -60.00000000000000000 ) ) ;
#42487 = EDGE_CURVE ( 'NONE', #17310, #8816, #37368, .T. ) ;
#42488 = AXIS2_PLACEMENT_3D ( 'NONE', #22943, #14744, #4218 ) ;
#42489 = CARTESIAN_POINT ( 'NONE',  ( 341.9999999999999432, -165.0000000000001137, -94.00000000000019895 ) ) ;
#42490 = VERTEX_POINT ( 'NONE', #10394 ) ;
#42491 = CARTESIAN_POINT ( 'NONE',  ( 349.9999999999999432, -168.9999999999999432, 339.9999999999997726 ) ) ;
#42492 = EDGE_CURVE ( 'NONE', #48360, #15177, #43715, .T. ) ;
#42493 = CARTESIAN_POINT ( 'NONE',  ( 14.48769039275578407, 30.44468701195595983, 8.807470649214879543 ) ) ;
#42494 =( BOUNDED_CURVE ( )  B_SPLINE_CURVE ( 3, ( #20320, #7517, #23152, #23918 ),
 .UNSPECIFIED., .F., .F. ) 
 B_SPLINE_CURVE_WITH_KNOTS ( ( 4, 4 ),
 ( 4.712388980384689674, 6.283185307179586232 ),
 .UNSPECIFIED. ) 
 CURVE ( )  GEOMETRIC_REPRESENTATION_ITEM ( )  RATIONAL_B_SPLINE_CURVE ( ( 1.000000000000000000, 0.8047378541243649375, 0.8047378541243649375, 1.000000000000000000 ) ) 
 REPRESENTATION_ITEM ( '' )  );
#42495 = ADVANCED_FACE ( 'NONE', ( #41684 ), #46504, .F. ) ;
#42496 = CARTESIAN_POINT ( 'NONE',  ( 183.0000000000000284, -9.999999999999953815, -111.0000000000001563 ) ) ;
#42497 = CARTESIAN_POINT ( 'NONE',  ( 113.3040265531850537, 1.749999999999997113, 40.81828755692798438 ) ) ;
#42498 = CARTESIAN_POINT ( 'NONE',  ( 31.94178169330218964, -9.256608784833820991, -3.760136334089591248 ) ) ;
#42499 = CYLINDRICAL_SURFACE ( 'NONE', #27364, 4.000000000000003553 ) ;
#42500 = VERTEX_POINT ( 'NONE', #42941 ) ;
#42501 = CARTESIAN_POINT ( 'NONE',  ( 13.59579750444771307, -10.60877755095900632, 8.727788335465566760 ) ) ;
#42502 = FACE_OUTER_BOUND ( 'NONE', #10995, .T. ) ;
#42503 = CARTESIAN_POINT ( 'NONE',  ( 1.531049279420177101, 0.4659387722960993683, 9.919954280166514593 ) ) ;
#42504 = VERTEX_POINT ( 'NONE', #7820 ) ;
#42505 =( NAMED_UNIT ( * ) PLANE_ANGLE_UNIT ( ) SI_UNIT ( $, .RADIAN. ) );
#42506 = EDGE_CURVE ( 'NONE', #29795, #31313, #5189, .T. ) ;
#42507 = PLANE ( 'NONE',  #37675 ) ;
#42508 = ORIENTED_EDGE ( 'NONE', *, *, #9028, .F. ) ;
#42509 = CARTESIAN_POINT ( 'NONE',  ( 185.0000000000000000, -5.999999999999950262, -350.0000000000001705 ) ) ;
#42510 = CARTESIAN_POINT ( 'NONE',  ( 74.32915281903215998, -1.750000000000010436, -80.20683870891910772 ) ) ;
#42511 = CARTESIAN_POINT ( 'NONE',  ( -0.3443084382165982893, -1.609917862996312676, 9.927568724237803011 ) ) ;
#42512 = ORIENTED_EDGE ( 'NONE', *, *, #23533, .T. ) ;
#42513 = CARTESIAN_POINT ( 'NONE',  ( -1.011271242968688533, 0.7347315653655859258, -3.333333333333333481 ) ) ;
#42514 = ORIENTED_EDGE ( 'NONE', *, *, #32223, .F. ) ;
#42515 = ORIENTED_EDGE ( 'NONE', *, *, #6658, .T. ) ;
#42516 = CYLINDRICAL_SURFACE ( 'NONE', #41033, 4.000000000000003553 ) ;
#42517 = AXIS2_PLACEMENT_3D ( 'NONE', #9373, #12955, #33252 ) ;
#42518 = AXIS2_PLACEMENT_3D ( 'NONE', #12852, #8011, #36479 ) ;
#42519 = EDGE_LOOP ( 'NONE', ( #44481, #36557, #15532, #23746, #47966, #46756 ) ) ;
#42520 = DIRECTION ( 'NONE',  ( -1.612977847700450206E-50, 0.000000000000000000, -1.000000000000000000 ) ) ;
#42521 = CARTESIAN_POINT ( 'NONE',  ( 340.0000000000000568, 181.0000000000000284, 357.9999999999997726 ) ) ;
#42522 = DIRECTION ( 'NONE',  ( -0.000000000000000000, -0.000000000000000000, -1.000000000000000000 ) ) ;
#42523 = AXIS2_PLACEMENT_3D ( 'NONE', #16451, #32358, #32873 ) ;
#42524 = VECTOR ( 'NONE', #35386, 1000.000000000000000 ) ;
#42525 = EDGE_CURVE ( 'NONE', #36023, #30497, #30922, .T. ) ;
#42526 = AXIS2_PLACEMENT_3D ( 'NONE', #3566, #27187, #7688 ) ;
#42527 = CARTESIAN_POINT ( 'NONE',  ( 30.00000000000187228, 17.00000000000000000, 65.00000000000000000 ) ) ;
#42528 = ORIENTED_EDGE ( 'NONE', *, *, #48200, .T. ) ;
#42529 = CARTESIAN_POINT ( 'NONE',  ( 356.0000000000000000, -165.0000000000001137, -340.0000000000002842 ) ) ;
#42530 = LINE ( 'NONE', #23034, #5370 ) ;
#42531 = VECTOR ( 'NONE', #49923, 999.9999999999998863 ) ;
#42532 = ORIENTED_EDGE ( 'NONE', *, *, #2988, .F. ) ;
#42533 = DIRECTION ( 'NONE',  ( 0.000000000000000000, -1.000000000000000000, 1.822804496942679766E-16 ) ) ;
#42534 = CARTESIAN_POINT ( 'NONE',  ( 7.500000000000000000, 224.9999999999999716, -240.0000000000000000 ) ) ;
#42535 = ORIENTED_EDGE ( 'NONE', *, *, #21222, .F. ) ;
#42536 = EDGE_CURVE ( 'NONE', #38752, #46997, #11286, .T. ) ;
#42537 = EDGE_LOOP ( 'NONE', ( #26259, #38650, #5677, #38272 ) ) ;
#42538 = ORIENTED_EDGE ( 'NONE', *, *, #26445, .F. ) ;
#42539 = FACE_OUTER_BOUND ( 'NONE', #12946, .T. ) ;
#42540 = LINE ( 'NONE', #12265, #45488 ) ;
#42541 = VERTEX_POINT ( 'NONE', #39381 ) ;
#42542 = PLANE ( 'NONE',  #45868 ) ;
#42543 = CARTESIAN_POINT ( 'NONE',  ( 1.782521105131670724, -0.3635605703593869920, 9.903764339332079558 ) ) ;
#42544 = ADVANCED_FACE ( 'NONE', ( #3433 ), #19598, .F. ) ;
#42545 = CARTESIAN_POINT ( 'NONE',  ( 71.55402655318505367, 0.000000000000000000, -165.0000000000000000 ) ) ;
#42546 = EDGE_CURVE ( 'NONE', #50239, #8111, #50085, .T. ) ;
#42547 = CYLINDRICAL_SURFACE ( 'NONE', #42220, 4.000000000000003553 ) ;
#42548 = CARTESIAN_POINT ( 'NONE',  ( 31.55402655318503236, -1.025126265847089657, 119.0682875569279560 ) ) ;
#42549 = FILL_AREA_STYLE ('',( #11271 ) ) ;
#42550 = EDGE_CURVE ( 'NONE', #30097, #27796, #34774, .T. ) ;
#42551 = DIRECTION ( 'NONE',  ( 1.000000000000000000, 0.000000000000000000, 0.000000000000000000 ) ) ;
#42552 = AXIS2_PLACEMENT_3D ( 'NONE', #12921, #1400, #9091 ) ;
#42553 = VERTEX_POINT ( 'NONE', #3697 ) ;
#42554 = EDGE_CURVE ( 'NONE', #21151, #17197, #29174, .T. ) ;
#42555 = VECTOR ( 'NONE', #37006, 1000.000000000000000 ) ;
#42556 = EDGE_CURVE ( 'NONE', #48152, #45274, #34425, .T. ) ;
#42557 = CARTESIAN_POINT ( 'NONE',  ( 194.9999999999999432, -173.0000000000000000, 112.0000000000000284 ) ) ;
#42558 = DIRECTION ( 'NONE',  ( -1.000000000000000000, -0.000000000000000000, -0.000000000000000000 ) ) ;
#42559 = CARTESIAN_POINT ( 'NONE',  ( 1.055760676366898521, 37.52140099356444836, -2.490396854064190535 ) ) ;
#42560 = CARTESIAN_POINT ( 'NONE',  ( -167.4999999999999432, -112.5000000000000000, -18.87174264961130632 ) ) ;
#42561 = EDGE_LOOP ( 'NONE', ( #48453, #34506, #29929, #43918, #33036, #20706 ) ) ;
#42562 = CARTESIAN_POINT ( 'NONE',  ( -1.011271242968688533, 0.7347315653655859258, -10.00000000000000000 ) ) ;
#42563 = VECTOR ( 'NONE', #9230, 1000.000000000000000 ) ;
#42564 = CARTESIAN_POINT ( 'NONE',  ( -126.6959734468149321, 1.749999999999997335, -79.18171244307201562 ) ) ;
#42565 = EDGE_CURVE ( 'NONE', #36027, #16851, #5902, .T. ) ;
#42566 = CARTESIAN_POINT ( 'NONE',  ( 31.94178169330218964, -9.256608784833820991, -3.760136334089591248 ) ) ;
#42567 = DIRECTION ( 'NONE',  ( -0.000000000000000000, -1.000000000000000000, -0.000000000000000000 ) ) ;
#42568 = VECTOR ( 'NONE', #36309, 1000.000000000000000 ) ;
#42569 = ORIENTED_EDGE ( 'NONE', *, *, #12383, .T. ) ;
#42570 = CARTESIAN_POINT ( 'NONE',  ( -46.76852358249001895, 17.86468378716740801, -9.367992836599951190 ) ) ;
#42571 = VERTEX_POINT ( 'NONE', #31424 ) ;
#42572 = CARTESIAN_POINT ( 'NONE',  ( 33.64889274059390090, -3.704246042440748621, 8.356839323120299312 ) ) ;
#42573 = ORIENTED_EDGE ( 'NONE', *, *, #37821, .F. ) ;
#42574 = DIRECTION ( 'NONE',  ( -1.156482317317871478E-16, -1.000000000000000000, 0.000000000000000000 ) ) ;
#42575 = LINE ( 'NONE', #26938, #1980 ) ;
#42576 = ORIENTED_EDGE ( 'NONE', *, *, #39681, .T. ) ;
#42577 = ORIENTED_EDGE ( 'NONE', *, *, #33079, .F. ) ;
#42578 = ORIENTED_EDGE ( 'NONE', *, *, #49624, .T. ) ;
#42579 = DIRECTION ( 'NONE',  ( 1.000000000000000000, 0.000000000000000000, 0.000000000000000000 ) ) ;
#42580 = DIRECTION ( 'NONE',  ( 0.000000000000000000, -2.537652627714642000E-15, -1.000000000000000000 ) ) ;
#42581 = ORIENTED_EDGE ( 'NONE', *, *, #22240, .F. ) ;
#42582 = FACE_OUTER_BOUND ( 'NONE', #28330, .T. ) ;
#42583 = CARTESIAN_POINT ( 'NONE',  ( 164.9999999999999716, 16.00000000000000000, 35.00000000000000000 ) ) ;
#42584 = CARTESIAN_POINT ( 'NONE',  ( 153.3040265531850537, 0.000000000000000000, 165.0000000000000000 ) ) ;
#42585 = VERTEX_POINT ( 'NONE', #11917 ) ;
#42586 = ORIENTED_EDGE ( 'NONE', *, *, #38526, .T. ) ;
#42587 = CYLINDRICAL_SURFACE ( 'NONE', #22634, 4.000000000000003553 ) ;
#42588 = AXIS2_PLACEMENT_3D ( 'NONE', #34923, #27961, #43598 ) ;
#42589 = ADVANCED_FACE ( 'NONE', ( #43208 ), #23715, .T. ) ;
#42590 = CARTESIAN_POINT ( 'NONE',  ( -114.9999999999987779, 17.00000000000000000, 5.000000000000004441 ) ) ;
#42591 = AXIS2_PLACEMENT_3D ( 'NONE', #1010, #35917, #32823 ) ;
#42592 = VECTOR ( 'NONE', #13176, 1000.000000000000000 ) ;
#42593 = ORIENTED_EDGE ( 'NONE', *, *, #16232, .F. ) ;
#42594 = DIRECTION ( 'NONE',  ( -0.000000000000000000, -1.000000000000000000, -0.000000000000000000 ) ) ;
#42595 = CARTESIAN_POINT ( 'NONE',  ( -115.0000000000000284, 16.00000000000000000, -90.00000000000000000 ) ) ;
#42596 = EDGE_LOOP ( 'NONE', ( #6788, #50068, #30609, #1965 ) ) ;
#42597 = PLANE ( 'NONE',  #2438 ) ;
#42598 = VECTOR ( 'NONE', #13259, 1000.000000000000000 ) ;
#42599 = DIRECTION ( 'NONE',  ( -0.000000000000000000, -0.000000000000000000, 1.000000000000000000 ) ) ;
#42600 = ORIENTED_EDGE ( 'NONE', *, *, #23556, .T. ) ;
#42601 = CARTESIAN_POINT ( 'NONE',  ( 191.5540265531850537, 1.025126265847089213, -160.9317124430720014 ) ) ;
#42602 = CARTESIAN_POINT ( 'NONE',  ( -48.77035878734830732, -11.70366853303726273, -8.466730184410787174 ) ) ;
#42603 = CARTESIAN_POINT ( 'NONE',  ( -210.0000000000000568, 0.000000000000000000, 122.5682875569279844 ) ) ;
#42604 = VECTOR ( 'NONE', #39336, 1000.000000000000000 ) ;
#42605 = CARTESIAN_POINT ( 'NONE',  ( 183.0000000000000568, 165.0000000000000000, 355.9999999999998863 ) ) ;
#42606 = ADVANCED_FACE ( 'NONE', ( #38361 ), #3173, .T. ) ;
#42607 = EDGE_CURVE ( 'NONE', #46138, #5590, #25541, .T. ) ;
#42608 = EDGE_LOOP ( 'NONE', ( #33676, #16318, #38505, #19780, #3601, #38340 ) ) ;
#42609 = CARTESIAN_POINT ( 'NONE',  ( 33.01266944765062306, -5.813986777101467496, 1.847720168420772691 ) ) ;
#42610 = CARTESIAN_POINT ( 'NONE',  ( 0.3370904143228947158, 0.2449105217885311492, 10.00000000000000000 ) ) ;
#42611 = CARTESIAN_POINT ( 'NONE',  ( 0.3862712429686978033, -1.188820645368937834, 10.00000000000000000 ) ) ;
#42612 = ORIENTED_EDGE ( 'NONE', *, *, #31926, .F. ) ;
#42613 = ORIENTED_EDGE ( 'NONE', *, *, #44807, .F. ) ;
#42614 = ADVANCED_FACE ( 'NONE', ( #27048 ), #42686, .F. ) ;
#42615 = DIRECTION ( 'NONE',  ( 0.9996489189823327681, -3.191891195797324659E-15, 0.02649601436921053890 ) ) ;
#42616 = ADVANCED_FACE ( 'NONE', ( #28065 ), #39889, .T. ) ;
#42617 = LINE ( 'NONE', #31091, #34341 ) ;
#42618 = FACE_OUTER_BOUND ( 'NONE', #45650, .T. ) ;
#42619 = CARTESIAN_POINT ( 'NONE',  ( -19.99999999999846523, 17.00000000000000000, 60.00000000000000000 ) ) ;
#42620 = DIRECTION ( 'NONE',  ( -1.000000000000000000, -0.000000000000000000, -0.000000000000000000 ) ) ;
#42621 = DIRECTION ( 'NONE',  ( -1.000000000000000000, -0.000000000000000000, -0.000000000000000000 ) ) ;
#42622 = ORIENTED_EDGE ( 'NONE', *, *, #12042, .F. ) ;
#42623 = EDGE_CURVE ( 'NONE', #14468, #9223, #28319, .T. ) ;
#42624 = CARTESIAN_POINT ( 'NONE',  ( 37.27397286063867199, -4.111076158911552092, 7.697694107796188234 ) ) ;
#42625 = CARTESIAN_POINT ( 'NONE',  ( 210.0000000000000568, 0.000000000000000000, 160.8182875569279702 ) ) ;
#42626 = CARTESIAN_POINT ( 'NONE',  ( -46.69597344681494633, 1.750000000000010214, -39.18171244307202983 ) ) ;
#42627 = CIRCLE ( 'NONE', #21323, 2.000000000000001776 ) ;
#42628 =( BOUNDED_CURVE ( )  B_SPLINE_CURVE ( 3, ( #34767, #3169, #19080, #30139 ),
 .UNSPECIFIED., .F., .F. ) 
 B_SPLINE_CURVE_WITH_KNOTS ( ( 4, 4 ),
 ( 3.141592653589793116, 4.712388980384689674 ),
 .UNSPECIFIED. ) 
 CURVE ( )  GEOMETRIC_REPRESENTATION_ITEM ( )  RATIONAL_B_SPLINE_CURVE ( ( 1.000000000000000000, 0.8047378541243649375, 0.8047378541243649375, 1.000000000000000000 ) ) 
 REPRESENTATION_ITEM ( '' )  );
#42629 = VECTOR ( 'NONE', #29842, 1000.000000000000227 ) ;
#42630 = CARTESIAN_POINT ( 'NONE',  ( 15.00000000000000000, -46.12433806312137108, -6.404467680894764925 ) ) ;
#42631 = VERTEX_POINT ( 'NONE', #880 ) ;
#42632 = CARTESIAN_POINT ( 'NONE',  ( 35.05402655318504657, 2.143131898507882349E-16, 165.0000000000000000 ) ) ;
#42633 = CARTESIAN_POINT ( 'NONE',  ( 1.011271242968694084, -0.7347315653655782652, 10.00000000000000000 ) ) ;
#42634 = ORIENTED_EDGE ( 'NONE', *, *, #26501, .F. ) ;
#42635 = VECTOR ( 'NONE', #30763, 1000.000000000000000 ) ;
#42636 = CARTESIAN_POINT ( 'NONE',  ( -14.99999999999812594, 16.00000000000000000, 65.00000000000000000 ) ) ;
#42637 = CYLINDRICAL_SURFACE ( 'NONE', #11840, 1.750000000000010214 ) ;
#42638 = VECTOR ( 'NONE', #24510, 1000.000000000000000 ) ;
#42639 = AXIS2_PLACEMENT_3D ( 'NONE', #1757, #17399, #33066 ) ;
#42640 = CARTESIAN_POINT ( 'NONE',  ( 115.0540265531850395, 2.143131898507847836E-16, -0.9317124430719969652 ) ) ;
#42641 = VERTEX_POINT ( 'NONE', #21116 ) ;
#42642 = CARTESIAN_POINT ( 'NONE',  ( -14.99999999999876366, 16.00000000000000000, 30.00000000000000000 ) ) ;
#42643 = DIRECTION ( 'NONE',  ( 0.000000000000000000, 0.000000000000000000, -1.000000000000000000 ) ) ;
#42644 = ORIENTED_EDGE ( 'NONE', *, *, #40157, .F. ) ;
#42645 = CARTESIAN_POINT ( 'NONE',  ( 2.500000000000003997, 194.9999999999999716, -224.9999999999999716 ) ) ;
#42646 = FACE_OUTER_BOUND ( 'NONE', #1815, .T. ) ;
#42647 = CARTESIAN_POINT ( 'NONE',  ( 27.33593271309472073, -41.94268121623323253, -9.367992836599951190 ) ) ;
#42648 =( BOUNDED_CURVE ( )  B_SPLINE_CURVE ( 3, ( #40031, #39025, #23867, #35435 ),
 .UNSPECIFIED., .F., .F. ) 
 B_SPLINE_CURVE_WITH_KNOTS ( ( 4, 4 ),
 ( 4.712388980384689674, 6.283185307179586232 ),
 .UNSPECIFIED. ) 
 CURVE ( )  GEOMETRIC_REPRESENTATION_ITEM ( )  RATIONAL_B_SPLINE_CURVE ( ( 1.000000000000000000, 0.8047378541243649375, 0.8047378541243649375, 1.000000000000000000 ) ) 
 REPRESENTATION_ITEM ( '' )  );
#42649 = ORIENTED_EDGE ( 'NONE', *, *, #25817, .F. ) ;
#42650 = VERTEX_POINT ( 'NONE', #1630 ) ;
#42651 = FACE_OUTER_BOUND ( 'NONE', #47185, .T. ) ;
#42652 = CARTESIAN_POINT ( 'NONE',  ( 0.4426377647354858835, 1.666766018367784596, 9.928159647716132241 ) ) ;
#42653 = ADVANCED_FACE ( 'NONE', ( #16524 ), #24478, .F. ) ;
#42654 = ORIENTED_EDGE ( 'NONE', *, *, #11243, .T. ) ;
#42655 = ORIENTED_EDGE ( 'NONE', *, *, #23388, .T. ) ;
#42656 = FACE_OUTER_BOUND ( 'NONE', #33516, .T. ) ;
#42657 = LINE ( 'NONE', #8543, #19357 ) ;
#42658 = PLANE ( 'NONE',  #40364 ) ;
#42659 = EDGE_LOOP ( 'NONE', ( #46329, #19009, #45300, #14647, #29298, #11942 ) ) ;
#42660 = CARTESIAN_POINT ( 'NONE',  ( -31.44259251615275019, -38.95901822126145220, -9.367992836599954742 ) ) ;
#42661 = VERTEX_POINT ( 'NONE', #47274 ) ;
#42662 = CARTESIAN_POINT ( 'NONE',  ( 0.3862712429686894766, -1.188820645368940276, 10.00000000000000000 ) ) ;
#42663 = LINE ( 'NONE', #45982, #39818 ) ;
#42664 = CIRCLE ( 'NONE', #19750, 2.000000000000001776 ) ;
#42665 = FACE_OUTER_BOUND ( 'NONE', #8295, .T. ) ;
#42666 = AXIS2_PLACEMENT_3D ( 'NONE', #11871, #20067, #12127 ) ;
#42667 = ORIENTED_EDGE ( 'NONE', *, *, #10352, .F. ) ;
#42668 = EDGE_LOOP ( 'NONE', ( #19329, #42297, #42343, #37367 ) ) ;
#42669 = VERTEX_POINT ( 'NONE', #20110 ) ;
#42670 = DIRECTION ( 'NONE',  ( 9.711650524620651178E-33, -1.223873602809432483E-48, 1.000000000000000000 ) ) ;
#42671 = DIRECTION ( 'NONE',  ( -0.000000000000000000, -0.000000000000000000, -1.000000000000000000 ) ) ;
#42672 = ORIENTED_EDGE ( 'NONE', *, *, #36269, .T. ) ;
#42673 = CARTESIAN_POINT ( 'NONE',  ( -88.44597344681497475, 0.000000000000000000, 39.06828755692795596 ) ) ;
#42674 = VECTOR ( 'NONE', #3772, 1000.000000000000000 ) ;
#42675 = ORIENTED_EDGE ( 'NONE', *, *, #28784, .T. ) ;
#42676 = B_SPLINE_CURVE_WITH_KNOTS ( 'NONE', 3,
 ( #50705, #31013, #42289, #34351 ),
 .UNSPECIFIED., .F., .F.,
 ( 4, 4 ),
 ( 2.453269466693398698E-18, 0.002466147708923231447 ),
 .UNSPECIFIED. ) ;
#42677 = CARTESIAN_POINT ( 'NONE',  ( 210.0000000000000568, 0.000000000000000000, 120.8182875569279702 ) ) ;
#42678 = VERTEX_POINT ( 'NONE', #24730 ) ;
#42679 = CARTESIAN_POINT ( 'NONE',  ( 153.3040265531850537, -1.750000000000009992, 0.8182875569279768335 ) ) ;
#42680 = LINE ( 'NONE', #5707, #32691 ) ;
#42681 = DIRECTION ( 'NONE',  ( -4.758098676964957447E-16, -1.000000000000000000, 7.143884938411937192E-48 ) ) ;
#42682 = LINE ( 'NONE', #3431, #44591 ) ;
#42683 = VERTEX_POINT ( 'NONE', #35799 ) ;
#42684 = ORIENTED_EDGE ( 'NONE', *, *, #16150, .T. ) ;
#42685 = ADVANCED_FACE ( 'NONE', ( #8826 ), #40127, .T. ) ;
#42686 = PLANE ( 'NONE',  #32104 ) ;
#42687 = CARTESIAN_POINT ( 'NONE',  ( -2.052549611693787135, 0.2039603569406744088, 9.894754715216729224 ) ) ;
#42688 = FACE_OUTER_BOUND ( 'NONE', #43659, .T. ) ;
#42689 = DIRECTION ( 'NONE',  ( -1.000000000000000000, 0.000000000000000000, 0.000000000000000000 ) ) ;
#42690 = DIRECTION ( 'NONE',  ( 0.000000000000000000, -0.3846153846153845812, -0.9230769230769231282 ) ) ;
#42691 = FACE_OUTER_BOUND ( 'NONE', #32463, .T. ) ;
#42692 = ORIENTED_EDGE ( 'NONE', *, *, #43048, .F. ) ;
#42693 = DIRECTION ( 'NONE',  ( 3.363195139050033768E-16, 0.7071067811865474617, 0.7071067811865475727 ) ) ;
#42694 = LINE ( 'NONE', #23980, #39445 ) ;
#42695 = AXIS2_PLACEMENT_3D ( 'NONE', #4197, #19833, #27030 ) ;
#42696 = VERTEX_POINT ( 'NONE', #28568 ) ;
#42697 = DIRECTION ( 'NONE',  ( -1.000000000000000000, -0.000000000000000000, -0.000000000000000000 ) ) ;
#42698 = DIRECTION ( 'NONE',  ( -1.000000000000000000, 0.000000000000000000, -4.758098658057970186E-16 ) ) ;
#42699 = DIRECTION ( 'NONE',  ( -1.000000000000000000, -0.000000000000000000, -0.000000000000000000 ) ) ;
#42700 = AXIS2_PLACEMENT_3D ( 'NONE', #35095, #46325, #42254 ) ;
#42701 = ORIENTED_EDGE ( 'NONE', *, *, #13283, .F. ) ;
#42702 = AXIS2_PLACEMENT_3D ( 'NONE', #34984, #27263, #39082 ) ;
#42703 = ORIENTED_EDGE ( 'NONE', *, *, #2638, .T. ) ;
#42704 = CYLINDRICAL_SURFACE ( 'NONE', #29165, 1.750000000000015543 ) ;
#42705 = CARTESIAN_POINT ( 'NONE',  ( 7.576114424932982594, -50.00000000000000711, 7.906207997025717304 ) ) ;
#42706 = ORIENTED_EDGE ( 'NONE', *, *, #10529, .F. ) ;
#42707 = EDGE_LOOP ( 'NONE', ( #22192, #14976, #31931, #20120, #25823, #13204, #30861, #45152 ) ) ;
#42708 = CARTESIAN_POINT ( 'NONE',  ( -126.6959734468149321, -1.749999999999997113, 40.81828755692798438 ) ) ;
#42709 = LINE ( 'NONE', #7584, #24948 ) ;
#42710 = LINE ( 'NONE', #42969, #20973 ) ;
#42711 = ORIENTED_EDGE ( 'NONE', *, *, #29133, .T. ) ;
#42712 = ORIENTED_EDGE ( 'NONE', *, *, #5109, .F. ) ;
#42713 = VERTEX_POINT ( 'NONE', #23964 ) ;
#42714 = LINE ( 'NONE', #18610, #25082 ) ;
#42715 = FACE_OUTER_BOUND ( 'NONE', #8373, .T. ) ;
#42716 = ORIENTED_EDGE ( 'NONE', *, *, #22712, .T. ) ;
#42717 = CARTESIAN_POINT ( 'NONE',  ( -119.9999999999990905, 17.00000000000000000, 0.000000000000000000 ) ) ;
#42718 = CARTESIAN_POINT ( 'NONE',  ( 356.0000000000000000, -174.9999999999999147, 343.9999999999998295 ) ) ;
#42719 = CARTESIAN_POINT ( 'NONE',  ( -164.9999999999981526, 17.00000000000000000, 65.00000000000000000 ) ) ;
#42720 = ORIENTED_EDGE ( 'NONE', *, *, #453, .F. ) ;
#42721 =( BOUNDED_CURVE ( )  B_SPLINE_CURVE ( 3, ( #23432, #30621, #12136, #4430 ),
 .UNSPECIFIED., .F., .F. ) 
 B_SPLINE_CURVE_WITH_KNOTS ( ( 4, 4 ),
 ( 3.141592653589793116, 4.712388980384689674 ),
 .UNSPECIFIED. ) 
 CURVE ( )  GEOMETRIC_REPRESENTATION_ITEM ( )  RATIONAL_B_SPLINE_CURVE ( ( 1.000000000000000000, 0.8047378541243649375, 0.8047378541243649375, 1.000000000000000000 ) ) 
 REPRESENTATION_ITEM ( '' )  );
#42722 = ORIENTED_EDGE ( 'NONE', *, *, #30594, .F. ) ;
#42723 = PLANE ( 'NONE',  #27900 ) ;
#42724 = DIRECTION ( 'NONE',  ( -0.000000000000000000, -0.000000000000000000, -1.000000000000000000 ) ) ;
#42725 = AXIS2_PLACEMENT_3D ( 'NONE', #9055, #24710, #12386 ) ;
#42726 = VECTOR ( 'NONE', #19904, 1000.000000000000000 ) ;
#42727 = CARTESIAN_POINT ( 'NONE',  ( 360.0000000000000000, 174.9999999999996589, -344.0000000000002842 ) ) ;
#42728 = ORIENTED_EDGE ( 'NONE', *, *, #33677, .F. ) ;
#42729 = VERTEX_POINT ( 'NONE', #31933 ) ;
#42730 = VERTEX_POINT ( 'NONE', #4959 ) ;
#42731 = LINE ( 'NONE', #7611, #14050 ) ;
#42732 = CARTESIAN_POINT ( 'NONE',  ( 169.0000000000000000, -9.999999999999953815, -99.00000000000014211 ) ) ;
#42733 = DIRECTION ( 'NONE',  ( 0.000000000000000000, -1.000000000000000000, 0.000000000000000000 ) ) ;
#42734 = EDGE_CURVE ( 'NONE', #12712, #16019, #12908, .T. ) ;
#42735 = VECTOR ( 'NONE', #12106, 1000.000000000000000 ) ;
#42736 = CARTESIAN_POINT ( 'NONE',  ( 23.29043492822826167, -24.10797434788167948, 1.847720168420772691 ) ) ;
#42737 = ORIENTED_EDGE ( 'NONE', *, *, #8791, .F. ) ;
#42738 = EDGE_CURVE ( 'NONE', #10420, #13192, #7902, .T. ) ;
#42739 = CARTESIAN_POINT ( 'NONE',  ( -49.75871208702130133, -40.58472229863598102, 5.000000000000000000 ) ) ;
#42740 = DIRECTION ( 'NONE',  ( 0.000000000000000000, 0.2223603367690632493, -0.9749645535258955054 ) ) ;
#42741 = CARTESIAN_POINT ( 'NONE',  ( 151.5540265531850537, 0.000000000000000000, -37.43171244307205825 ) ) ;
#42742 = EDGE_CURVE ( 'NONE', #5180, #23932, #13123, .T. ) ;
#42743 = CARTESIAN_POINT ( 'NONE',  ( 151.5540265531850537, 0.000000000000000000, 165.0000000000000000 ) ) ;
#42744 = EDGE_CURVE ( 'NONE', #26840, #12918, #47770, .T. ) ;
#42745 = EDGE_LOOP ( 'NONE', ( #21909, #17849, #29941, #5006 ) ) ;
#42746 = CARTESIAN_POINT ( 'NONE',  ( 3.087186397306452612, 2.514307945609885131, -2.642742795433417058E-16 ) ) ;
#42747 = CARTESIAN_POINT ( 'NONE',  ( -206.6959734468149463, 0.000000000000000000, 165.0000000000000000 ) ) ;
#42748 = CARTESIAN_POINT ( 'NONE',  ( -166.6959734468149463, -1.750000000000009992, -159.1817124430720298 ) ) ;
#42749 = ORIENTED_EDGE ( 'NONE', *, *, #13596, .F. ) ;
#42750 =( NAMED_UNIT ( * ) SI_UNIT ( $, .STERADIAN. ) SOLID_ANGLE_UNIT ( ) );
#42751 = CARTESIAN_POINT ( 'NONE',  ( -165.6708471809677974, 1.750000000000010214, 121.8434138227750623 ) ) ;
#42752 = EDGE_LOOP ( 'NONE', ( #23924, #23488, #39792, #1086, #38677, #6714 ) ) ;
#42753 = DIRECTION ( 'NONE',  ( 0.000000000000000000, 0.000000000000000000, -1.000000000000000000 ) ) ;
#42754 = CARTESIAN_POINT ( 'NONE',  ( 9.907356528111447957, -1.358045148324435347, 0.000000000000000000 ) ) ;
#42755 = DIRECTION ( 'NONE',  ( -1.000000000000000000, 0.000000000000000000, -0.000000000000000000 ) ) ;
#42756 = CARTESIAN_POINT ( 'NONE',  ( 21.20039782019597396, -30.97601161206925724, -2.490396854064192755 ) ) ;
#42757 = VECTOR ( 'NONE', #9735, 1000.000000000000000 ) ;
#42758 = ORIENTED_EDGE ( 'NONE', *, *, #6264, .F. ) ;
#42759 = CARTESIAN_POINT ( 'NONE',  ( 35.05402655318504657, 2.143131898507880377E-16, 2.568287556927978166 ) ) ;
#42760 = EDGE_CURVE ( 'NONE', #13377, #38138, #37067, .T. ) ;
#42762 = EDGE_LOOP ( 'NONE', ( #24195, #50271, #49382, #29295, #22137 ) ) ;
#42761 = EDGE_CURVE ( 'NONE', #25084, #3248, #16770, .T. ) ;
#42763 = ORIENTED_EDGE ( 'NONE', *, *, #38948, .T. ) ;
#42764 = VECTOR ( 'NONE', #25226, 1000.000000000000227 ) ;
#42765 = CARTESIAN_POINT ( 'NONE',  ( 14.49999999999999822, -46.01315789473684248, 5.916985404131814619 ) ) ;
#42766 = ADVANCED_FACE ( 'NONE', ( #39625 ), #32177, .T. ) ;
#42767 = ADVANCED_FACE ( 'NONE', ( #32674 ), #48272, .T. ) ;
#42768 = ORIENTED_EDGE ( 'NONE', *, *, #29267, .F. ) ;
#42769 = AXIS2_PLACEMENT_3D ( 'NONE', #42844, #12311, #50506 ) ;
#42770 = DIRECTION ( 'NONE',  ( 0.000000000000000000, 0.000000000000000000, 1.000000000000000000 ) ) ;
#42771 = FACE_OUTER_BOUND ( 'NONE', #2905, .T. ) ;
#42772 = UNCERTAINTY_MEASURE_WITH_UNIT (LENGTH_MEASURE( 1.000000000000000082E-05 ), #21041, 'distance_accuracy_value', 'NONE');
#42773 = EDGE_CURVE ( 'NONE', #12693, #14684, #39973, .T. ) ;
#42774 = EDGE_CURVE ( 'NONE', #44239, #13377, #29573, .T. ) ;
#42775 = CARTESIAN_POINT ( 'NONE',  ( 36.76598589393955052, 7.383243274241862331, -8.192531242611266862 ) ) ;
#42776 = ORIENTED_EDGE ( 'NONE', *, *, #8900, .T. ) ;
#42777 = DIRECTION ( 'NONE',  ( 0.000000000000000000, 2.969158215481698263E-48, -1.000000000000000000 ) ) ;
#42778 = CARTESIAN_POINT ( 'NONE',  ( 135.0000000000000000, 17.00000000000000000, -90.00000000000000000 ) ) ;
#42779 =( BOUNDED_CURVE ( )  B_SPLINE_CURVE ( 3, ( #33216, #21135, #39902, #32193 ),
 .UNSPECIFIED., .F., .F. ) 
 B_SPLINE_CURVE_WITH_KNOTS ( ( 4, 4 ),
 ( 1.570796326794896780, 3.141592653589460493 ),
 .UNSPECIFIED. ) 
 CURVE ( )  GEOMETRIC_REPRESENTATION_ITEM ( )  RATIONAL_B_SPLINE_CURVE ( ( 1.000000000000000000, 0.8047378541244434302, 0.8047378541244434302, 1.000000000000000000 ) ) 
 REPRESENTATION_ITEM ( '' )  );
#42780 = EDGE_LOOP ( 'NONE', ( #47238, #48286, #28982, #1841, #6281, #18661, #17537, #47051 ) ) ;
#42781 = CARTESIAN_POINT ( 'NONE',  ( 195.0540265531851105, 2.143131898507880377E-16, -160.9317124430720014 ) ) ;
#42782 = DIRECTION ( 'NONE',  ( 0.3090169943749447312, 0.9510565162951544194, 0.000000000000000000 ) ) ;
#42783 = EDGE_LOOP ( 'NONE', ( #25499, #30343, #13683, #8246, #36664, #30841 ) ) ;
#42784 = ORIENTED_EDGE ( 'NONE', *, *, #28015, .F. ) ;
#42785 = ORIENTED_EDGE ( 'NONE', *, *, #35916, .F. ) ;
#42786 = DIRECTION ( 'NONE',  ( -4.625929269271542120E-16, 0.000000000000000000, -1.000000000000000000 ) ) ;
#42787 =( BOUNDED_CURVE ( )  B_SPLINE_CURVE ( 3, ( #38116, #30404, #14494, #48646 ),
 .UNSPECIFIED., .F., .F. ) 
 B_SPLINE_CURVE_WITH_KNOTS ( ( 4, 4 ),
 ( 4.712388980384689674, 6.283185307179586232 ),
 .UNSPECIFIED. ) 
 CURVE ( )  GEOMETRIC_REPRESENTATION_ITEM ( )  RATIONAL_B_SPLINE_CURVE ( ( 1.000000000000000000, 0.8047378541243649375, 0.8047378541243649375, 1.000000000000000000 ) ) 
 REPRESENTATION_ITEM ( '' )  );
#42788 = VECTOR ( 'NONE', #48810, 1000.000000000000000 ) ;
#42789 = CARTESIAN_POINT ( 'NONE',  ( 168.9999999999999716, 175.0000000000000284, -358.0000000000001705 ) ) ;
#42790 = ORIENTED_EDGE ( 'NONE', *, *, #49084, .F. ) ;
#42791 = EDGE_CURVE ( 'NONE', #38537, #24864, #39667, .T. ) ;
#42792 = ADVANCED_FACE ( 'NONE', ( #48523 ), #5714, .T. ) ;
#42793 = CARTESIAN_POINT ( 'NONE',  ( 339.9999999999999432, 181.0000000000000284, -358.0000000000002274 ) ) ;
#42794 = CARTESIAN_POINT ( 'NONE',  ( 4.204997580903516941, 7.611558401714507482, 229.0000000000000000 ) ) ;
#42795 = CARTESIAN_POINT ( 'NONE',  ( -45.21167770612412085, -22.65616271077779942, 7.906207997025717304 ) ) ;
#42796 = EDGE_CURVE ( 'NONE', #47173, #23694, #41628, .T. ) ;
#42797 = CARTESIAN_POINT ( 'NONE',  ( -127.7210997126620242, 1.749999999999996225, -158.1565861772249377 ) ) ;
#42798 = CARTESIAN_POINT ( 'NONE',  ( -128.4459734468149179, 0.000000000000000000, 119.0682875569279986 ) ) ;
#42799 = EDGE_CURVE ( 'NONE', #6581, #35009, #26639, .T. ) ;
#42800 = CARTESIAN_POINT ( 'NONE',  ( 0.8433491450857230065, -0.9182416014173362395, 9.981352469109934233 ) ) ;
#42801 = VECTOR ( 'NONE', #35584, 1000.000000000000000 ) ;
#42802 = CARTESIAN_POINT ( 'NONE',  ( -86.69597344681494633, -1.750000000000010214, 40.81828755692798438 ) ) ;
#42803 = CARTESIAN_POINT ( 'NONE',  ( -208.4459734468149463, 0.000000000000000000, 165.0000000000000000 ) ) ;
#42804 = AXIS2_PLACEMENT_3D ( 'NONE', #28306, #12644, #8814 ) ;
#42805 = FACE_BOUND ( 'NONE', #5892, .T. ) ;
#42806 = CARTESIAN_POINT ( 'NONE',  ( -5.000000000000000000, -184.7999999999999545, -359.8000000000002387 ) ) ;
#42807 = VECTOR ( 'NONE', #43640, 1000.000000000000000 ) ;
#42808 = ADVANCED_FACE ( 'NONE', ( #9576 ), #22128, .F. ) ;
#42809 = ORIENTED_EDGE ( 'NONE', *, *, #22995, .T. ) ;
#42810 = FACE_OUTER_BOUND ( 'NONE', #45932, .T. ) ;
#42811 = VECTOR ( 'NONE', #38044, 999.9999999999998863 ) ;
#42812 = DIRECTION ( 'NONE',  ( -1.000000000000000000, -0.000000000000000000, -0.000000000000000000 ) ) ;
#42813 = CYLINDRICAL_SURFACE ( 'NONE', #44484, 1.750000000000008438 ) ;
#42814 = VERTEX_POINT ( 'NONE', #2132 ) ;
#42815 = DIRECTION ( 'NONE',  ( -1.586032880504786307E-16, 1.654361225106055350E-24, -1.000000000000000000 ) ) ;
#42816 = EDGE_CURVE ( 'NONE', #18177, #21391, #6707, .T. ) ;
#42817 = DIRECTION ( 'NONE',  ( -1.000000000000000000, 0.000000000000000000, 0.000000000000000000 ) ) ;
#42818 = CARTESIAN_POINT ( 'NONE',  ( -29.18392875402943432, -17.44843138996582965, 7.906207997025717304 ) ) ;
#42819 = CARTESIAN_POINT ( 'NONE',  ( -88.44597344681497475, 0.000000000000000000, 2.568287556928006143 ) ) ;
#42820 = CARTESIAN_POINT ( 'NONE',  ( 14.86945752723346637, 7.944783388879009145, 2.590526750877053086 ) ) ;
#42821 = ORIENTED_EDGE ( 'NONE', *, *, #17960, .T. ) ;
#42822 = ORIENTED_EDGE ( 'NONE', *, *, #41633, .F. ) ;
#42823 = LINE ( 'NONE', #26934, #32761 ) ;
#42824 = ADVANCED_FACE ( 'NONE', ( #2613 ), #37054, .F. ) ;
#42825 = ORIENTED_EDGE ( 'NONE', *, *, #7013, .T. ) ;
#42826 = DIRECTION ( 'NONE',  ( -4.759647537211363479E-16, 5.772796816983493182E-42, -1.000000000000000000 ) ) ;
#42827 = VECTOR ( 'NONE', #43925, 1000.000000000000000 ) ;
#42828 = ORIENTED_EDGE ( 'NONE', *, *, #27735, .T. ) ;
#42829 = VERTEX_POINT ( 'NONE', #32945 ) ;
#42830 = EDGE_CURVE ( 'NONE', #19115, #1912, #41258, .T. ) ;
#42831 = EDGE_CURVE ( 'NONE', #34859, #19251, #30092, .T. ) ;
#42832 = VERTEX_POINT ( 'NONE', #45693 ) ;
#42833 = CARTESIAN_POINT ( 'NONE',  ( 85.00000000000029843, 17.00000000000000000, -84.99999999999998579 ) ) ;
#42834 = ORIENTED_EDGE ( 'NONE', *, *, #18614, .F. ) ;
#42835 = CARTESIAN_POINT ( 'NONE',  ( -84.94597344681494633, 2.143131898507880377E-16, 122.5682875569279702 ) ) ;
#42836 = B_SPLINE_CURVE_WITH_KNOTS ( 'NONE', 3,
 ( #48947, #13835, #10009, #25669 ),
 .UNSPECIFIED., .F., .F.,
 ( 4, 4 ),
 ( 0.001937412222931662181, 0.003978261222109142140 ),
 .UNSPECIFIED. ) ;
#42837 = CARTESIAN_POINT ( 'NONE',  ( 183.0000000000000000, -184.9999999999999716, -344.0000000000003979 ) ) ;
#42838 = AXIS2_PLACEMENT_3D ( 'NONE', #17202, #32869, #36733 ) ;
#42839 = CARTESIAN_POINT ( 'NONE',  ( 0.000000000000000000, 165.2000000000000171, -340.2000000000001592 ) ) ;
#42840 = ORIENTED_EDGE ( 'NONE', *, *, #39405, .F. ) ;
#42841 = EDGE_CURVE ( 'NONE', #24864, #47066, #50086, .T. ) ;
#42842 = CARTESIAN_POINT ( 'NONE',  ( 14.49999999999999822, -46.01315789473684248, 5.916985404131813731 ) ) ;
#42843 = EDGE_CURVE ( 'NONE', #2131, #33144, #4598, .T. ) ;
#42844 = CARTESIAN_POINT ( 'NONE',  ( 169.0000000000000000, -9.999999999999953815, -99.00000000000014211 ) ) ;
#42845 = ADVANCED_FACE ( 'NONE', ( #44697 ), #25223, .T. ) ;
#42846 = ORIENTED_EDGE ( 'NONE', *, *, #46483, .F. ) ;
#42847 = CIRCLE ( 'NONE', #5167, 4.250000000000000000 ) ;
#42848 = CARTESIAN_POINT ( 'NONE',  ( -164.9459734468149463, 2.143131898507880377E-16, -37.43171244307205825 ) ) ;
#42849 = DIRECTION ( 'NONE',  ( -4.755310728521421461E-16, 0.000000000000000000, -1.000000000000000000 ) ) ;
#42850 = EDGE_LOOP ( 'NONE', ( #19832, #7189, #36887, #48644, #34357, #32053 ) ) ;
#42851 = PLANE ( 'NONE',  #7350 ) ;
#42852 = ADVANCED_FACE ( 'NONE', ( #33690 ), #49276, .T. ) ;
#42853 = DIRECTION ( 'NONE',  ( -0.000000000000000000, -1.544785076050074834E-48, -1.000000000000000000 ) ) ;
#42854 = B_SPLINE_SURFACE_WITH_KNOTS ( 'NONE', 3, 3, ( 
 ( #19428, #11732, #7128, #43719 ),
 ( #8588, #897, #30469, #16538 ),
 ( #32191, #3254, #22767, #18906 ),
 ( #34581, #46342, #7385, #5986 ) ),
 .UNSPECIFIED., .F., .F., .F.,
 ( 4, 4 ),
 ( 4, 4 ),
 ( 0.000000000000000000, 1.000000000000000000 ),
 ( 0.000000000000000000, 1.000000000000000000 ),
 .UNSPECIFIED. ) ;
#42855 = ORIENTED_EDGE ( 'NONE', *, *, #50050, .F. ) ;
#42856 = CARTESIAN_POINT ( 'NONE',  ( 0.9598058911017247619, 1.847159827636295937, 9.888808121373916293 ) ) ;
#42857 = CYLINDRICAL_SURFACE ( 'NONE', #33961, 1.750000000000036193 ) ;
#42858 = FACE_OUTER_BOUND ( 'NONE', #31697, .T. ) ;
#42859 = FACE_OUTER_BOUND ( 'NONE', #30008, .T. ) ;
#42860 = EDGE_CURVE ( 'NONE', #20632, #28535, #46447, .T. ) ;
#42861 = ORIENTED_EDGE ( 'NONE', *, *, #26127, .T. ) ;
#42862 = FACE_OUTER_BOUND ( 'NONE', #22382, .T. ) ;
#42863 = CARTESIAN_POINT ( 'NONE',  ( -126.6959734468149321, -1.749999999999996891, -159.1817124430720298 ) ) ;
#42864 = VERTEX_POINT ( 'NONE', #39307 ) ;
#42865 = ORIENTED_EDGE ( 'NONE', *, *, #8334, .T. ) ;
#42866 = DIRECTION ( 'NONE',  ( -0.2144099651976388021, 1.438973879383406636E-14, 0.9767437569925631058 ) ) ;
#42867 = CARTESIAN_POINT ( 'NONE',  ( 181.0000000000000000, -184.9999999999999716, -340.0000000000001705 ) ) ;
#42868 = CARTESIAN_POINT ( 'NONE',  ( -9.696760411816217839, -2.443938934554997999, 0.000000000000000000 ) ) ;
#42869 = CARTESIAN_POINT ( 'NONE',  ( 210.0000000000000568, 0.000000000000000000, -39.18171244307202983 ) ) ;
#42870 = VECTOR ( 'NONE', #34324, 1000.000000000000000 ) ;
#42871 = DIRECTION ( 'NONE',  ( -3.172065784643302499E-16, -1.000000000000000000, 2.537652627714642000E-15 ) ) ;
#42872 = CARTESIAN_POINT ( 'NONE',  ( 31.55402655318503236, 0.000000000000000000, -40.93171244307205825 ) ) ;
#42873 = ORIENTED_EDGE ( 'NONE', *, *, #7338, .F. ) ;
#42874 = CARTESIAN_POINT ( 'NONE',  ( 195.0540265531851105, -1.025126265847089657, 119.0682875569279560 ) ) ;
#42875 = CIRCLE ( 'NONE', #12556, 2.000000000000001776 ) ;
#42876 = CARTESIAN_POINT ( 'NONE',  ( -16.69947034530963847, 2.312583065866374632, 2.590526750877053086 ) ) ;
#42877 = DIRECTION ( 'NONE',  ( 1.000000000000000000, 0.000000000000000000, 0.000000000000000000 ) ) ;
#42878 = VECTOR ( 'NONE', #19802, 1000.000000000000000 ) ;
#42879 = ORIENTED_EDGE ( 'NONE', *, *, #3558, .T. ) ;
#42880 = PRESENTATION_STYLE_ASSIGNMENT (( #30341 ) ) ;
#42881 = ORIENTED_EDGE ( 'NONE', *, *, #464, .F. ) ;
#42882 = AXIS2_PLACEMENT_3D ( 'NONE', #29581, #3894, #30860 ) ;
#42883 = DIRECTION ( 'NONE',  ( 1.000000000000000000, 0.000000000000000000, 0.000000000000000000 ) ) ;
#42884 = CARTESIAN_POINT ( 'NONE',  ( -1.011271242968688533, 0.7347315653655859258, 10.00000000000000000 ) ) ;
#42885 = ORIENTED_EDGE ( 'NONE', *, *, #40386, .F. ) ;
#42886 = CARTESIAN_POINT ( 'NONE',  ( 30.00000000000123279, 16.00000000000000000, 30.00000000000000000 ) ) ;
#42887 = CARTESIAN_POINT ( 'NONE',  ( -1.011271242968693862, 0.7347315653655780432, -10.00000000000000000 ) ) ;
#42888 = CARTESIAN_POINT ( 'NONE',  ( 181.0000000000000000, -164.9999999999999432, 355.9999999999998863 ) ) ;
#42889 = DIRECTION ( 'NONE',  ( -0.000000000000000000, -0.000000000000000000, -1.000000000000000000 ) ) ;
#42890 = ORIENTED_EDGE ( 'NONE', *, *, #42761, .T. ) ;
#42891 = EDGE_CURVE ( 'NONE', #30805, #3733, #38836, .T. ) ;
#42892 = VECTOR ( 'NONE', #16817, 1000.000000000000000 ) ;
#42893 = DIRECTION ( 'NONE',  ( -1.000000000000000000, 0.000000000000000000, 0.000000000000000000 ) ) ;
#42894 = EDGE_CURVE ( 'NONE', #47864, #6375, #43543, .T. ) ;
#42895 = CARTESIAN_POINT ( 'NONE',  ( -126.6959734468149321, 1.749999999999996891, 160.8182875569279702 ) ) ;
#42896 = EDGE_LOOP ( 'NONE', ( #23815, #35886, #28580, #31524 ) ) ;
#42897 = LINE ( 'NONE', #27530, #21360 ) ;
#42898 = DIRECTION ( 'NONE',  ( 0.000000000000000000, -0.000000000000000000, 1.000000000000000000 ) ) ;
#42899 = DIRECTION ( 'NONE',  ( -1.000000000000000000, -0.000000000000000000, -0.000000000000000000 ) ) ;
#42900 = UNCERTAINTY_MEASURE_WITH_UNIT (LENGTH_MEASURE( 1.000000000000000082E-05 ), #50597, 'distance_accuracy_value', 'NONE');
#42901 = PLANE ( 'NONE',  #33259 ) ;
#42902 = VERTEX_POINT ( 'NONE', #50025 ) ;
#42903 = EDGE_CURVE ( 'NONE', #6362, #13604, #42118, .T. ) ;
#42904 = ORIENTED_EDGE ( 'NONE', *, *, #7899, .T. ) ;
#42905 = DIRECTION ( 'NONE',  ( -1.000000000000000000, 0.000000000000000000, 0.000000000000000000 ) ) ;
#42906 = ADVANCED_FACE ( 'NONE', ( #45946 ), #43148, .F. ) ;
#42907 = EDGE_CURVE ( 'NONE', #15777, #23917, #38805, .T. ) ;
#42908 = ORIENTED_EDGE ( 'NONE', *, *, #48474, .T. ) ;
#42909 = DIRECTION ( 'NONE',  ( -1.586032892321652236E-16, -1.000000000000000000, -2.288264760618012091E-48 ) ) ;
#42910 = DIRECTION ( 'NONE',  ( 0.000000000000000000, 0.000000000000000000, 1.000000000000000000 ) ) ;
#42911 = AXIS2_PLACEMENT_3D ( 'NONE', #8281, #36246, #35489 ) ;
#42912 = CARTESIAN_POINT ( 'NONE',  ( -165.6708471809677974, -1.750000000000009326, -158.1565861772249377 ) ) ;
#42913 = ORIENTED_EDGE ( 'NONE', *, *, #9010, .F. ) ;
#42914 = LINE ( 'NONE', #47245, #22700 ) ;
#42915 = VECTOR ( 'NONE', #1998, 1000.000000000000000 ) ;
#42916 = ORIENTED_EDGE ( 'NONE', *, *, #19516, .F. ) ;
#42917 = EDGE_CURVE ( 'NONE', #11294, #10604, #48750, .T. ) ;
#42918 = LINE ( 'NONE', #23689, #23868 ) ;
#42919 = COLOUR_RGB ( '',0.7921568627450980005, 0.8196078431372548767, 0.9333333333333333481 ) ;
#42920 = CARTESIAN_POINT ( 'NONE',  ( -6.880036658038818587, -197.4999999999999432, -228.6347188485896140 ) ) ;
#42921 = CIRCLE ( 'NONE', #46994, 2.000000000000001776 ) ;
#42922 = CARTESIAN_POINT ( 'NONE',  ( 1.249999999999999778, -0.000000000000000000, -10.00000000000000000 ) ) ;
#42923 = ORIENTED_EDGE ( 'NONE', *, *, #6431, .F. ) ;
#42924 = ORIENTED_EDGE ( 'NONE', *, *, #37108, .F. ) ;
#42925 = ORIENTED_EDGE ( 'NONE', *, *, #35137, .F. ) ;
#42926 = CARTESIAN_POINT ( 'NONE',  ( 339.9999999999999432, -182.9999999999999716, -344.0000000000001705 ) ) ;
#42927 = DIRECTION ( 'NONE',  ( 3.172065745548403743E-16, 1.000000000000000000, 0.000000000000000000 ) ) ;
#42928 = ORIENTED_EDGE ( 'NONE', *, *, #49840, .T. ) ;
#42929 = FACE_OUTER_BOUND ( 'NONE', #40984, .T. ) ;
#42930 = ORIENTED_EDGE ( 'NONE', *, *, #41224, .F. ) ;
#42931 = CARTESIAN_POINT ( 'NONE',  ( 181.0000000000000000, -270.4999999999999432, -349.9999999999999432 ) ) ;
#42932 = EDGE_LOOP ( 'NONE', ( #31654, #17394, #38352, #33657 ) ) ;
#42933 = DIRECTION ( 'NONE',  ( -1.586032880504786307E-16, 1.654361225106055350E-24, -1.000000000000000000 ) ) ;
#42934 =( BOUNDED_CURVE ( )  B_SPLINE_CURVE ( 3, ( #3787, #19437, #35116, #50691 ),
 .UNSPECIFIED., .F., .F. ) 
 B_SPLINE_CURVE_WITH_KNOTS ( ( 4, 4 ),
 ( 3.141592653589793116, 4.712388980384689674 ),
 .UNSPECIFIED. ) 
 CURVE ( )  GEOMETRIC_REPRESENTATION_ITEM ( )  RATIONAL_B_SPLINE_CURVE ( ( 1.000000000000000000, 0.8047378541243649375, 0.8047378541243649375, 1.000000000000000000 ) ) 
 REPRESENTATION_ITEM ( '' )  );
#42935 = CARTESIAN_POINT ( 'NONE',  ( 14.48769039275578407, 30.44468701195595983, 8.807470649214879543 ) ) ;
#42936 = FACE_BOUND ( 'NONE', #3262, .T. ) ;
#42937 = VECTOR ( 'NONE', #49263, 1000.000000000000000 ) ;
#42938 = CARTESIAN_POINT ( 'NONE',  ( 1.249999999999999778, -0.000000000000000000, -3.333333333333333481 ) ) ;
#42939 = EDGE_LOOP ( 'NONE', ( #40450, #27615, #28411, #49053 ) ) ;
#42940 = ORIENTED_EDGE ( 'NONE', *, *, #12797, .T. ) ;
#42941 = CARTESIAN_POINT ( 'NONE',  ( 181.0000000000000000, -270.5000000000000000, -114.9999999999999147 ) ) ;
#42942 =( BOUNDED_CURVE ( )  B_SPLINE_CURVE ( 3, ( #19201, #4334, #35148, #46623 ),
 .UNSPECIFIED., .F., .F. ) 
 B_SPLINE_CURVE_WITH_KNOTS ( ( 4, 4 ),
 ( 0.000000000000000000, 1.570796326794896780 ),
 .UNSPECIFIED. ) 
 CURVE ( )  GEOMETRIC_REPRESENTATION_ITEM ( )  RATIONAL_B_SPLINE_CURVE ( ( 1.000000000000000000, 0.8047378541243649375, 0.8047378541243649375, 1.000000000000000000 ) ) 
 REPRESENTATION_ITEM ( '' )  );
#42943 = CARTESIAN_POINT ( 'NONE',  ( -14.99999999999876366, 16.00000000000000000, 30.00000000000000000 ) ) ;
#42944 = CARTESIAN_POINT ( 'NONE',  ( 167.5000000000000000, -69.93075758371368522, -120.5992382549688671 ) ) ;
#42945 = EDGE_CURVE ( 'NONE', #11648, #49618, #34970, .T. ) ;
#42946 = CARTESIAN_POINT ( 'NONE',  ( -5.000000000000000000, -184.7999999999999545, 340.1999999999997044 ) ) ;
#42947 = AXIS2_PLACEMENT_3D ( 'NONE', #38960, #8414, #23553 ) ;
#42948 = CARTESIAN_POINT ( 'NONE',  ( 36.44255557191966943, 8.993813888722351990, -5.338708898921616708 ) ) ;
#42949 = ORIENTED_EDGE ( 'NONE', *, *, #41265, .T. ) ;
#42950 = CIRCLE ( 'NONE', #20838, 2.000000000000001776 ) ;
#42951 = DIRECTION ( 'NONE',  ( 0.000000000000000000, 0.000000000000000000, 1.000000000000000000 ) ) ;
#42952 =( BOUNDED_CURVE ( )  B_SPLINE_CURVE ( 3, ( #25026, #47569, #12705, #24515 ),
 .UNSPECIFIED., .F., .F. ) 
 B_SPLINE_CURVE_WITH_KNOTS ( ( 4, 4 ),
 ( 4.712388980384689674, 6.283185307179586232 ),
 .UNSPECIFIED. ) 
 CURVE ( )  GEOMETRIC_REPRESENTATION_ITEM ( )  RATIONAL_B_SPLINE_CURVE ( ( 1.000000000000000000, 0.8047378541243649375, 0.8047378541243649375, 1.000000000000000000 ) ) 
 REPRESENTATION_ITEM ( '' )  );
#42953 = LINE ( 'NONE', #18835, #7467 ) ;
#42954 = AXIS2_PLACEMENT_3D ( 'NONE', #47437, #31340, #15934 ) ;
#42955 = EDGE_LOOP ( 'NONE', ( #10734, #22923, #20504, #38330 ) ) ;
#42956 = DIRECTION ( 'NONE',  ( 0.000000000000000000, -2.969158215481698263E-48, 1.000000000000000000 ) ) ;
#42957 = CARTESIAN_POINT ( 'NONE',  ( -128.4459734468149463, -1.025126265847081886, 119.0682875569279702 ) ) ;
#42958 = DIRECTION ( 'NONE',  ( 4.379057701015053347E-47, -1.000000000000000000, 2.537652627714642000E-15 ) ) ;
#42959 = ORIENTED_EDGE ( 'NONE', *, *, #46280, .F. ) ;
#42960 = PRODUCT_DEFINITION_SHAPE ( 'NONE', 'NONE',  #50738 ) ;
#42961 = ORIENTED_EDGE ( 'NONE', *, *, #46197, .T. ) ;
#42962 = CARTESIAN_POINT ( 'NONE',  ( 155.0540265531850537, 2.143131898507880377E-16, 82.56828755692798438 ) ) ;
#42963 = CARTESIAN_POINT ( 'NONE',  ( -4.672045878990125800, 33.19353511768168374, 1.847720168420772691 ) ) ;
#42964 = VECTOR ( 'NONE', #53, 1000.000000000000000 ) ;
#42965 = ORIENTED_EDGE ( 'NONE', *, *, #1217, .F. ) ;
#42966 = ORIENTED_EDGE ( 'NONE', *, *, #20417, .F. ) ;
#42967 = CARTESIAN_POINT ( 'NONE',  ( -45.64490844644706158, -21.32281559348763977, 8.807470649214879543 ) ) ;
#42968 = CARTESIAN_POINT ( 'NONE',  ( -8.277096487746778308, 33.14818118907697198, 7.455576670931136185 ) ) ;
#42969 = CARTESIAN_POINT ( 'NONE',  ( 210.0000000000000568, 2.143131898507881116E-16, 39.06828755692797728 ) ) ;
#42970 = FACE_OUTER_BOUND ( 'NONE', #10489, .T. ) ;
#42971 = ORIENTED_EDGE ( 'NONE', *, *, #16285, .F. ) ;
#42972 = VECTOR ( 'NONE', #46628, 1000.000000000000000 ) ;
#42973 = EDGE_LOOP ( 'NONE', ( #9168, #48731, #26481, #25712 ) ) ;
#42974 = EDGE_CURVE ( 'NONE', #36777, #4637, #3220, .T. ) ;
#42975 = ORIENTED_EDGE ( 'NONE', *, *, #46513, .T. ) ;
#42976 = B_SPLINE_CURVE_WITH_KNOTS ( 'NONE', 3,
 ( #43575, #11075, #8445, #45937 ),
 .UNSPECIFIED., .F., .F.,
 ( 4, 4 ),
 ( 0.0009679537044784938989, 0.001281751046851235375 ),
 .UNSPECIFIED. ) ;
#42977 = CARTESIAN_POINT ( 'NONE',  ( -208.4459734468149463, 0.000000000000000000, 165.0000000000000000 ) ) ;
#42978 = CARTESIAN_POINT ( 'NONE',  ( 0.000000000000000000, 17.00000000000000000, 0.000000000000000000 ) ) ;
#42979 = ORIENTED_EDGE ( 'NONE', *, *, #33053, .T. ) ;
#42980 = CARTESIAN_POINT ( 'NONE',  ( 6.875132362119187768, -50.00000000000000711, 8.356839323120299312 ) ) ;
#42981 = DIRECTION ( 'NONE',  ( 1.000000000000000000, 0.000000000000000000, 0.000000000000000000 ) ) ;
#42982 = CARTESIAN_POINT ( 'NONE',  ( 21.17460298198255231, 30.99364813079834491, -3.721387749823085400 ) ) ;
#42983 = CIRCLE ( 'NONE', #42138, 4.000000000000003553 ) ;
#42984 = ORIENTED_EDGE ( 'NONE', *, *, #34567, .T. ) ;
#42985 = ORIENTED_EDGE ( 'NONE', *, *, #36494, .F. ) ;
#42986 = CARTESIAN_POINT ( 'NONE',  ( 355.9999999999998295, -165.0000000000001137, -108.0000000000002132 ) ) ;
#42987 = DIRECTION ( 'NONE',  ( -1.000000000000000000, -0.000000000000000000, -0.000000000000000000 ) ) ;
#42988 = CARTESIAN_POINT ( 'NONE',  ( 2.948105490344985480, 9.555557232197198658, 9.282506307616484875 ) ) ;
#42989 = UNCERTAINTY_MEASURE_WITH_UNIT (LENGTH_MEASURE( 1.000000000000000082E-05 ), #15335, 'distance_accuracy_value', 'NONE');
#42990 = EDGE_LOOP ( 'NONE', ( #39983, #38444, #42821, #12790 ) ) ;
#42991 = VERTEX_POINT ( 'NONE', #23395 ) ;
#42992 = AXIS2_PLACEMENT_3D ( 'NONE', #41291, #22545, #45361 ) ;
#42993 = DIRECTION ( 'NONE',  ( 0.000000000000000000, 0.000000000000000000, -1.000000000000000000 ) ) ;
#42994 =( NAMED_UNIT ( * ) SI_UNIT ( $, .STERADIAN. ) SOLID_ANGLE_UNIT ( ) );
#42995 = ORIENTED_EDGE ( 'NONE', *, *, #7697, .T. ) ;
#42996 = CARTESIAN_POINT ( 'NONE',  ( 210.0000000000000568, 2.143131898507881856E-16, 119.0682875569279560 ) ) ;
#42997 = CARTESIAN_POINT ( 'NONE',  ( 35.05402655318504657, 2.143131898507880377E-16, -117.4317124430720156 ) ) ;
#42998 = DIRECTION ( 'NONE',  ( 0.000000000000000000, 5.664403186863042467E-17, 1.000000000000000000 ) ) ;
#42999 = CARTESIAN_POINT ( 'NONE',  ( 339.9999999999999432, -168.9999999999999432, -340.0000000000001705 ) ) ;
#43000 = ORIENTED_EDGE ( 'NONE', *, *, #11177, .F. ) ;
#43001 = CARTESIAN_POINT ( 'NONE',  ( 31.55402655318503236, 0.000000000000000000, 42.56828755692798438 ) ) ;
#43002 = CARTESIAN_POINT ( 'NONE',  ( 339.9999999999998863, -183.3431457505077731, -358.3431457505079720 ) ) ;
#43003 = DIRECTION ( 'NONE',  ( -0.000000000000000000, -0.000000000000000000, -1.000000000000000000 ) ) ;
#43004 = EDGE_CURVE ( 'NONE', #23447, #38333, #8501, .T. ) ;
#43005 = CARTESIAN_POINT ( 'NONE',  ( -0.1287570809895658697, 0.3962735484563123523, -10.00000000000000000 ) ) ;
#43006 = VECTOR ( 'NONE', #45772, 1000.000000000000000 ) ;
#43007 = AXIS2_PLACEMENT_3D ( 'NONE', #13608, #29264, #44880 ) ;
#43008 = ORIENTED_EDGE ( 'NONE', *, *, #40185, .F. ) ;
#43009 = CARTESIAN_POINT ( 'NONE',  ( 4.997594231923199182, 3.246827887979424787, -2.642742795433417058E-16 ) ) ;
#43010 = DIRECTION ( 'NONE',  ( -1.000000000000000000, 0.000000000000000000, 0.000000000000000000 ) ) ;
#43011 = CARTESIAN_POINT ( 'NONE',  ( -168.4459734468149747, -1.025126265847089213, -160.9317124430720014 ) ) ;
#43012 = ORIENTED_EDGE ( 'NONE', *, *, #3670, .T. ) ;
#43013 = FACE_OUTER_BOUND ( 'NONE', #5002, .T. ) ;
#43014 = AXIS2_PLACEMENT_3D ( 'NONE', #41374, #1626, #6468 ) ;
#43015 = CARTESIAN_POINT ( 'NONE',  ( 240.0000000000000000, -175.0000000000000000, 32.29650858650035161 ) ) ;
#43016 = VECTOR ( 'NONE', #13916, 1000.000000000000000 ) ;
#43017 = ORIENTED_EDGE ( 'NONE', *, *, #34312, .T. ) ;
#43018 = CARTESIAN_POINT ( 'NONE',  ( -114.9999999999991047, 17.00000000000000000, 0.000000000000000000 ) ) ;
#43019 = FACE_OUTER_BOUND ( 'NONE', #29239, .T. ) ;
#43020 = CARTESIAN_POINT ( 'NONE',  ( -87.72109971266203843, 1.750000000000009548, -40.20683870891912193 ) ) ;
#43021 = VERTEX_POINT ( 'NONE', #14676 ) ;
#43022 = CARTESIAN_POINT ( 'NONE',  ( 185.0000000000000284, -174.9999999999999716, -99.00000000000014211 ) ) ;
#43023 = ORIENTED_EDGE ( 'NONE', *, *, #35697, .T. ) ;
#43024 = ORIENTED_EDGE ( 'NONE', *, *, #21202, .F. ) ;
#43025 = VECTOR ( 'NONE', #3164, 1000.000000000000000 ) ;
#43026 = PLANE ( 'NONE',  #31637 ) ;
#43027 = DIRECTION ( 'NONE',  ( 1.000000000000000000, 0.000000000000000000, 3.469446951953611033E-15 ) ) ;
#43028 = ORIENTED_EDGE ( 'NONE', *, *, #5823, .T. ) ;
#43029 = CARTESIAN_POINT ( 'NONE',  ( 2.391286777838985245, -5.398370916123746532, 9.586754400234157814 ) ) ;
#43030 = CARTESIAN_POINT ( 'NONE',  ( -8.445973446814914354, 0.000000000000000000, 162.5682875569279702 ) ) ;
#43031 =( BOUNDED_CURVE ( )  B_SPLINE_CURVE ( 3, ( #6350, #36679, #21997, #9186 ),
 .UNSPECIFIED., .F., .F. ) 
 B_SPLINE_CURVE_WITH_KNOTS ( ( 4, 4 ),
 ( 1.570796326794896558, 3.141592653589793116 ),
 .UNSPECIFIED. ) 
 CURVE ( )  GEOMETRIC_REPRESENTATION_ITEM ( )  RATIONAL_B_SPLINE_CURVE ( ( 1.000000000000000000, 0.8047378541243649375, 0.8047378541243649375, 1.000000000000000000 ) ) 
 REPRESENTATION_ITEM ( '' )  );
#43032 = ADVANCED_FACE ( 'NONE', ( #46951 ), #41288, .T. ) ;
#43033 = CARTESIAN_POINT ( 'NONE',  ( 0.6812130152897633018, 2.552013566577088888, 9.847478321177755234 ) ) ;
#43034 = EDGE_LOOP ( 'NONE', ( #7487, #38324, #45692, #34926, #33667, #7641 ) ) ;
#43035 = CYLINDRICAL_SURFACE ( 'NONE', #19245, 1.750000000000015543 ) ;
#43036 = LINE ( 'NONE', #14837, #6228 ) ;
#43037 = CARTESIAN_POINT ( 'NONE',  ( 10.00000000000000000, -250.0000000000000000, 225.0000000000000000 ) ) ;
#43038 = EDGE_LOOP ( 'NONE', ( #12445, #15353, #20455, #33789, #48477, #35233, #37036, #14335 ) ) ;
#43039 = DIRECTION ( 'NONE',  ( 1.000000000000000000, 0.000000000000000000, 0.000000000000000000 ) ) ;
#43040 = CARTESIAN_POINT ( 'NONE',  ( -22.82242230425432439, -2.816136035261162185, 230.0000000000000000 ) ) ;
#43041 = ORIENTED_EDGE ( 'NONE', *, *, #25208, .F. ) ;
#43042 = VECTOR ( 'NONE', #9192, 1000.000000000000000 ) ;
#43043 = ORIENTED_EDGE ( 'NONE', *, *, #41582, .T. ) ;
#43044 = VERTEX_POINT ( 'NONE', #5145 ) ;
#43045 = LINE ( 'NONE', #11510, #6569 ) ;
#43046 = EDGE_CURVE ( 'NONE', #4462, #34536, #9009, .T. ) ;
#43047 = AXIS2_PLACEMENT_3D ( 'NONE', #5709, #8819, #36030 ) ;
#43048 = EDGE_CURVE ( 'NONE', #5075, #29454, #12339, .T. ) ;
#43049 = LINE ( 'NONE', #7418, #2901 ) ;
#43050 = ORIENTED_EDGE ( 'NONE', *, *, #13329, .F. ) ;
#43051 = CARTESIAN_POINT ( 'NONE',  ( 2.538055338523177440, 50.00000000000000711, -9.367992836599954742 ) ) ;
#43052 = DIRECTION ( 'NONE',  ( 0.000000000000000000, 0.000000000000000000, 1.000000000000000000 ) ) ;
#43053 = EDGE_CURVE ( 'NONE', #22708, #28480, #4150, .T. ) ;
#43054 = FACE_OUTER_BOUND ( 'NONE', #5624, .T. ) ;
#43055 = VECTOR ( 'NONE', #19522, 1000.000000000000000 ) ;
#43056 = PLANE ( 'NONE',  #48893 ) ;
#43057 = CARTESIAN_POINT ( 'NONE',  ( -1.011271242968687867, 0.7347315653655861478, 9.972675548442463622 ) ) ;
#43058 = CARTESIAN_POINT ( 'NONE',  ( -64.99999999999846523, 16.00000000000000000, 35.00000000000000000 ) ) ;
#43059 = AXIS2_PLACEMENT_3D ( 'NONE', #30135, #17820, #10122 ) ;
#43060 = VECTOR ( 'NONE', #11262, 1000.000000000000000 ) ;
#43061 = CARTESIAN_POINT ( 'NONE',  ( -2.536646476037189846, -2.794100479408525128, 9.865049507598756762 ) ) ;
#43062 = DIRECTION ( 'NONE',  ( -0.000000000000000000, -0.000000000000000000, -1.000000000000000000 ) ) ;
#43063 = DIRECTION ( 'NONE',  ( -1.000000000000000000, 0.000000000000000000, -0.000000000000000000 ) ) ;
#43064 = CARTESIAN_POINT ( 'NONE',  ( -165.3973046169136012, -98.56198943095992604, -17.65743994998275213 ) ) ;
#43065 = EDGE_CURVE ( 'NONE', #20271, #11044, #44383, .T. ) ;
#43066 = EDGE_CURVE ( 'NONE', #3216, #7644, #28261, .T. ) ;
#43067 = AXIS2_PLACEMENT_3D ( 'NONE', #14487, #25280, #9878 ) ;
#43068 = ORIENTED_EDGE ( 'NONE', *, *, #5417, .T. ) ;
#43069 = AXIS2_PLACEMENT_3D ( 'NONE', #18596, #37633, #34273 ) ;
#43070 = CARTESIAN_POINT ( 'NONE',  ( -7.721099712662037540, 1.750000000000023315, 81.84341382277507648 ) ) ;
#43071 = DIRECTION ( 'NONE',  ( -1.000000000000000000, -0.000000000000000000, -0.000000000000000000 ) ) ;
#43072 = EDGE_CURVE ( 'NONE', #2551, #11678, #43381, .T. ) ;
#43073 = EDGE_CURVE ( 'NONE', #49857, #50159, #20299, .T. ) ;
#43074 = FACE_OUTER_BOUND ( 'NONE', #2848, .T. ) ;
#43075 = CARTESIAN_POINT ( 'NONE',  ( 80.00000000000216005, 17.00000000000000000, 95.00000000000000000 ) ) ;
#43076 = VERTEX_POINT ( 'NONE', #9258 ) ;
#43077 = CYLINDRICAL_SURFACE ( 'NONE', #14699, 1.750000000000015543 ) ;
#43078 = EDGE_CURVE ( 'NONE', #22969, #27259, #44137, .T. ) ;
#43079 = LINE ( 'NONE', #43324, #13003 ) ;
#43080 = DIRECTION ( 'NONE',  ( -0.000000000000000000, -1.000000000000000000, -0.000000000000000000 ) ) ;
#43081 = CARTESIAN_POINT ( 'NONE',  ( -34.08355720199904226, 2.371364769369340042, 7.455576670931136185 ) ) ;
#43082 = VERTEX_POINT ( 'NONE', #47703 ) ;
#43083 = AXIS2_PLACEMENT_3D ( 'NONE', #43106, #19757, #46912 ) ;
#43084 = DIRECTION ( 'NONE',  ( -6.938893903907233900E-15, 0.000000000000000000, 1.000000000000000000 ) ) ;
#43085 = VERTEX_POINT ( 'NONE', #40313 ) ;
#43086 = CARTESIAN_POINT ( 'NONE',  ( 35.05402655318504657, 2.143131898507880377E-16, 165.0000000000000000 ) ) ;
#43087 = VECTOR ( 'NONE', #407, 1000.000000000000000 ) ;
#43088 = EDGE_LOOP ( 'NONE', ( #32982, #15957, #21163, #16548 ) ) ;
#43089 = FACE_OUTER_BOUND ( 'NONE', #21885, .T. ) ;
#43090 = CARTESIAN_POINT ( 'NONE',  ( 0.000000000000000000, 181.0000000000000284, 355.9999999999997726 ) ) ;
#43091 = VECTOR ( 'NONE', #46885, 1000.000000000000000 ) ;
#43092 = ORIENTED_EDGE ( 'NONE', *, *, #41569, .T. ) ;
#43093 = CARTESIAN_POINT ( 'NONE',  ( 214.9999999999999432, 164.9999999999999716, 111.9999999999999858 ) ) ;
#43094 = EDGE_CURVE ( 'NONE', #24059, #14851, #16695, .T. ) ;
#43095 = ORIENTED_EDGE ( 'NONE', *, *, #42192, .T. ) ;
#43096 =( BOUNDED_CURVE ( )  B_SPLINE_CURVE ( 3, ( #33407, #48977, #9284, #25695 ),
 .UNSPECIFIED., .F., .F. ) 
 B_SPLINE_CURVE_WITH_KNOTS ( ( 4, 4 ),
 ( 4.712388980384689674, 6.283185307179586232 ),
 .UNSPECIFIED. ) 
 CURVE ( )  GEOMETRIC_REPRESENTATION_ITEM ( )  RATIONAL_B_SPLINE_CURVE ( ( 1.000000000000000000, 0.8047378541243649375, 0.8047378541243649375, 1.000000000000000000 ) ) 
 REPRESENTATION_ITEM ( '' )  );
#43097 = VECTOR ( 'NONE', #36130, 1000.000000000000000 ) ;
#43098 = EDGE_CURVE ( 'NONE', #48433, #31642, #8513, .T. ) ;
#43099 = EDGE_CURVE ( 'NONE', #38145, #29600, #16204, .T. ) ;
#43100 = ORIENTED_EDGE ( 'NONE', *, *, #12335, .T. ) ;
#43101 = LINE ( 'NONE', #4107, #38523 ) ;
#43102 = DIRECTION ( 'NONE',  ( -1.000000000000000000, -0.000000000000000000, -0.000000000000000000 ) ) ;
#43103 =( GEOMETRIC_REPRESENTATION_CONTEXT ( 3 ) GLOBAL_UNCERTAINTY_ASSIGNED_CONTEXT ( ( #32303 ) ) GLOBAL_UNIT_ASSIGNED_CONTEXT ( ( #49817, #35019, #42168 ) ) REPRESENTATION_CONTEXT ( 'NONE', 'WORKASPACE' ) );
#43104 = ORIENTED_EDGE ( 'NONE', *, *, #15333, .T. ) ;
#43105 = CARTESIAN_POINT ( 'NONE',  ( -208.4459734468149463, 0.000000000000000000, -165.0000000000000000 ) ) ;
#43106 = CARTESIAN_POINT ( 'NONE',  ( 0.000000000000000000, 0.000000000000000000, 0.000000000000000000 ) ) ;
#43107 = EDGE_CURVE ( 'NONE', #29740, #8815, #13727, .T. ) ;
#43108 = DIRECTION ( 'NONE',  ( -1.000000000000000000, 0.000000000000000000, 0.000000000000000000 ) ) ;
#43109 =( BOUNDED_CURVE ( )  B_SPLINE_CURVE ( 3, ( #12913, #17283, #1392, #44209 ),
 .UNSPECIFIED., .F., .F. ) 
 B_SPLINE_CURVE_WITH_KNOTS ( ( 4, 4 ),
 ( 4.712388980384689674, 6.283185307179586232 ),
 .UNSPECIFIED. ) 
 CURVE ( )  GEOMETRIC_REPRESENTATION_ITEM ( )  RATIONAL_B_SPLINE_CURVE ( ( 1.000000000000000000, 0.8047378541243649375, 0.8047378541243649375, 1.000000000000000000 ) ) 
 REPRESENTATION_ITEM ( '' )  );
#43110 = VERTEX_POINT ( 'NONE', #19790 ) ;
#43111 = DIRECTION ( 'NONE',  ( -1.000000000000000000, -0.000000000000000000, -0.000000000000000000 ) ) ;
#43112 = EDGE_CURVE ( 'NONE', #33150, #27796, #31620, .T. ) ;
#43113 = AXIS2_PLACEMENT_3D ( 'NONE', #35619, #31255, #6939 ) ;
#43114 = CARTESIAN_POINT ( 'NONE',  ( 8.176860274785711979, -5.756644512789521606, 9.282506307616484875 ) ) ;
#43115 = VERTEX_POINT ( 'NONE', #27750 ) ;
#43116 = CARTESIAN_POINT ( 'NONE',  ( 6.174150299305392053, -33.14591993373988998, 8.807470649214879543 ) ) ;
#43117 = LINE ( 'NONE', #16182, #44174 ) ;
#43118 = ORIENTED_EDGE ( 'NONE', *, *, #12430, .F. ) ;
#43119 = CARTESIAN_POINT ( 'NONE',  ( 1.468446590252912465, 0.3226319952343980058, 9.953784399990622589 ) ) ;
#43120 = PLANE ( 'NONE',  #16111 ) ;
#43121 = ORIENTED_EDGE ( 'NONE', *, *, #29333, .F. ) ;
#43122 = DIRECTION ( 'NONE',  ( -0.000000000000000000, -1.000000000000000000, -0.000000000000000000 ) ) ;
#43123 = CARTESIAN_POINT ( 'NONE',  ( 344.0000000000000000, -166.9999999999999716, 341.9999999999998295 ) ) ;
#43124 = CARTESIAN_POINT ( 'NONE',  ( 196.8526953830863135, -154.8119894309599260, 22.84256005001721945 ) ) ;
#43125 = CARTESIAN_POINT ( 'NONE',  ( -6.695973446814940111, 1.750000000000023759, 40.81828755692798438 ) ) ;
#43126 = AXIS2_PLACEMENT_3D ( 'NONE', #7791, #26771, #19315 ) ;
#43127 = VECTOR ( 'NONE', #40285, 1000.000000000000000 ) ;
#43128 = ORIENTED_EDGE ( 'NONE', *, *, #498, .T. ) ;
#43129 = EDGE_CURVE ( 'NONE', #40831, #17041, #8253, .T. ) ;
#43130 = CARTESIAN_POINT ( 'NONE',  ( -22.69295089195507487, -45.31600496604688999, 7.455576670931136185 ) ) ;
#43131 = VECTOR ( 'NONE', #13388, 1000.000000000000000 ) ;
#43132 = LINE ( 'NONE', #557, #10336 ) ;
#43133 = CARTESIAN_POINT ( 'NONE',  ( -126.6959734468149321, 0.000000000000000000, 165.0000000000000000 ) ) ;
#43134 = ORIENTED_EDGE ( 'NONE', *, *, #6765, .F. ) ;
#43135 = VERTEX_POINT ( 'NONE', #31868 ) ;
#43136 = CARTESIAN_POINT ( 'NONE',  ( 1039.120266371688786, 781.3714735868810521, 1335.804925479510075 ) ) ;
#43137 = CARTESIAN_POINT ( 'NONE',  ( 21.24469349090191983, 33.89193117067290473, 910.0000000000000000 ) ) ;
#43138 = VECTOR ( 'NONE', #27479, 1000.000000000000000 ) ;
#43139 = LINE ( 'NONE', #46693, #43858 ) ;
#43140 = ADVANCED_FACE ( 'NONE', ( #47458 ), #8770, .F. ) ;
#43141 = EDGE_CURVE ( 'NONE', #33295, #32324, #43544, .T. ) ;
#43142 = CARTESIAN_POINT ( 'NONE',  ( 193.3040265531851105, 1.750000000000010214, 40.81828755692798438 ) ) ;
#43143 = LINE ( 'NONE', #34966, #16764 ) ;
#43144 = COLOUR_RGB ( '',0.7921568627450980005, 0.8196078431372548767, 0.9333333333333333481 ) ;
#43145 = CARTESIAN_POINT ( 'NONE',  ( 2.210477865340801706, 37.43479381012853224, -9.422646554964178023 ) ) ;
#43146 = VERTEX_POINT ( 'NONE', #4891 ) ;
#43147 = EDGE_CURVE ( 'NONE', #17682, #11134, #24743, .T. ) ;
#43148 = CYLINDRICAL_SURFACE ( 'NONE', #18969, 2.000000000000001776 ) ;
#43149 = EDGE_CURVE ( 'NONE', #46777, #41284, #20554, .T. ) ;
#43150 = CARTESIAN_POINT ( 'NONE',  ( -168.4459734468149747, 1.025126265847089435, -77.43171244307200141 ) ) ;
#43151 = DIRECTION ( 'NONE',  ( 0.000000000000000000, 5.664403186863042467E-17, 1.000000000000000000 ) ) ;
#43152 =( NAMED_UNIT ( * ) SI_UNIT ( $, .STERADIAN. ) SOLID_ANGLE_UNIT ( ) );
#43153 = VECTOR ( 'NONE', #38071, 1000.000000000000000 ) ;
#43154 = EDGE_CURVE ( 'NONE', #46476, #290, #9365, .T. ) ;
#43155 = VERTEX_POINT ( 'NONE', #29260 ) ;
#43156 = DIRECTION ( 'NONE',  ( 1.000000000000000000, 0.000000000000000000, -0.000000000000000000 ) ) ;
#43157 = ORIENTED_EDGE ( 'NONE', *, *, #24604, .T. ) ;
#43158 = CARTESIAN_POINT ( 'NONE',  ( 356.0000000000000000, -165.0000000000001137, -94.00000000000019895 ) ) ;
#43159 = ORIENTED_EDGE ( 'NONE', *, *, #25759, .T. ) ;
#43160 = CARTESIAN_POINT ( 'NONE',  ( 183.0000000000000568, 165.0000000000000000, 343.9999999999998863 ) ) ;
#43161 = DIRECTION ( 'NONE',  ( 0.000000000000000000, 0.000000000000000000, -1.000000000000000000 ) ) ;
#43162 = CARTESIAN_POINT ( 'NONE',  ( -175.0000000000000000, 15.00000000000000000, -122.5000000000000000 ) ) ;
#43163 = ORIENTED_EDGE ( 'NONE', *, *, #6538, .F. ) ;
#43164 = PLANE ( 'NONE',  #49050 ) ;
#43165 = VECTOR ( 'NONE', #3213, 1000.000000000000000 ) ;
#43166 = EDGE_CURVE ( 'NONE', #46434, #18177, #37493, .T. ) ;
#43167 = CARTESIAN_POINT ( 'NONE',  ( -8.277096487746778308, 50.00000000000000000, 7.455576670931136185 ) ) ;
#43168 = ORIENTED_EDGE ( 'NONE', *, *, #10829, .T. ) ;
#43169 = CARTESIAN_POINT ( 'NONE',  ( -54.99999999999997868, -52.50000000000000711, 5.000000000000000000 ) ) ;
#43170 = FACE_OUTER_BOUND ( 'NONE', #35822, .T. ) ;
#43171 = DIRECTION ( 'NONE',  ( 0.000000000000000000, 0.000000000000000000, -1.000000000000000000 ) ) ;
#43172 = DIRECTION ( 'NONE',  ( 1.000000000000000000, 0.000000000000000000, -0.000000000000000000 ) ) ;
#43173 = ORIENTED_EDGE ( 'NONE', *, *, #35291, .F. ) ;
#43174 = ORIENTED_EDGE ( 'NONE', *, *, #39187, .F. ) ;
#43175 = CARTESIAN_POINT ( 'NONE',  ( 35.05402655318503946, 0.000000000000000000, 162.5682875569279702 ) ) ;
#43176 = ORIENTED_EDGE ( 'NONE', *, *, #1764, .F. ) ;
#43177 = CARTESIAN_POINT ( 'NONE',  ( -128.4459734468149179, 0.000000000000000000, -117.4317124430720725 ) ) ;
#43178 = CYLINDRICAL_SURFACE ( 'NONE', #47190, 4.000000000000003553 ) ;
#43179 = CARTESIAN_POINT ( 'NONE',  ( 130.0000000000012221, 16.00000000000000000, 5.000000000000004441 ) ) ;
#43180 = ORIENTED_EDGE ( 'NONE', *, *, #338, .T. ) ;
#43181 = CARTESIAN_POINT ( 'NONE',  ( -0.2099955233291965206, -1.205406147626143509, 9.993783931180535873 ) ) ;
#43182 = ORIENTED_EDGE ( 'NONE', *, *, #38426, .F. ) ;
#43183 = EDGE_CURVE ( 'NONE', #47427, #2039, #40560, .T. ) ;
#43184 = CARTESIAN_POINT ( 'NONE',  ( -1.962712821592842882, -1.022159834731130257, 9.881002359080275355 ) ) ;
#43185 = VECTOR ( 'NONE', #33725, 1000.000000000000000 ) ;
#43186 = LINE ( 'NONE', #23691, #25114 ) ;
#43187 = DIRECTION ( 'NONE',  ( 1.000000000000000000, -3.614007241618348278E-16, 0.000000000000000000 ) ) ;
#43188 = EDGE_LOOP ( 'NONE', ( #50686, #39402, #9602, #20876, #47661 ) ) ;
#43189 = ORIENTED_EDGE ( 'NONE', *, *, #37492, .F. ) ;
#43190 = EDGE_LOOP ( 'NONE', ( #33885, #43666, #12679, #7632 ) ) ;
#43191 = LINE ( 'NONE', #39607, #18128 ) ;
#43192 = B_SPLINE_CURVE_WITH_KNOTS ( 'NONE', 3,
 ( #42988, #26845, #11207, #23513 ),
 .UNSPECIFIED., .F., .F.,
 ( 4, 4 ),
 ( 1.404617285391336434E-17, 0.009404495247862658044 ),
 .UNSPECIFIED. ) ;
#43193 = DIRECTION ( 'NONE',  ( 0.000000000000000000, 0.000000000000000000, 1.000000000000000000 ) ) ;
#43194 = CARTESIAN_POINT ( 'NONE',  ( 3.222683565149129237, 0.4845875505058722110, 9.799352050262459812 ) ) ;
#43195 = EDGE_LOOP ( 'NONE', ( #35429, #6267, #21070 ) ) ;
#43196 = FACE_OUTER_BOUND ( 'NONE', #36944, .T. ) ;
#43197 = ORIENTED_EDGE ( 'NONE', *, *, #8013, .F. ) ;
#43198 = DIRECTION ( 'NONE',  ( -1.000000000000000000, 0.000000000000000000, -0.000000000000000000 ) ) ;
#43199 = ORIENTED_EDGE ( 'NONE', *, *, #49422, .T. ) ;
#43200 = FACE_OUTER_BOUND ( 'NONE', #35083, .T. ) ;
#43201 = PLANE ( 'NONE',  #5540 ) ;
#43202 = CARTESIAN_POINT ( 'NONE',  ( 210.0000000000000568, 2.143131898507881856E-16, -80.93171244307202983 ) ) ;
#43203 = ADVANCED_FACE ( 'NONE', ( #22059 ), #49470, .T. ) ;
#43204 = ADVANCED_FACE ( 'NONE', ( #9501 ), #41313, .T. ) ;
#43205 = DIRECTION ( 'NONE',  ( 0.000000000000000000, -1.000000000000000000, -3.186989995019654210E-49 ) ) ;
#43206 = VERTEX_POINT ( 'NONE', #2557 ) ;
#43207 = ORIENTED_EDGE ( 'NONE', *, *, #45651, .T. ) ;
#43208 = FACE_OUTER_BOUND ( 'NONE', #19385, .T. ) ;
#43209 = EDGE_CURVE ( 'NONE', #24506, #44363, #24238, .T. ) ;
#43210 = CARTESIAN_POINT ( 'NONE',  ( 26.42016489236587873, 32.24895757977031963, -9.387872844313825738 ) ) ;
#43211 = DIRECTION ( 'NONE',  ( 0.000000000000000000, 0.000000000000000000, 1.000000000000000000 ) ) ;
#43212 = EDGE_CURVE ( 'NONE', #38645, #49869, #29512, .T. ) ;
#43213 = ADVANCED_FACE ( 'NONE', ( #10509 ), #45128, .T. ) ;
#43214 = CARTESIAN_POINT ( 'NONE',  ( -0.3862712429686809279, -1.188820645368943163, 10.00000000000000000 ) ) ;
#43215 = CARTESIAN_POINT ( 'NONE',  ( 42.99990394833793061, 47.95759300784327905, -5.000000000000000000 ) ) ;
#43216 = ORIENTED_EDGE ( 'NONE', *, *, #30694, .F. ) ;
#43217 = LINE ( 'NONE', #892, #38527 ) ;
#43218 = EDGE_CURVE ( 'NONE', #4051, #2864, #32096, .T. ) ;
#43219 = DIRECTION ( 'NONE',  ( -1.156482317317870492E-16, 1.000000000000000000, 0.000000000000000000 ) ) ;
#43220 = ORIENTED_EDGE ( 'NONE', *, *, #27757, .F. ) ;
#43221 = CARTESIAN_POINT ( 'NONE',  ( 0.9925179869589159098, 0.000000000000000000, 0.000000000000000000 ) ) ;
#43222 = CARTESIAN_POINT ( 'NONE',  ( -128.4459734468149179, 0.000000000000000000, 42.56828755692794175 ) ) ;
#43223 = DIRECTION ( 'NONE',  ( -0.000000000000000000, -0.000000000000000000, -1.000000000000000000 ) ) ;
#43224 = ORIENTED_EDGE ( 'NONE', *, *, #23670, .T. ) ;
#43225 = ORIENTED_EDGE ( 'NONE', *, *, #23556, .F. ) ;
#43226 = CARTESIAN_POINT ( 'NONE',  ( 183.0000000000000000, -5.999999999999950262, -340.0000000000001137 ) ) ;
#43227 = DIRECTION ( 'NONE',  ( 0.000000000000000000, 1.000000000000000000, 6.123233995736766036E-17 ) ) ;
#43228 = AXIS2_PLACEMENT_3D ( 'NONE', #23957, #16259, #48016 ) ;
#43229 = ORIENTED_EDGE ( 'NONE', *, *, #24434, .T. ) ;
#43230 = ORIENTED_EDGE ( 'NONE', *, *, #14345, .T. ) ;
#43231 = DIRECTION ( 'NONE',  ( -1.000000000000000000, 0.000000000000000000, 1.860490536778032451E-50 ) ) ;
#43232 = CARTESIAN_POINT ( 'NONE',  ( 26.18032376592674737, -21.95228666728361233, 7.455576670931136185 ) ) ;
#43233 = CARTESIAN_POINT ( 'NONE',  ( 356.0000000000000568, 175.0000000000000284, -94.00000000000019895 ) ) ;
#43234 = ORIENTED_EDGE ( 'NONE', *, *, #14058, .T. ) ;
#43235 = ORIENTED_EDGE ( 'NONE', *, *, #31789, .T. ) ;
#43236 = ORIENTED_EDGE ( 'NONE', *, *, #6051, .F. ) ;
#43237 = EDGE_CURVE ( 'NONE', #41284, #47386, #34734, .T. ) ;
#43238 = LINE ( 'NONE', #20145, #27544 ) ;
#43239 =( BOUNDED_CURVE ( )  B_SPLINE_CURVE ( 3, ( #13073, #36455, #47677, #47937 ),
 .UNSPECIFIED., .F., .F. ) 
 B_SPLINE_CURVE_WITH_KNOTS ( ( 4, 4 ),
 ( 0.000000000000000000, 1.570796326794896558 ),
 .UNSPECIFIED. ) 
 CURVE ( )  GEOMETRIC_REPRESENTATION_ITEM ( )  RATIONAL_B_SPLINE_CURVE ( ( 1.000000000000000000, 0.8047378541243649375, 0.8047378541243649375, 1.000000000000000000 ) ) 
 REPRESENTATION_ITEM ( '' )  );
#43240 = ORIENTED_EDGE ( 'NONE', *, *, #39361, .T. ) ;
#43241 = CARTESIAN_POINT ( 'NONE',  ( 6.875132362119187768, -33.14667368551891258, 8.356839323120299312 ) ) ;
#43242 = LINE ( 'NONE', #8108, #24158 ) ;
#43243 = CARTESIAN_POINT ( 'NONE',  ( 111.5540265531850537, 1.025126265847081664, -117.4317124430720440 ) ) ;
#43244 = ORIENTED_EDGE ( 'NONE', *, *, #34310, .F. ) ;
#43245 = ORIENTED_EDGE ( 'NONE', *, *, #29806, .F. ) ;
#43246 = DIRECTION ( 'NONE',  ( -0.000000000000000000, -0.000000000000000000, -1.000000000000000000 ) ) ;
#43247 =( BOUNDED_CURVE ( )  B_SPLINE_CURVE ( 3, ( #13647, #48502, #23757, #13143 ),
 .UNSPECIFIED., .F., .F. ) 
 B_SPLINE_CURVE_WITH_KNOTS ( ( 4, 4 ),
 ( 3.141592653589793116, 4.712388980384689674 ),
 .UNSPECIFIED. ) 
 CURVE ( )  GEOMETRIC_REPRESENTATION_ITEM ( )  RATIONAL_B_SPLINE_CURVE ( ( 1.000000000000000000, 0.8047378541243649375, 0.8047378541243649375, 1.000000000000000000 ) ) 
 REPRESENTATION_ITEM ( '' )  );
#43248 = CARTESIAN_POINT ( 'NONE',  ( 344.0000000000000000, 175.0000000000000284, -92.00000000000019895 ) ) ;
#43249 = ORIENTED_EDGE ( 'NONE', *, *, #14051, .T. ) ;
#43250 = ORIENTED_EDGE ( 'NONE', *, *, #46773, .T. ) ;
#43251 = DIRECTION ( 'NONE',  ( -0.000000000000000000, -0.000000000000000000, -1.000000000000000000 ) ) ;
#43252 = CARTESIAN_POINT ( 'NONE',  ( -46.76852358249002606, 17.86468378716741512, -9.367992836599951190 ) ) ;
#43253 = ORIENTED_EDGE ( 'NONE', *, *, #28511, .F. ) ;
#43254 = LINE ( 'NONE', #3753, #23069 ) ;
#43255 = DIRECTION ( 'NONE',  ( -0.000000000000000000, -0.000000000000000000, 1.000000000000000000 ) ) ;
#43256 = CARTESIAN_POINT ( 'NONE',  ( -164.9459734468149463, 2.143131898507880377E-16, -160.9317124430720014 ) ) ;
#43257 = ADVANCED_FACE ( 'NONE', ( #48709 ), #25165, .F. ) ;
#43258 = FACE_OUTER_BOUND ( 'NONE', #5380, .T. ) ;
#43259 = ORIENTED_EDGE ( 'NONE', *, *, #10685, .T. ) ;
#43260 = CARTESIAN_POINT ( 'NONE',  ( 1.011271242968694084, -0.7347315653655782652, 10.00000000000000000 ) ) ;
#43261 = CARTESIAN_POINT ( 'NONE',  ( 331.7552636306688214, -248.6897383013408103, 297.1446280767819985 ) ) ;
#43262 =( BOUNDED_CURVE ( )  B_SPLINE_CURVE ( 3, ( #41925, #22176, #22421, #25516 ),
 .UNSPECIFIED., .F., .F. ) 
 B_SPLINE_CURVE_WITH_KNOTS ( ( 4, 4 ),
 ( 0.000000000000000000, 1.570796326794896780 ),
 .UNSPECIFIED. ) 
 CURVE ( )  GEOMETRIC_REPRESENTATION_ITEM ( )  RATIONAL_B_SPLINE_CURVE ( ( 1.000000000000000000, 0.8047378541243649375, 0.8047378541243649375, 1.000000000000000000 ) ) 
 REPRESENTATION_ITEM ( '' )  );
#43263 = DIRECTION ( 'NONE',  ( -1.000000000000000000, 0.000000000000000000, -2.958228394578794270E-31 ) ) ;
#43264 = EDGE_CURVE ( 'NONE', #37192, #31020, #48461, .T. ) ;
#43265 = CARTESIAN_POINT ( 'NONE',  ( -8.445973446814976526, 0.000000000000000000, 2.568287556928034121 ) ) ;
#43266 = ADVANCED_FACE ( 'NONE', ( #5652 ), #13348, .T. ) ;
#43267 = VECTOR ( 'NONE', #41872, 1000.000000000000000 ) ;
#43268 = EDGE_CURVE ( 'NONE', #21250, #50360, #20627, .T. ) ;
#43269 = PLANE ( 'NONE',  #44990 ) ;
#43270 = CARTESIAN_POINT ( 'NONE',  ( -50.11058929355266400, 7.578863168071933387, 7.455576670931136185 ) ) ;
#43271 = B_SPLINE_CURVE_WITH_KNOTS ( 'NONE', 3,
 ( #14476, #26286, #37360, #25521 ),
 .UNSPECIFIED., .F., .F.,
 ( 4, 4 ),
 ( 0.000000000000000000, 0.009404495247862337121 ),
 .UNSPECIFIED. ) ;
#43272 = CYLINDRICAL_SURFACE ( 'NONE', #2540, 0.4999999999999997224 ) ;
#43273 = ORIENTED_EDGE ( 'NONE', *, *, #5454, .T. ) ;
#43274 = PLANE ( 'NONE',  #36070 ) ;
#43275 = VERTEX_POINT ( 'NONE', #21554 ) ;
#43276 = DIRECTION ( 'NONE',  ( 1.000000000000000000, 1.156482317317870492E-16, -0.000000000000000000 ) ) ;
#43277 = DIRECTION ( 'NONE',  ( 0.000000000000000000, -1.000000000000000000, 2.969158215481698263E-48 ) ) ;
#43278 = CARTESIAN_POINT ( 'NONE',  ( 31.55402655318503236, 0.000000000000000000, 2.568287556927978166 ) ) ;
#43279 = ORIENTED_EDGE ( 'NONE', *, *, #47915, .F. ) ;
#43280 = DIRECTION ( 'NONE',  ( 0.000000000000000000, 0.000000000000000000, 1.000000000000000000 ) ) ;
#43281 = B_SPLINE_SURFACE_WITH_KNOTS ( 'NONE', 3, 3, ( 
 ( #15025, #50374, #26829, #22963 ),
 ( #3457, #15291, #30950, #46536 ),
 ( #27079, #24761, #25009, #8848 ),
 ( #13194, #12689, #28350, #27849 ) ),
 .UNSPECIFIED., .F., .F., .F.,
 ( 4, 4 ),
 ( 4, 4 ),
 ( 0.000000000000000000, 1.000000000000000000 ),
 ( 0.000000000000000000, 1.000000000000000000 ),
 .UNSPECIFIED. ) ;
#43282 = EDGE_LOOP ( 'NONE', ( #26430, #411, #15707, #43480, #13752, #10117 ) ) ;
#43283 = ORIENTED_EDGE ( 'NONE', *, *, #13028, .T. ) ;
#43284 = CARTESIAN_POINT ( 'NONE',  ( 0.3862712429686978033, -1.188820645368937834, 3.333333333333333481 ) ) ;
#43285 = CARTESIAN_POINT ( 'NONE',  ( 167.5000000000000000, -102.5000000000000142, 10.00000000000000000 ) ) ;
#43286 = VERTEX_POINT ( 'NONE', #30274 ) ;
#43287 = CARTESIAN_POINT ( 'NONE',  ( 350.0000000000000000, -180.9999999999999716, -356.0000000000002274 ) ) ;
#43288 = CARTESIAN_POINT ( 'NONE',  ( 167.0000000000000000, -9.999999999999953815, -99.00000000000014211 ) ) ;
#43289 = LINE ( 'NONE', #15352, #4664 ) ;
#43290 = ORIENTED_EDGE ( 'NONE', *, *, #1396, .F. ) ;
#43291 = ADVANCED_FACE ( 'NONE', ( #42319 ), #1957, .T. ) ;
#43292 = CARTESIAN_POINT ( 'NONE',  ( -5.000000000000000000, -165.1999999999999602, 359.7999999999997840 ) ) ;
#43293 = DIRECTION ( 'NONE',  ( -1.000000000000000000, -0.000000000000000000, -0.000000000000000000 ) ) ;
#43294 = DIRECTION ( 'NONE',  ( -3.172065784643302499E-16, -1.000000000000000000, 2.537652627714642000E-15 ) ) ;
#43295 = ORIENTED_EDGE ( 'NONE', *, *, #44396, .F. ) ;
#43296 = VECTOR ( 'NONE', #2926, 1000.000000000000000 ) ;
#43297 = CYLINDRICAL_SURFACE ( 'NONE', #44784, 1.750000000000001554 ) ;
#43298 = CARTESIAN_POINT ( 'NONE',  ( -6.695973446814940111, 0.000000000000000000, 165.0000000000000000 ) ) ;
#43299 = ORIENTED_EDGE ( 'NONE', *, *, #8698, .F. ) ;
#43300 = ORIENTED_EDGE ( 'NONE', *, *, #48868, .F. ) ;
#43301 = ORIENTED_EDGE ( 'NONE', *, *, #43769, .F. ) ;
#43302 = LINE ( 'NONE', #31021, #22141 ) ;
#43303 = CARTESIAN_POINT ( 'NONE',  ( 34.99999999999997868, 16.00000000000000000, -114.9999999999999858 ) ) ;
#43304 = ORIENTED_EDGE ( 'NONE', *, *, #43154, .F. ) ;
#43305 = CLOSED_SHELL ( 'NONE', ( #15803, #21453, #31243, #50594, #29771, #42265, #50541, #49033, #2763, #29134, #30855, #5154, #16602, #12640, #12973, #26172, #36735, #16754 ) ) ;
#43306 = CARTESIAN_POINT ( 'NONE',  ( 3.627208138665139803, 0.000000000000000000, 27.58190990837850265 ) ) ;
#43307 = CARTESIAN_POINT ( 'NONE',  ( -46.69597344681494633, -1.750000000000009992, 0.8182875569279768335 ) ) ;
#43308 = CARTESIAN_POINT ( 'NONE',  ( 30.00000000000092726, 16.00000000000000000, 0.000000000000000000 ) ) ;
#43309 = DIRECTION ( 'NONE',  ( -0.000000000000000000, -0.000000000000000000, -1.000000000000000000 ) ) ;
#43310 = FACE_OUTER_BOUND ( 'NONE', #49856, .T. ) ;
#43311 = CARTESIAN_POINT ( 'NONE',  ( -1.250000000000000222, 0.000000000000000000, 10.00000000000000000 ) ) ;
#43312 = CARTESIAN_POINT ( 'NONE',  ( -206.6959734468149463, 1.750000000000010214, 40.81828755692798438 ) ) ;
#43313 = DIRECTION ( 'NONE',  ( 0.000000000000000000, 0.000000000000000000, 1.000000000000000000 ) ) ;
#43314 = DIRECTION ( 'NONE',  ( 0.000000000000000000, 1.000000000000000000, 0.000000000000000000 ) ) ;
#43315 = CARTESIAN_POINT ( 'NONE',  ( 3.231548175622897645, -9.463461120997347820, 9.282506307616472441 ) ) ;
#43316 = CARTESIAN_POINT ( 'NONE',  ( -2.774199681320129951, -2.805557802885433993, 6.494306115488113207 ) ) ;
#43317 = DIRECTION ( 'NONE',  ( -1.000000000000000000, 0.000000000000000000, 0.000000000000000000 ) ) ;
#43318 = CARTESIAN_POINT ( 'NONE',  ( 50.24128791297869867, -41.04536285977715693, -5.000000000000000000 ) ) ;
#43319 = CARTESIAN_POINT ( 'NONE',  ( -69.99999999999879208, 17.00000000000000000, 5.000000000000004441 ) ) ;
#43320 = CARTESIAN_POINT ( 'NONE',  ( 151.5540265531850537, 1.025126265847089657, 119.0682875569279560 ) ) ;
#43321 = EDGE_LOOP ( 'NONE', ( #4177, #63, #49417, #40660, #43606, #44887 ) ) ;
#43322 = EDGE_CURVE ( 'NONE', #38973, #2035, #6657, .T. ) ;
#43323 = CARTESIAN_POINT ( 'NONE',  ( 47.55282581475783132, -15.45084971874691604, 0.000000000000000000 ) ) ;
#43324 = CARTESIAN_POINT ( 'NONE',  ( -164.9999999999990905, 17.00000000000000000, 0.000000000000000000 ) ) ;
#43325 = CARTESIAN_POINT ( 'NONE',  ( 0.000000000000000000, 167.0000000000000000, -356.0000000000002274 ) ) ;
#43326 = CARTESIAN_POINT ( 'NONE',  ( 151.5540265531850537, 0.000000000000000000, 162.5682875569279702 ) ) ;
#43327 = AXIS2_PLACEMENT_3D ( 'NONE', #49392, #10688, #34059 ) ;
#43328 = ORIENTED_EDGE ( 'NONE', *, *, #40945, .F. ) ;
#43329 = CARTESIAN_POINT ( 'NONE',  ( -210.0000000000000568, 0.000000000000000000, 0.8182875569279768335 ) ) ;
#43330 = ORIENTED_EDGE ( 'NONE', *, *, #295, .F. ) ;
#43331 = LINE ( 'NONE', #27448, #15542 ) ;
#43332 =( BOUNDED_CURVE ( )  B_SPLINE_CURVE ( 3, ( #1860, #13390, #44669, #2351 ),
 .UNSPECIFIED., .F., .F. ) 
 B_SPLINE_CURVE_WITH_KNOTS ( ( 4, 4 ),
 ( 3.141592653589793116, 4.712388980384689674 ),
 .UNSPECIFIED. ) 
 CURVE ( )  GEOMETRIC_REPRESENTATION_ITEM ( )  RATIONAL_B_SPLINE_CURVE ( ( 1.000000000000000000, 0.8047378541243649375, 0.8047378541243649375, 1.000000000000000000 ) ) 
 REPRESENTATION_ITEM ( '' )  );
#43333 = CIRCLE ( 'NONE', #21220, 1.750000000000001554 ) ;
#43334 = EDGE_LOOP ( 'NONE', ( #44230, #35456, #11896, #13356, #39015, #32269, #25620, #45424, #3522, #11233, #29664, #50713, #49878, #1233 ) ) ;
#43335 = VECTOR ( 'NONE', #42782, 1000.000000000000000 ) ;
#43336 = CARTESIAN_POINT ( 'NONE',  ( 155.0540265531850537, -1.025126265847089213, -160.9317124430720014 ) ) ;
#43337 = CARTESIAN_POINT ( 'NONE',  ( -1.275927284277175167, 0.1224368140627496299, 9.976582533991679824 ) ) ;
#43338 = ORIENTED_EDGE ( 'NONE', *, *, #44797, .F. ) ;
#43339 = VECTOR ( 'NONE', #795, 1000.000000000000000 ) ;
#43340 = ORIENTED_EDGE ( 'NONE', *, *, #4381, .T. ) ;
#43341 = VECTOR ( 'NONE', #31712, 1000.000000000000000 ) ;
#43342 = VERTEX_POINT ( 'NONE', #50480 ) ;
#43343 = CARTESIAN_POINT ( 'NONE',  ( -165.0000000000000284, 16.00000000000000000, 115.0000000000000142 ) ) ;
#43344 = CARTESIAN_POINT ( 'NONE',  ( 181.0000000000000000, -164.9999999999999432, -344.0000000000001137 ) ) ;
#43345 =( REPRESENTATION_RELATIONSHIP ('NONE','NONE', #45699, #31369 ) REPRESENTATION_RELATIONSHIP_WITH_TRANSFORMATION ( #9742 )SHAPE_REPRESENTATION_RELATIONSHIP( ) );
#43346 = ORIENTED_EDGE ( 'NONE', *, *, #19160, .T. ) ;
#43347 = CARTESIAN_POINT ( 'NONE',  ( 210.0000000000000568, 0.000000000000000000, -119.1817124430720440 ) ) ;
#43348 = DIRECTION ( 'NONE',  ( -0.000000000000000000, -0.000000000000000000, -1.000000000000000000 ) ) ;
#43349 = CARTESIAN_POINT ( 'NONE',  ( 210.0000000000000568, 2.143131898507881856E-16, 79.06828755692797017 ) ) ;
#43350 = EDGE_CURVE ( 'NONE', #13694, #26320, #21632, .T. ) ;
#43351 = DIRECTION ( 'NONE',  ( -1.586032880504786307E-16, 1.654361225106055350E-24, -1.000000000000000000 ) ) ;
#43352 = FACE_OUTER_BOUND ( 'NONE', #30900, .T. ) ;
#43353 = EDGE_CURVE ( 'NONE', #11178, #9223, #11019, .T. ) ;
#43354 = VERTEX_POINT ( 'NONE', #34900 ) ;
#43355 = DIRECTION ( 'NONE',  ( -1.000000000000000000, -0.000000000000000000, -0.000000000000000000 ) ) ;
#43356 = LINE ( 'NONE', #43610, #15509 ) ;
#43357 = VERTEX_POINT ( 'NONE', #31041 ) ;
#43358 = PLANE ( 'NONE',  #8700 ) ;
#43359 = CARTESIAN_POINT ( 'NONE',  ( 185.0000000000000000, -164.9999999999999432, -356.0000000000001705 ) ) ;
#43360 = ORIENTED_EDGE ( 'NONE', *, *, #1265, .F. ) ;
#43361 = CARTESIAN_POINT ( 'NONE',  ( 210.0000000000000568, 0.000000000000000000, -117.4317124430720298 ) ) ;
#43362 = VECTOR ( 'NONE', #31628, 1000.000000000000000 ) ;
#43363 = LINE ( 'NONE', #4383, #12630 ) ;
#43364 = CARTESIAN_POINT ( 'NONE',  ( -114.9999999999981526, 17.00000000000000000, 90.00000000000000000 ) ) ;
#43365 = CARTESIAN_POINT ( 'NONE',  ( 339.9999999999999432, -180.9999999999999716, -356.0000000000002274 ) ) ;
#43366 = CIRCLE ( 'NONE', #8993, 2.000000000000001776 ) ;
#43367 = ORIENTED_EDGE ( 'NONE', *, *, #4502, .F. ) ;
#43368 = CYLINDRICAL_SURFACE ( 'NONE', #21226, 4.000000000000003553 ) ;
#43369 = VECTOR ( 'NONE', #13762, 1000.000000000000000 ) ;
#43370 = CARTESIAN_POINT ( 'NONE',  ( 14.52758583651987223, 8.922352469211173087, 8.953103998512858652 ) ) ;
#43371 = VECTOR ( 'NONE', #36419, 1000.000000000000114 ) ;
#43372 = CARTESIAN_POINT ( 'NONE',  ( 28.96803024440893992, 18.11533787072037072, 7.455576670931136185 ) ) ;
#43373 = ORIENTED_EDGE ( 'NONE', *, *, #35781, .F. ) ;
#43374 = ORIENTED_EDGE ( 'NONE', *, *, #21239, .T. ) ;
#43375 = DIRECTION ( 'NONE',  ( 1.608507482352848411E-14, -0.1191452206184307749, 0.9928768384869220975 ) ) ;
#43376 = CARTESIAN_POINT ( 'NONE',  ( 169.0000000000000000, 2.775557561562891351E-14, -113.0000000000001563 ) ) ;
#43377 = EDGE_CURVE ( 'NONE', #20584, #29162, #42062, .T. ) ;
#43378 = EDGE_CURVE ( 'NONE', #35747, #45670, #2587, .T. ) ;
#43379 = CARTESIAN_POINT ( 'NONE',  ( 2.538055338523173443, 45.80735277814159190, -9.367992836599951190 ) ) ;
#43380 = VERTEX_POINT ( 'NONE', #46635 ) ;
#43381 = LINE ( 'NONE', #20796, #16536 ) ;
#43382 = EDGE_CURVE ( 'NONE', #35493, #7132, #34639, .T. ) ;
#43383 = PRODUCT ( 'frame_Default<As Machined>', 'frame_Default<As Machined>', '', ( #1809 ) ) ;
#43384 = PLANE ( 'NONE',  #11402 ) ;
#43385 = DIRECTION ( 'NONE',  ( -0.000000000000000000, 3.186989995019654210E-49, 1.000000000000000000 ) ) ;
#43386 = ADVANCED_FACE ( 'NONE', ( #11282 ), #27186, .F. ) ;
#43387 = FACE_OUTER_BOUND ( 'NONE', #35420, .T. ) ;
#43388 = EDGE_CURVE ( 'NONE', #15960, #36214, #25871, .T. ) ;
#43389 =( BOUNDED_CURVE ( )  B_SPLINE_CURVE ( 3, ( #21867, #2350, #47812, #33664 ),
 .UNSPECIFIED., .F., .F. ) 
 B_SPLINE_CURVE_WITH_KNOTS ( ( 4, 4 ),
 ( 4.712388980384689674, 6.283185307179586232 ),
 .UNSPECIFIED. ) 
 CURVE ( )  GEOMETRIC_REPRESENTATION_ITEM ( )  RATIONAL_B_SPLINE_CURVE ( ( 1.000000000000000000, 0.8047378541243649375, 0.8047378541243649375, 1.000000000000000000 ) ) 
 REPRESENTATION_ITEM ( '' )  );
#43390 = ORIENTED_EDGE ( 'NONE', *, *, #49692, .F. ) ;
#43391 = FACE_BOUND ( 'NONE', #31612, .T. ) ;
#43392 = ORIENTED_EDGE ( 'NONE', *, *, #9536, .F. ) ;
#43393 = PLANE ( 'NONE',  #31077 ) ;
#43394 = ORIENTED_EDGE ( 'NONE', *, *, #16222, .T. ) ;
#43395 = LINE ( 'NONE', #4162, #34453 ) ;
#43396 = PLANE ( 'NONE',  #10183 ) ;
#43397 =( BOUNDED_CURVE ( )  B_SPLINE_CURVE ( 3, ( #16698, #43150, #39566, #31622 ),
 .UNSPECIFIED., .F., .F. ) 
 B_SPLINE_CURVE_WITH_KNOTS ( ( 4, 4 ),
 ( 3.141592653589793116, 4.712388980384689674 ),
 .UNSPECIFIED. ) 
 CURVE ( )  GEOMETRIC_REPRESENTATION_ITEM ( )  RATIONAL_B_SPLINE_CURVE ( ( 1.000000000000000000, 0.8047378541243649375, 0.8047378541243649375, 1.000000000000000000 ) ) 
 REPRESENTATION_ITEM ( '' )  );
#43398 = CARTESIAN_POINT ( 'NONE',  ( 74.32915281903215998, -1.750000000000009548, 41.84341382277508359 ) ) ;
#43399 = LINE ( 'NONE', #28014, #12426 ) ;
#43400 = AXIS2_PLACEMENT_3D ( 'NONE', #17668, #37201, #14061 ) ;
#43401 = ORIENTED_EDGE ( 'NONE', *, *, #47562, .F. ) ;
#43402 = AXIS2_PLACEMENT_3D ( 'NONE', #7635, #35363, #23263 ) ;
#43403 = CIRCLE ( 'NONE', #13909, 1.750000000000008438 ) ;
#43404 = CARTESIAN_POINT ( 'NONE',  ( 210.0000000000000568, 0.000000000000000000, -77.43171244307200141 ) ) ;
#43405 = CARTESIAN_POINT ( 'NONE',  ( 210.0000000000000568, 0.000000000000000000, -119.1817124430720440 ) ) ;
#43406 = ORIENTED_EDGE ( 'NONE', *, *, #19101, .T. ) ;
#43407 = DIRECTION ( 'NONE',  ( 1.000000000000000000, 0.000000000000000000, 0.000000000000000000 ) ) ;
#43408 = DIRECTION ( 'NONE',  ( -1.000000000000000000, -0.000000000000000000, -0.000000000000000000 ) ) ;
#43409 = CARTESIAN_POINT ( 'NONE',  ( 193.3040265531851105, 0.000000000000000000, 165.0000000000000000 ) ) ;
#43410 = AXIS2_PLACEMENT_3D ( 'NONE', #43929, #5686, #17495 ) ;
#43411 = ORIENTED_EDGE ( 'NONE', *, *, #45252, .T. ) ;
#43413 = ORIENTED_EDGE ( 'NONE', *, *, #11158, .T. ) ;
#43412 = EDGE_CURVE ( 'NONE', #12301, #4003, #25534, .T. ) ;
#43414 = LINE ( 'NONE', #11360, #20180 ) ;
#43415 = ADVANCED_FACE ( 'NONE', ( #25577 ), #37151, .T. ) ;
#43416 = VECTOR ( 'NONE', #42390, 1000.000000000000000 ) ;
#43417 = EDGE_CURVE ( 'NONE', #21466, #29055, #41396, .T. ) ;
#43418 = ADVANCED_FACE ( 'NONE', ( #33535 ), #41217, .F. ) ;
#43419 = ORIENTED_EDGE ( 'NONE', *, *, #5559, .F. ) ;
#43420 = CARTESIAN_POINT ( 'NONE',  ( -214.5896300087917155, 164.9999999999999716, 498.0000000000002274 ) ) ;
#43421 = PLANE ( 'NONE',  #21006 ) ;
#43422 = DIRECTION ( 'NONE',  ( 1.000000000000000000, 0.000000000000000000, 0.000000000000000000 ) ) ;
#43423 = VERTEX_POINT ( 'NONE', #13761 ) ;
#43424 = DIRECTION ( 'NONE',  ( -0.000000000000000000, -0.000000000000000000, -1.000000000000000000 ) ) ;
#43425 = ADVANCED_FACE ( 'NONE', ( #29182 ), #41980, .T. ) ;
#43426 = ORIENTED_EDGE ( 'NONE', *, *, #6473, .T. ) ;
#43427 = ADVANCED_FACE ( 'NONE', ( #41727 ), #37905, .F. ) ;
#43428 = EDGE_LOOP ( 'NONE', ( #15978, #28880, #48595, #34521, #48835, #46298 ) ) ;
#43429 = DIRECTION ( 'NONE',  ( 0.000000000000000000, -1.000000000000000000, 0.000000000000000000 ) ) ;
#43430 = CARTESIAN_POINT ( 'NONE',  ( -8.277096487746778308, 50.00000000000000711, 7.455576670931136185 ) ) ;
#43431 = ORIENTED_EDGE ( 'NONE', *, *, #37481, .T. ) ;
#43432 = VERTEX_POINT ( 'NONE', #41475 ) ;
#43433 = VERTEX_POINT ( 'NONE', #1973 ) ;
#43434 = CARTESIAN_POINT ( 'NONE',  ( 42.51732812238058301, -47.49695244670218131, 5.000000000000000000 ) ) ;
#43435 = CARTESIAN_POINT ( 'NONE',  ( -6.695973446814940111, -1.750000000000024203, 120.8182875569279702 ) ) ;
#43436 = CARTESIAN_POINT ( 'NONE',  ( -15.00000000000000000, -46.40197772635230677, -5.828307196921269195 ) ) ;
#43437 = VERTEX_POINT ( 'NONE', #49630 ) ;
#43438 = CARTESIAN_POINT ( 'NONE',  ( 357.1715728752537871, 167.0000000000001990, -342.0000000000002842 ) ) ;
#43440 = ORIENTED_EDGE ( 'NONE', *, *, #3053, .T. ) ;
#43439 = CIRCLE ( 'NONE', #47515, 3.749999999999975575 ) ;
#43441 = EDGE_CURVE ( 'NONE', #46863, #18038, #18155, .T. ) ;
#43442 = LINE ( 'NONE', #18002, #28323 ) ;
#43444 = ORIENTED_EDGE ( 'NONE', *, *, #5253, .T. ) ;
#43443 = VECTOR ( 'NONE', #1647, 1000.000000000000000 ) ;
#43445 = CARTESIAN_POINT ( 'NONE',  ( 168.9999999999999716, -272.4999999999999432, -339.9999999999998863 ) ) ;
#43446 = FACE_OUTER_BOUND ( 'NONE', #19554, .T. ) ;
#43447 = FACE_OUTER_BOUND ( 'NONE', #9087, .T. ) ;
#43448 = CARTESIAN_POINT ( 'NONE',  ( 34.32915281903212446, -1.750000000000009548, 161.8434138227750907 ) ) ;
#43449 = AXIS2_PLACEMENT_3D ( 'NONE', #10348, #19800, #47470 ) ;
#43450 = EDGE_CURVE ( 'NONE', #14373, #17870, #2720, .T. ) ;
#43451 = EDGE_CURVE ( 'NONE', #950, #24182, #29422, .T. ) ;
#43452 = CARTESIAN_POINT ( 'NONE',  ( 4.672045878990125800, -50.00000000000000711, 1.847720168420772691 ) ) ;
#43453 = CARTESIAN_POINT ( 'NONE',  ( 26.18032376592674737, -21.95228666728361233, 7.455576670931136185 ) ) ;
#43454 = ORIENTED_EDGE ( 'NONE', *, *, #7400, .F. ) ;
#43455 = ORIENTED_EDGE ( 'NONE', *, *, #39634, .F. ) ;
#43457 = VECTOR ( 'NONE', #50189, 1000.000000000000000 ) ;
#43456 = DIRECTION ( 'NONE',  ( 0.000000000000000000, 0.000000000000000000, 1.000000000000000000 ) ) ;
#43458 =( GEOMETRIC_REPRESENTATION_CONTEXT ( 3 ) GLOBAL_UNCERTAINTY_ASSIGNED_CONTEXT ( ( #6056 ) ) GLOBAL_UNIT_ASSIGNED_CONTEXT ( ( #3542, #19455, #15107 ) ) REPRESENTATION_CONTEXT ( 'NONE', 'WORKASPACE' ) );
#43459 = FACE_OUTER_BOUND ( 'NONE', #6743, .T. ) ;
#43460 = CARTESIAN_POINT ( 'NONE',  ( -48.98697415750977768, -11.03699497439218646, -8.016098858316199838 ) ) ;
#43461 = PLANE ( 'NONE',  #2630 ) ;
#43462 = FACE_OUTER_BOUND ( 'NONE', #18400, .T. ) ;
#43463 = ORIENTED_EDGE ( 'NONE', *, *, #15300, .T. ) ;
#43464 = EDGE_CURVE ( 'NONE', #6873, #10796, #129, .T. ) ;
#43465 = CARTESIAN_POINT ( 'NONE',  ( -41.59994237955809382, 5.070535260985659320, 7.544061037322998153 ) ) ;
#43466 = DIRECTION ( 'NONE',  ( -1.000000000000000000, 0.000000000000000000, 0.000000000000000000 ) ) ;
#43467 = ORIENTED_EDGE ( 'NONE', *, *, #27154, .F. ) ;
#43468 = CARTESIAN_POINT ( 'NONE',  ( 1.249999999999999778, -0.000000000000000000, -10.00000000000000000 ) ) ;
#43469 = EDGE_CURVE ( 'NONE', #5743, #6144, #18356, .T. ) ;
#43470 = CARTESIAN_POINT ( 'NONE',  ( 339.9999999999999432, 181.0000000000000284, -360.0000000000002274 ) ) ;
#43471 = CARTESIAN_POINT ( 'NONE',  ( 349.9999999999999432, -182.9999999999999716, 355.9999999999997726 ) ) ;
#43472 = ORIENTED_EDGE ( 'NONE', *, *, #10456, .T. ) ;
#43473 = ORIENTED_EDGE ( 'NONE', *, *, #16861, .F. ) ;
#43474 = LINE ( 'NONE', #4481, #20956 ) ;
#43475 = CARTESIAN_POINT ( 'NONE',  ( -0.3370904143228978245, 0.2449105217885259589, 10.00000000000000000 ) ) ;
#43476 = AXIS2_PLACEMENT_3D ( 'NONE', #13498, #25308, #41963 ) ;
#43477 = ADVANCED_FACE ( 'NONE', ( #14266 ), #17619, .T. ) ;
#43478 = AXIS2_PLACEMENT_3D ( 'NONE', #35488, #35753, #19549 ) ;
#43479 = EDGE_CURVE ( 'NONE', #13504, #37058, #45548, .T. ) ;
#43480 = ORIENTED_EDGE ( 'NONE', *, *, #23078, .T. ) ;
#43481 = ORIENTED_EDGE ( 'NONE', *, *, #20236, .T. ) ;
#43482 = DIRECTION ( 'NONE',  ( -1.586032892321652236E-16, -1.000000000000000000, -6.853681917100419162E-49 ) ) ;
#43483 = CARTESIAN_POINT ( 'NONE',  ( -6.875132362119187768, 33.14667368551891258, 8.356839323120299312 ) ) ;
#43484 = DIRECTION ( 'NONE',  ( 1.333906992743555050E-23, -1.000000000000000000, 0.000000000000000000 ) ) ;
#43485 = CYLINDRICAL_SURFACE ( 'NONE', #28050, 1.749999999999973799 ) ;
#43486 = VERTEX_POINT ( 'NONE', #45045 ) ;
#43487 = ORIENTED_EDGE ( 'NONE', *, *, #29891, .T. ) ;
#43488 = ORIENTED_EDGE ( 'NONE', *, *, #40671, .T. ) ;
#43489 = ADVANCED_FACE ( 'NONE', ( #18363 ), #34045, .T. ) ;
#43490 = VECTOR ( 'NONE', #32818, 1000.000000000000000 ) ;
#43491 = EDGE_CURVE ( 'NONE', #30540, #750, #13511, .T. ) ;
#43492 = DIRECTION ( 'NONE',  ( 0.000000000000000000, 0.000000000000000000, -1.000000000000000000 ) ) ;
#43493 = EDGE_CURVE ( 'NONE', #1405, #17026, #3154, .T. ) ;
#43494 = ORIENTED_EDGE ( 'NONE', *, *, #37948, .T. ) ;
#43495 = ORIENTED_EDGE ( 'NONE', *, *, #15770, .T. ) ;
#43496 = VERTEX_POINT ( 'NONE', #19325 ) ;
#43497 = CARTESIAN_POINT ( 'NONE',  ( 1.962558162476984114, -3.366505435497487042, 9.741991644047251597 ) ) ;
#43498 = CARTESIAN_POINT ( 'NONE',  ( 1.011271242968688311, -0.7347315653655855927, -3.333333333333333481 ) ) ;
#43499 = ADVANCED_FACE ( 'NONE', ( #30121 ), #46194, .T. ) ;
#43500 = CYLINDRICAL_SURFACE ( 'NONE', #42088, 1.750000000000015543 ) ;
#43501 = VERTEX_POINT ( 'NONE', #3673 ) ;
#43502 = ORIENTED_EDGE ( 'NONE', *, *, #24252, .T. ) ;
#43503 = CARTESIAN_POINT ( 'NONE',  ( 1.377509002708426689, -0.6027468487254984408, 9.927319414211227766 ) ) ;
#43504 = CARTESIAN_POINT ( 'NONE',  ( 33.30402655318503946, 1.750000000000009992, -159.1817124430720298 ) ) ;
#43505 = ORIENTED_EDGE ( 'NONE', *, *, #25812, .F. ) ;
#43506 = CARTESIAN_POINT ( 'NONE',  ( -86.69597344681494633, -1.750000000000010658, 120.8182875569279702 ) ) ;
#43507 = CARTESIAN_POINT ( 'NONE',  ( 0.000000000000000000, 0.000000000000000000, 900.0000000000000000 ) ) ;
#43508 = CARTESIAN_POINT ( 'NONE',  ( 30.00000000000219202, 16.00000000000000000, 115.0000000000000142 ) ) ;
#43509 = CARTESIAN_POINT ( 'NONE',  ( 152.2789002873379900, -1.750000000000009548, -40.20683870891912193 ) ) ;
#43510 = ORIENTED_EDGE ( 'NONE', *, *, #43836, .F. ) ;
#43511 = CARTESIAN_POINT ( 'NONE',  ( -4.945973446814903696, 2.143131898507913410E-16, 165.0000000000000000 ) ) ;
#43512 = CARTESIAN_POINT ( 'NONE',  ( 191.5540265531850537, 1.025126265847089657, -120.9317124430720440 ) ) ;
#43513 = CARTESIAN_POINT ( 'NONE',  ( 344.0000000000000000, -167.0000000000001137, -342.0000000000002842 ) ) ;
#43514 = AXIS2_PLACEMENT_3D ( 'NONE', #16505, #17003, #9304 ) ;
#43515 = FACE_OUTER_BOUND ( 'NONE', #819, .T. ) ;
#43516 = DIRECTION ( 'NONE',  ( -1.000000000000000000, -0.000000000000000000, -0.000000000000000000 ) ) ;
#43517 = VECTOR ( 'NONE', #48484, 1000.000000000000000 ) ;
#43518 = CARTESIAN_POINT ( 'NONE',  ( 181.0000000000000568, 175.0000000000000284, 341.9999999999998863 ) ) ;
#43519 = B_SPLINE_CURVE_WITH_KNOTS ( 'NONE', 3,
 ( #49959, #2796, #3050, #45629 ),
 .UNSPECIFIED., .F., .F.,
 ( 4, 4 ),
 ( 0.000000000000000000, 0.0003726855806051465212 ),
 .UNSPECIFIED. ) ;
#43520 = DIRECTION ( 'NONE',  ( 0.3090169943749447312, 0.9510565162951544194, 0.000000000000000000 ) ) ;
#43521 = EDGE_CURVE ( 'NONE', #29044, #36853, #38115, .T. ) ;
#43522 = ORIENTED_EDGE ( 'NONE', *, *, #16957, .F. ) ;
#43523 = DIRECTION ( 'NONE',  ( -0.000000000000000000, -0.000000000000000000, -1.000000000000000000 ) ) ;
#43524 = CARTESIAN_POINT ( 'NONE',  ( -88.44597344681497475, 0.000000000000000000, 159.0682875569279418 ) ) ;
#43525 = ORIENTED_EDGE ( 'NONE', *, *, #1171, .F. ) ;
#43526 = DIRECTION ( 'NONE',  ( -0.000000000000000000, 1.000000000000000000, -0.000000000000000000 ) ) ;
#43527 = DIRECTION ( 'NONE',  ( 0.000000000000000000, 0.000000000000000000, -1.000000000000000000 ) ) ;
#43528 = CARTESIAN_POINT ( 'NONE',  ( -3.975459390375366997, -0.2195152216756601216, -2.642742795433417058E-16 ) ) ;
#43529 = ORIENTED_EDGE ( 'NONE', *, *, #20537, .F. ) ;
#43530 = CARTESIAN_POINT ( 'NONE',  ( 0.7455485644579565863, 0.9687920084208806459, 9.987567862361069970 ) ) ;
#43531 = B_SPLINE_CURVE_WITH_KNOTS ( 'NONE', 3,
 ( #17874, #13524, #45056, #20727 ),
 .UNSPECIFIED., .F., .F.,
 ( 4, 4 ),
 ( 5.641302087905949829E-05, 0.0003272669002638295692 ),
 .UNSPECIFIED. ) ;
#43532 = ORIENTED_EDGE ( 'NONE', *, *, #2352, .T. ) ;
#43533 = ORIENTED_EDGE ( 'NONE', *, *, #26768, .F. ) ;
#43534 = LINE ( 'NONE', #22585, #9484 ) ;
#43535 = DIRECTION ( 'NONE',  ( 0.000000000000000000, 0.000000000000000000, -1.000000000000000000 ) ) ;
#43536 =( BOUNDED_CURVE ( )  B_SPLINE_CURVE ( 3, ( #45890, #30041, #22071, #34393 ),
 .UNSPECIFIED., .F., .F. ) 
 B_SPLINE_CURVE_WITH_KNOTS ( ( 4, 4 ),
 ( 4.712388980384689674, 6.283185307179586232 ),
 .UNSPECIFIED. ) 
 CURVE ( )  GEOMETRIC_REPRESENTATION_ITEM ( )  RATIONAL_B_SPLINE_CURVE ( ( 1.000000000000000000, 0.8047378541243649375, 0.8047378541243649375, 1.000000000000000000 ) ) 
 REPRESENTATION_ITEM ( '' )  );
#43537 = EDGE_CURVE ( 'NONE', #24564, #3086, #11129, .T. ) ;
#43538 = EDGE_CURVE ( 'NONE', #25566, #25084, #45731, .T. ) ;
#43539 = ORIENTED_EDGE ( 'NONE', *, *, #4469, .T. ) ;
#43540 = DIRECTION ( 'NONE',  ( -0.000000000000000000, -1.000000000000000000, -0.000000000000000000 ) ) ;
#43541 = CARTESIAN_POINT ( 'NONE',  ( -164.9459734468149463, 2.143131898507880377E-16, 39.06828755692798438 ) ) ;
#43542 = ORIENTED_EDGE ( 'NONE', *, *, #314, .T. ) ;
#43543 =( BOUNDED_CURVE ( )  B_SPLINE_CURVE ( 3, ( #38559, #15689, #26985, #7500 ),
 .UNSPECIFIED., .F., .F. ) 
 B_SPLINE_CURVE_WITH_KNOTS ( ( 4, 4 ),
 ( 0.000000000000000000, 1.570796326794896558 ),
 .UNSPECIFIED. ) 
 CURVE ( )  GEOMETRIC_REPRESENTATION_ITEM ( )  RATIONAL_B_SPLINE_CURVE ( ( 1.000000000000000000, 0.8047378541243649375, 0.8047378541243649375, 1.000000000000000000 ) ) 
 REPRESENTATION_ITEM ( '' )  );
#43544 = CIRCLE ( 'NONE', #31303, 40.00000000000000000 ) ;
#43545 = EDGE_CURVE ( 'NONE', #14195, #43608, #15481, .T. ) ;
#43546 = LINE ( 'NONE', #8417, #8775 ) ;
#43547 = ORIENTED_EDGE ( 'NONE', *, *, #11750, .T. ) ;
#43549 = EDGE_CURVE ( 'NONE', #15492, #46409, #30379, .T. ) ;
#43548 = DIRECTION ( 'NONE',  ( 3.364279341222519273E-16, -0.7071067811865474617, 0.7071067811865476838 ) ) ;
#43550 = CARTESIAN_POINT ( 'NONE',  ( -84.94597344681494633, 2.143131898507880377E-16, -120.9317124430720156 ) ) ;
#43551 = ADVANCED_FACE ( 'NONE', ( #7275 ), #22921, .T. ) ;
#43552 = FILL_AREA_STYLE ('',( #27660 ) ) ;
#43553 = VERTEX_POINT ( 'NONE', #38598 ) ;
#43554 = DIRECTION ( 'NONE',  ( -1.000000000000000000, -0.000000000000000000, -0.000000000000000000 ) ) ;
#43555 = DIRECTION ( 'NONE',  ( 1.000000000000000000, 0.000000000000000000, 0.000000000000000000 ) ) ;
#43556 = EDGE_LOOP ( 'NONE', ( #36199, #30852, #44575, #41359, #30428, #27509 ) ) ;
#43557 = ORIENTED_EDGE ( 'NONE', *, *, #23803, .F. ) ;
#43558 = VERTEX_POINT ( 'NONE', #3415 ) ;
#43559 = CARTESIAN_POINT ( 'NONE',  ( 193.3040265531851105, 1.750000000000010658, 80.81828755692798438 ) ) ;
#43560 = EDGE_CURVE ( 'NONE', #43960, #34142, #38087, .T. ) ;
#43561 =( BOUNDED_CURVE ( )  B_SPLINE_CURVE ( 3, ( #49069, #21663, #25025, #25774 ),
 .UNSPECIFIED., .F., .F. ) 
 B_SPLINE_CURVE_WITH_KNOTS ( ( 4, 4 ),
 ( 4.712388980384689674, 6.283185307179586232 ),
 .UNSPECIFIED. ) 
 CURVE ( )  GEOMETRIC_REPRESENTATION_ITEM ( )  RATIONAL_B_SPLINE_CURVE ( ( 1.000000000000000000, 0.8047378541243649375, 0.8047378541243649375, 1.000000000000000000 ) ) 
 REPRESENTATION_ITEM ( '' )  );
#43562 = CARTESIAN_POINT ( 'NONE',  ( -65.00000000000002842, 17.00000000000000000, -114.9999999999999858 ) ) ;
#43563 = VECTOR ( 'NONE', #15450, 1000.000000000000000 ) ;
#43564 = ORIENTED_EDGE ( 'NONE', *, *, #11444, .F. ) ;
#43565 = CARTESIAN_POINT ( 'NONE',  ( 31.55402655318506788, 0.000000000000000000, 162.5682875569279702 ) ) ;
#43566 = DIRECTION ( 'NONE',  ( 0.000000000000000000, 0.000000000000000000, -1.000000000000000000 ) ) ;
#43567 = CARTESIAN_POINT ( 'NONE',  ( -208.4459734468149463, 0.000000000000000000, 165.0000000000000000 ) ) ;
#43568 = CARTESIAN_POINT ( 'NONE',  ( 357.9999999999999432, -180.9999999999999716, 355.9999999999998295 ) ) ;
#43569 = CARTESIAN_POINT ( 'NONE',  ( -86.69597344681494633, 1.750000000000009992, 160.8182875569279702 ) ) ;
#43570 = FACE_BOUND ( 'NONE', #9361, .T. ) ;
#43571 = CARTESIAN_POINT ( 'NONE',  ( 210.0000000000000568, 2.143131898507880377E-16, -0.9317124430720331585 ) ) ;
#43572 =( NAMED_UNIT ( * ) SI_UNIT ( $, .STERADIAN. ) SOLID_ANGLE_UNIT ( ) );
#43573 = CARTESIAN_POINT ( 'NONE',  ( 1.540662627795932105, -1.371465786296032441, 9.894754715216729224 ) ) ;
#43574 = CARTESIAN_POINT ( 'NONE',  ( -46.69597344681494633, 0.000000000000000000, -165.0000000000000000 ) ) ;
#43575 = CARTESIAN_POINT ( 'NONE',  ( -1.655785408455817675, -0.7536129375911022610, 9.903764339332079558 ) ) ;
#43576 = FACE_OUTER_BOUND ( 'NONE', #17188, .T. ) ;
#43577 = CARTESIAN_POINT ( 'NONE',  ( 195.9526953830863079, -154.8119894309599260, 470.5025600500171095 ) ) ;
#43578 = LINE ( 'NONE', #36872, #39620 ) ;
#43579 = ORIENTED_EDGE ( 'NONE', *, *, #35307, .T. ) ;
#43580 = CARTESIAN_POINT ( 'NONE',  ( 2.500000000000000444, 224.9999999999999716, -224.9999999999999716 ) ) ;
#43581 = ADVANCED_FACE ( 'NONE', ( #42665 ), #23177, .T. ) ;
#43582 = VECTOR ( 'NONE', #1359, 1000.000000000000000 ) ;
#43583 = CARTESIAN_POINT ( 'NONE',  ( 181.0000000000000568, 165.0000000000000000, 339.9999999999997726 ) ) ;
#43584 = CARTESIAN_POINT ( 'NONE',  ( 7.216980890441427654, -6.922079660550236824, 0.000000000000000000 ) ) ;
#43585 = DIRECTION ( 'NONE',  ( 0.000000000000000000, -0.000000000000000000, -1.000000000000000000 ) ) ;
#43586 = EDGE_CURVE ( 'NONE', #33538, #23358, #23443, .T. ) ;
#43587 = ORIENTED_EDGE ( 'NONE', *, *, #15885, .F. ) ;
#43588 = CARTESIAN_POINT ( 'NONE',  ( 195.9526953830863079, 159.2880105690400399, 472.5992458228020610 ) ) ;
#43589 = AXIS2_PLACEMENT_3D ( 'NONE', #23464, #30657, #47016 ) ;
#43590 = ORIENTED_EDGE ( 'NONE', *, *, #7959, .T. ) ;
#43591 = CARTESIAN_POINT ( 'NONE',  ( -19.99999999999815969, 17.00000000000000000, 65.00000000000000000 ) ) ;
#43592 = FACE_OUTER_BOUND ( 'NONE', #29869, .T. ) ;
#43593 = CARTESIAN_POINT ( 'NONE',  ( 111.5540265531850679, 0.000000000000000000, -120.9317124430720156 ) ) ;
#43594 = ORIENTED_EDGE ( 'NONE', *, *, #25262, .F. ) ;
#43595 = CARTESIAN_POINT ( 'NONE',  ( 33.57695195286775913, 16.69845195084893064, 8.914903342594561408 ) ) ;
#43596 = ORIENTED_EDGE ( 'NONE', *, *, #14357, .T. ) ;
#43597 = VERTEX_POINT ( 'NONE', #49811 ) ;
#43598 = DIRECTION ( 'NONE',  ( 0.000000000000000000, 1.000000000000000000, 0.000000000000000000 ) ) ;
#43599 = DIRECTION ( 'NONE',  ( -0.000000000000000000, -0.000000000000000000, -1.000000000000000000 ) ) ;
#43600 = ORIENTED_EDGE ( 'NONE', *, *, #45666, .F. ) ;
#43601 = DIRECTION ( 'NONE',  ( 0.000000000000000000, -0.000000000000000000, -1.000000000000000000 ) ) ;
#43602 = CARTESIAN_POINT ( 'NONE',  ( -4.945973446814903696, 2.143131898507912917E-16, -37.43171244307200141 ) ) ;
#43603 = CARTESIAN_POINT ( 'NONE',  ( -208.1473046169136580, 160.1880105690400171, 22.84256005001721945 ) ) ;
#43604 = VECTOR ( 'NONE', #37834, 1000.000000000000000 ) ;
#43605 = LINE ( 'NONE', #47928, #43974 ) ;
#43606 = ORIENTED_EDGE ( 'NONE', *, *, #29206, .F. ) ;
#43607 = CARTESIAN_POINT ( 'NONE',  ( -581.3085477938158192, 57.49999999999996447, -68.52876838486925237 ) ) ;
#43608 = VERTEX_POINT ( 'NONE', #27290 ) ;
#43609 = CARTESIAN_POINT ( 'NONE',  ( 113.3040265531850537, 1.749999999999996891, -159.1817124430720298 ) ) ;
#43610 = CARTESIAN_POINT ( 'NONE',  ( 339.9999999999999432, -165.0000000000001137, -349.9999999999998863 ) ) ;
#43611 = AXIS2_PLACEMENT_3D ( 'NONE', #28372, #25522, #5010 ) ;
#43612 = ORIENTED_EDGE ( 'NONE', *, *, #28048, .F. ) ;
#43613 = DIRECTION ( 'NONE',  ( 0.000000000000000000, -0.000000000000000000, -1.000000000000000000 ) ) ;
#43614 = EDGE_CURVE ( 'NONE', #35055, #9213, #39468, .T. ) ;
#43615 = VECTOR ( 'NONE', #30130, 1000.000000000000000 ) ;
#43616 = CARTESIAN_POINT ( 'NONE',  ( 10.00000000000000000, -250.0000000000000000, 225.0000000000000000 ) ) ;
#43617 = ORIENTED_EDGE ( 'NONE', *, *, #15059, .T. ) ;
#43618 = DIRECTION ( 'NONE',  ( -1.000000000000000000, -0.000000000000000000, -0.000000000000000000 ) ) ;
#43619 = CARTESIAN_POINT ( 'NONE',  ( -204.9459734468149463, 2.143131898507880377E-16, 82.56828755692798438 ) ) ;
#43620 = DIRECTION ( 'NONE',  ( 0.000000000000000000, 0.000000000000000000, -1.000000000000000000 ) ) ;
#43621 = AXIS2_PLACEMENT_3D ( 'NONE', #19763, #31329, #47671 ) ;
#43622 = ORIENTED_EDGE ( 'NONE', *, *, #24834, .T. ) ;
#43623 = LINE ( 'NONE', #1552, #43339 ) ;
#43624 = LINE ( 'NONE', #11839, #32468 ) ;
#43625 = CARTESIAN_POINT ( 'NONE',  ( 75.05402655318509630, 2.143131898507880377E-16, 79.06828755692797017 ) ) ;
#43626 = ORIENTED_EDGE ( 'NONE', *, *, #32564, .T. ) ;
#43627 = ORIENTED_EDGE ( 'NONE', *, *, #3439, .F. ) ;
#43628 = APPLICATION_PROTOCOL_DEFINITION ( 'draft international standard', 'automotive_design', 1998, #32208 ) ;
#43629 = FACE_OUTER_BOUND ( 'NONE', #31851, .T. ) ;
#43630 = CARTESIAN_POINT ( 'NONE',  ( 210.0000000000000568, 0.000000000000000000, 40.81828755692798438 ) ) ;
#43631 = FACE_OUTER_BOUND ( 'NONE', #3731, .T. ) ;
#43632 = CARTESIAN_POINT ( 'NONE',  ( -2.143303251558873690, 0.2857918750721046286, 9.885585981620941709 ) ) ;
#43633 = DIRECTION ( 'NONE',  ( -1.000000000000000000, -0.000000000000000000, -0.000000000000000000 ) ) ;
#43634 = ORIENTED_EDGE ( 'NONE', *, *, #21751, .F. ) ;
#43635 = CARTESIAN_POINT ( 'NONE',  ( -168.4459734468149463, 0.000000000000000000, 165.0000000000000000 ) ) ;
#43636 = DIRECTION ( 'NONE',  ( 1.000000000000000000, 0.000000000000000000, 0.000000000000000000 ) ) ;
#43637 = CARTESIAN_POINT ( 'NONE',  ( -7.822422304254325276, 2.683863964738837371, 230.0000000000000000 ) ) ;
#43638 = CARTESIAN_POINT ( 'NONE',  ( 113.3040265531850537, -1.749999999999996891, 0.8182875569279768335 ) ) ;
#43639 = ORIENTED_EDGE ( 'NONE', *, *, #39046, .F. ) ;
#43640 = DIRECTION ( 'NONE',  ( 3.172065745548403743E-16, 1.000000000000000000, 0.000000000000000000 ) ) ;
#43641 = ORIENTED_EDGE ( 'NONE', *, *, #20169, .T. ) ;
#43642 = CARTESIAN_POINT ( 'NONE',  ( 114.3291528190321173, -1.749999999999996891, -40.20683870891911482 ) ) ;
#43643 = ORIENTED_EDGE ( 'NONE', *, *, #48063, .F. ) ;
#43644 = FACE_OUTER_BOUND ( 'NONE', #100, .T. ) ;
#43645 = VECTOR ( 'NONE', #6853, 1000.000000000000000 ) ;
#43646 = DIRECTION ( 'NONE',  ( 1.000000000000000000, 0.000000000000000000, 0.000000000000000000 ) ) ;
#43647 = FACE_OUTER_BOUND ( 'NONE', #41702, .T. ) ;
#43648 = CARTESIAN_POINT ( 'NONE',  ( -164.4973046169135387, 103.0380105690400683, -17.65743994998277699 ) ) ;
#43649 = ORIENTED_EDGE ( 'NONE', *, *, #14343, .T. ) ;
#43650 = AXIS2_PLACEMENT_3D ( 'NONE', #20745, #37431, #9195 ) ;
#43651 = CARTESIAN_POINT ( 'NONE',  ( -207.2473046169136808, -153.9812202001906769, 472.4964062038633870 ) ) ;
#43652 = VECTOR ( 'NONE', #5967, 1000.000000000000000 ) ;
#43653 = CARTESIAN_POINT ( 'NONE',  ( 177.5000000000000000, 112.5000000000000000, -10.00000000000000178 ) ) ;
#43654 = ORIENTED_EDGE ( 'NONE', *, *, #13, .F. ) ;
#43655 = DIRECTION ( 'NONE',  ( 3.614007241618348278E-16, 1.000000000000000000, 0.000000000000000000 ) ) ;
#43656 = DIRECTION ( 'NONE',  ( 0.000000000000000000, 1.000000000000000000, 6.123233995736766036E-17 ) ) ;
#43657 = DIRECTION ( 'NONE',  ( -0.6904757466825006684, -0.7233555441435720601, 0.000000000000000000 ) ) ;
#43658 = CARTESIAN_POINT ( 'NONE',  ( -206.6959734468149463, -1.750000000000009992, 0.8182875569279768335 ) ) ;
#43659 = EDGE_LOOP ( 'NONE', ( #42031, #13885, #42975, #50652 ) ) ;
#43660 = VERTEX_POINT ( 'NONE', #14467 ) ;
#43661 = CARTESIAN_POINT ( 'NONE',  ( 112.2789002873379758, -1.749999999999996891, -118.1565861772249661 ) ) ;
#43662 = ORIENTED_EDGE ( 'NONE', *, *, #38628, .T. ) ;
#43663 = CARTESIAN_POINT ( 'NONE',  ( 85.00000000000123634, 17.00000000000000000, 30.00000000000000000 ) ) ;
#43664 = FACE_OUTER_BOUND ( 'NONE', #2046, .T. ) ;
#43665 = DIRECTION ( 'NONE',  ( 0.000000000000000000, 0.000000000000000000, -1.000000000000000000 ) ) ;
#43666 = ORIENTED_EDGE ( 'NONE', *, *, #28513, .T. ) ;
#43667 = CARTESIAN_POINT ( 'NONE',  ( 194.3291528190321742, 1.750000000000010214, 79.79316129108087807 ) ) ;
#43668 = EDGE_CURVE ( 'NONE', #16142, #5465, #39602, .T. ) ;
#43669 = EDGE_CURVE ( 'NONE', #34532, #6290, #31910, .T. ) ;
#43670 = CYLINDRICAL_SURFACE ( 'NONE', #30836, 1.749999999999973799 ) ;
#43671 = ADVANCED_FACE ( 'NONE', ( #4193 ), #6902, .T. ) ;
#43672 = DIRECTION ( 'NONE',  ( 0.000000000000000000, -0.000000000000000000, 1.000000000000000000 ) ) ;
#43673 = EDGE_LOOP ( 'NONE', ( #1718, #36446, #48003, #24568 ) ) ;
#43674 = ORIENTED_EDGE ( 'NONE', *, *, #40813, .T. ) ;
#43675 = AXIS2_PLACEMENT_3D ( 'NONE', #23543, #16339, #46584 ) ;
#43676 = ORIENTED_EDGE ( 'NONE', *, *, #1502, .F. ) ;
#43677 = DIRECTION ( 'NONE',  ( -1.000000000000000000, 0.000000000000000000, 0.000000000000000000 ) ) ;
#43678 = VECTOR ( 'NONE', #22436, 1000.000000000000000 ) ;
#43679 = EDGE_CURVE ( 'NONE', #4741, #16142, #28295, .T. ) ;
#43680 = CARTESIAN_POINT ( 'NONE',  ( 164.9999999999999716, 175.0000000000000284, -340.0000000000001137 ) ) ;
#43681 = ADVANCED_FACE ( 'NONE', ( #16244 ), #47502, .F. ) ;
#43682 = PRODUCT_DEFINITION_CONTEXT ( 'detailed design', #42372, 'design' ) ;
#43683 = VERTEX_POINT ( 'NONE', #24458 ) ;
#43684 = CARTESIAN_POINT ( 'NONE',  ( 0.000000000000000000, 17.00000000000000000, 0.000000000000000000 ) ) ;
#43685 = ORIENTED_EDGE ( 'NONE', *, *, #23321, .F. ) ;
#43686 = VECTOR ( 'NONE', #11037, 1000.000000000000000 ) ;
#43687 = LINE ( 'NONE', #4946, #1263 ) ;
#43688 = ORIENTED_EDGE ( 'NONE', *, *, #29011, .F. ) ;
#43689 = ADVANCED_FACE ( 'NONE', ( #8050 ), #31664, .F. ) ;
#43690 = CARTESIAN_POINT ( 'NONE',  ( -165.3973046169136012, -98.56198943095992604, -17.65743994998277699 ) ) ;
#43691 =( BOUNDED_CURVE ( )  B_SPLINE_CURVE ( 3, ( #2917, #34246, #41430, #7045 ),
 .UNSPECIFIED., .F., .F. ) 
 B_SPLINE_CURVE_WITH_KNOTS ( ( 4, 4 ),
 ( 3.141592653589793116, 4.712388980384689674 ),
 .UNSPECIFIED. ) 
 CURVE ( )  GEOMETRIC_REPRESENTATION_ITEM ( )  RATIONAL_B_SPLINE_CURVE ( ( 1.000000000000000000, 0.8047378541243649375, 0.8047378541243649375, 1.000000000000000000 ) ) 
 REPRESENTATION_ITEM ( '' )  );
#43692 = DIRECTION ( 'NONE',  ( 1.000000000000000000, -0.000000000000000000, 0.000000000000000000 ) ) ;
#43694 = B_SPLINE_CURVE_WITH_KNOTS ( 'NONE', 3,
 ( #19169, #27911, #43029, #26884 ),
 .UNSPECIFIED., .F., .F.,
 ( 4, 4 ),
 ( 0.8097120833243680593, 0.9322955464062570030 ),
 .UNSPECIFIED. ) ;
#43693 = AXIS2_PLACEMENT_3D ( 'NONE', #25412, #33376, #29510 ) ;
#43695 = CARTESIAN_POINT ( 'NONE',  ( 0.000000000000000000, -33.89193117067290473, 910.0000000000000000 ) ) ;
#43696 = CARTESIAN_POINT ( 'NONE',  ( -126.6959734468149321, -1.749999999999997335, 80.81828755692798438 ) ) ;
#43697 = VERTEX_POINT ( 'NONE', #35254 ) ;
#43698 = ORIENTED_EDGE ( 'NONE', *, *, #17490, .T. ) ;
#43699 = CARTESIAN_POINT ( 'NONE',  ( 350.0000000000000000, -180.9999999999999716, -340.0000000000001705 ) ) ;
#43700 =( BOUNDED_CURVE ( )  B_SPLINE_CURVE ( 3, ( #28561, #40123, #39881, #47266 ),
 .UNSPECIFIED., .F., .F. ) 
 B_SPLINE_CURVE_WITH_KNOTS ( ( 4, 4 ),
 ( 0.000000000000000000, 1.570796326794896558 ),
 .UNSPECIFIED. ) 
 CURVE ( )  GEOMETRIC_REPRESENTATION_ITEM ( )  RATIONAL_B_SPLINE_CURVE ( ( 1.000000000000000000, 0.8047378541243649375, 0.8047378541243649375, 1.000000000000000000 ) ) 
 REPRESENTATION_ITEM ( '' )  );
#43701 = B_SPLINE_SURFACE_WITH_KNOTS ( 'NONE', 3, 3, ( 
 ( #37899, #21712, #33030, #48616 ),
 ( #14006, #25074, #44531, #26073 ),
 ( #37400, #14262, #29926, #33289 ),
 ( #45542, #22224, #9416, #10171 ) ),
 .UNSPECIFIED., .F., .F., .F.,
 ( 4, 4 ),
 ( 4, 4 ),
 ( 0.000000000000000000, 1.000000000000000000 ),
 ( 0.000000000000000000, 1.000000000000000000 ),
 .UNSPECIFIED. ) ;
#43702 = CARTESIAN_POINT ( 'NONE',  ( 153.3040265531850537, 0.000000000000000000, 165.0000000000000000 ) ) ;
#43703 = DIRECTION ( 'NONE',  ( 0.000000000000000000, 0.000000000000000000, 1.000000000000000000 ) ) ;
#43704 = EDGE_CURVE ( 'NONE', #15488, #37293, #97, .T. ) ;
#43705 = EDGE_CURVE ( 'NONE', #10853, #5199, #24203, .T. ) ;
#43706 = EDGE_CURVE ( 'NONE', #20580, #49549, #20020, .T. ) ;
#43707 = EDGE_CURVE ( 'NONE', #30294, #48563, #4936, .T. ) ;
#43708 = VECTOR ( 'NONE', #16509, 1000.000000000000000 ) ;
#43709 = CARTESIAN_POINT ( 'NONE',  ( -19.99999999999940670, 17.00000000000000000, -54.99999999999999289 ) ) ;
#43710 = CARTESIAN_POINT ( 'NONE',  ( -164.9999999999997442, 17.00000000000000000, -60.00000000000000000 ) ) ;
#43711 = EDGE_CURVE ( 'NONE', #4061, #45368, #39354, .T. ) ;
#43712 = ORIENTED_EDGE ( 'NONE', *, *, #9831, .F. ) ;
#43713 = LINE ( 'NONE', #35540, #46671 ) ;
#43714 = ADVANCED_FACE ( 'NONE', ( #1106, #48000 ), #12889, .F. ) ;
#43715 = B_SPLINE_CURVE_WITH_KNOTS ( 'NONE', 3,
 ( #37861, #35036, #11658, #15262 ),
 .UNSPECIFIED., .F., .F.,
 ( 4, 4 ),
 ( 0.7491799374948678869, 1.000000000000000000 ),
 .UNSPECIFIED. ) ;
#43716 = CARTESIAN_POINT ( 'NONE',  ( 191.5540265531850537, 1.025126265847088991, 2.568287556927986159 ) ) ;
#43717 = ORIENTED_EDGE ( 'NONE', *, *, #27233, .F. ) ;
#43718 = FACE_OUTER_BOUND ( 'NONE', #37790, .T. ) ;
#43719 = CARTESIAN_POINT ( 'NONE',  ( -1.249999999999999778, 0.000000000000000000, -10.00000000000000000 ) ) ;
#43720 = DIRECTION ( 'NONE',  ( 0.000000000000000000, 1.000000000000000000, -2.537652627714643577E-15 ) ) ;
#43721 = CARTESIAN_POINT ( 'NONE',  ( -114.9999999999987779, 17.00000000000000000, 5.000000000000004441 ) ) ;
#43722 = ORIENTED_EDGE ( 'NONE', *, *, #28417, .T. ) ;
#43723 = VERTEX_POINT ( 'NONE', #12145 ) ;
#43724 = EDGE_CURVE ( 'NONE', #27459, #19049, #33783, .T. ) ;
#43725 = CARTESIAN_POINT ( 'NONE',  ( -194.9999999999999432, -172.9999999999999716, 232.0000000000000284 ) ) ;
#43726 = VECTOR ( 'NONE', #21504, 1000.000000000000000 ) ;
#43727 = VECTOR ( 'NONE', #47383, 1000.000000000000000 ) ;
#43728 = ADVANCED_FACE ( 'NONE', ( #36776 ), #29810, .F. ) ;
#43729 = EDGE_LOOP ( 'NONE', ( #25604, #2142, #16059, #44208 ) ) ;
#43730 = EDGE_CURVE ( 'NONE', #29224, #9824, #21346, .T. ) ;
#43731 = ORIENTED_EDGE ( 'NONE', *, *, #27508, .T. ) ;
#43732 = CARTESIAN_POINT ( 'NONE',  ( -47.72109971266203132, 1.750000000000009548, -38.15658617722494483 ) ) ;
#43733 = CARTESIAN_POINT ( 'NONE',  ( 35.05402655318504657, 1.025126265847089657, 42.56828755692799149 ) ) ;
#43734 = CARTESIAN_POINT ( 'NONE',  ( 45.42829307628542779, 21.98948915213303579, 8.356839323120299312 ) ) ;
#43735 = DIRECTION ( 'NONE',  ( -0.000000000000000000, -0.000000000000000000, -1.000000000000000000 ) ) ;
#43736 = ORIENTED_EDGE ( 'NONE', *, *, #41920, .F. ) ;
#43737 = ORIENTED_EDGE ( 'NONE', *, *, #17196, .T. ) ;
#43738 = EDGE_CURVE ( 'NONE', #35096, #46138, #36521, .T. ) ;
#43739 = ORIENTED_EDGE ( 'NONE', *, *, #28856, .T. ) ;
#43740 = ADVANCED_FACE ( 'NONE', ( #48503 ), #1611, .T. ) ;
#43741 = DIRECTION ( 'NONE',  ( 1.156482317317870492E-16, -1.000000000000000000, -0.000000000000000000 ) ) ;
#43742 = ORIENTED_EDGE ( 'NONE', *, *, #46193, .F. ) ;
#43743 = VECTOR ( 'NONE', #49395, 1000.000000000000000 ) ;
#43744 = CARTESIAN_POINT ( 'NONE',  ( 4.999999999999999112, 175.0000000000000284, -353.7500000000001705 ) ) ;
#43745 = ORIENTED_EDGE ( 'NONE', *, *, #4642, .F. ) ;
#43746 = VERTEX_POINT ( 'NONE', #40846 ) ;
#43747 = DIRECTION ( 'NONE',  ( -1.000000000000000000, 0.000000000000000000, 1.860490536778032451E-50 ) ) ;
#43748 = LINE ( 'NONE', #39927, #10127 ) ;
#43749 = ORIENTED_EDGE ( 'NONE', *, *, #46269, .T. ) ;
#43750 = ORIENTED_EDGE ( 'NONE', *, *, #1859, .F. ) ;
#43751 = EDGE_CURVE ( 'NONE', #41868, #37688, #44426, .T. ) ;
#43752 = CYLINDRICAL_SURFACE ( 'NONE', #5308, 5.000000000000000000 ) ;
#43753 = LINE ( 'NONE', #39675, #49317 ) ;
#43754 = ORIENTED_EDGE ( 'NONE', *, *, #37164, .F. ) ;
#43755 = CARTESIAN_POINT ( 'NONE',  ( 210.0000000000000568, 2.143131898507881856E-16, 119.0682875569279560 ) ) ;
#43756 = CARTESIAN_POINT ( 'NONE',  ( -208.4459734468148611, 1.025126265847089435, 122.5682875569280128 ) ) ;
#43757 = CARTESIAN_POINT ( 'NONE',  ( -1.962712821592842882, -1.022159834731130257, 9.881002359080275355 ) ) ;
#43758 = VECTOR ( 'NONE', #47926, 1000.000000000000000 ) ;
#43759 = VECTOR ( 'NONE', #44787, 1000.000000000000000 ) ;
#43760 = ADVANCED_FACE ( 'NONE', ( #13884 ), #9298, .F. ) ;
#43761 = DIRECTION ( 'NONE',  ( -1.000000000000000000, 0.000000000000000000, 0.000000000000000000 ) ) ;
#43762 = VERTEX_POINT ( 'NONE', #32655 ) ;
#43763 = VECTOR ( 'NONE', #33639, 1000.000000000000000 ) ;
#43764 = PLANE ( 'NONE',  #32435 ) ;
#43765 = CYLINDRICAL_SURFACE ( 'NONE', #11763, 1.750000000000001554 ) ;
#43766 = DIRECTION ( 'NONE',  ( 0.000000000000000000, 0.000000000000000000, 1.000000000000000000 ) ) ;
#43767 = CARTESIAN_POINT ( 'NONE',  ( -88.44597344681497475, 0.000000000000000000, 165.0000000000000000 ) ) ;
#43768 = EDGE_CURVE ( 'NONE', #35926, #609, #28026, .T. ) ;
#43769 = EDGE_CURVE ( 'NONE', #16395, #22572, #17994, .T. ) ;
#43770 = ADVANCED_FACE ( 'NONE', ( #29551 ), #40607, .T. ) ;
#43771 = DIRECTION ( 'NONE',  ( 1.000000000000000000, 0.000000000000000000, 0.000000000000000000 ) ) ;
#43772 = B_SPLINE_CURVE_WITH_KNOTS ( 'NONE', 3,
 ( #40701, #48592, #28137, #29150 ),
 .UNSPECIFIED., .F., .F.,
 ( 4, 4 ),
 ( 0.9890644561682315761, 1.000000000000000000 ),
 .UNSPECIFIED. ) ;
#43773 = EDGE_CURVE ( 'NONE', #15646, #15638, #43332, .T. ) ;
#43774 = LINE ( 'NONE', #8881, #28300 ) ;
#43775 = CARTESIAN_POINT ( 'NONE',  ( 0.3862712429686978033, -1.188820645368937834, -10.00000000000000000 ) ) ;
#43776 = EDGE_CURVE ( 'NONE', #31636, #29723, #17254, .T. ) ;
#43777 = ORIENTED_EDGE ( 'NONE', *, *, #16558, .T. ) ;
#43778 = CARTESIAN_POINT ( 'NONE',  ( -33.38053581724533814, -17.16548397897120282, 4.835783797351804303 ) ) ;
#43779 = ORIENTED_EDGE ( 'NONE', *, *, #18370, .F. ) ;
#43780 = CARTESIAN_POINT ( 'NONE',  ( 166.9999999999999716, 6.000000000000060396, -350.0000000000001705 ) ) ;
#43781 = CARTESIAN_POINT ( 'NONE',  ( 34.95136153415558056, -36.40974830873469870, 8.356839323120299312 ) ) ;
#43782 = PLANE ( 'NONE',  #4526 ) ;
#43783 = VERTEX_POINT ( 'NONE', #49256 ) ;
#43784 = CARTESIAN_POINT ( 'NONE',  ( 193.3040265531851105, 1.750000000000010658, -119.1817124430720440 ) ) ;
#43785 = ORIENTED_EDGE ( 'NONE', *, *, #44013, .T. ) ;
#43786 = ORIENTED_EDGE ( 'NONE', *, *, #21454, .T. ) ;
#43787 = DIRECTION ( 'NONE',  ( -1.000000000000000000, -0.000000000000000000, -0.000000000000000000 ) ) ;
#43788 = CARTESIAN_POINT ( 'NONE',  ( 342.0000000000000000, 165.0000000000000000, -94.00000000000019895 ) ) ;
#43789 = VERTEX_POINT ( 'NONE', #33176 ) ;
#43790 = EDGE_CURVE ( 'NONE', #47214, #18098, #5080, .T. ) ;
#43791 = CARTESIAN_POINT ( 'NONE',  ( 240.0000000000000000, -164.9999999999999716, 62.29650858650038003 ) ) ;
#43792 = DIRECTION ( 'NONE',  ( 0.000000000000000000, 0.000000000000000000, 1.000000000000000000 ) ) ;
#43793 = VECTOR ( 'NONE', #45348, 1000.000000000000000 ) ;
#43794 = VERTEX_POINT ( 'NONE', #21597 ) ;
#43795 = CARTESIAN_POINT ( 'NONE',  ( -69.99999999999816680, 17.00000000000000000, 65.00000000000000000 ) ) ;
#43796 = ORIENTED_EDGE ( 'NONE', *, *, #4877, .F. ) ;
#43797 = AXIS2_PLACEMENT_3D ( 'NONE', #3610, #23625, #39041 ) ;
#43798 = CARTESIAN_POINT ( 'NONE',  ( -86.69597344681494633, -1.750000000000010214, 40.81828755692798438 ) ) ;
#43799 = CARTESIAN_POINT ( 'NONE',  ( 167.0000000000000000, -174.9999999999999716, -99.00000000000014211 ) ) ;
#43800 = DIRECTION ( 'NONE',  ( 0.000000000000000000, 0.000000000000000000, 1.000000000000000000 ) ) ;
#43801 = ORIENTED_EDGE ( 'NONE', *, *, #31944, .F. ) ;
#43802 = CARTESIAN_POINT ( 'NONE',  ( 12.35406723005396046, -11.51001571518080624, 9.178419661560148768 ) ) ;
#43803 = CARTESIAN_POINT ( 'NONE',  ( 168.9999999999999716, -164.9999999999999432, -340.0000000000001137 ) ) ;
#43804 = EDGE_LOOP ( 'NONE', ( #8396, #1411, #39394, #42711 ) ) ;
#43805 = ORIENTED_EDGE ( 'NONE', *, *, #22988, .T. ) ;
#43806 = ORIENTED_EDGE ( 'NONE', *, *, #33839, .F. ) ;
#43807 = CARTESIAN_POINT ( 'NONE',  ( 9.221081804193270059, 13.81382350053991104, 3.266473740018926541 ) ) ;
#43808 = EDGE_CURVE ( 'NONE', #42453, #43432, #34515, .T. ) ;
#43809 = FACE_OUTER_BOUND ( 'NONE', #5980, .T. ) ;
#43810 = ORIENTED_EDGE ( 'NONE', *, *, #12788, .T. ) ;
#43811 = B_SPLINE_CURVE_WITH_KNOTS ( 'NONE', 3,
 ( #31481, #19144, #4275, #27116 ),
 .UNSPECIFIED., .F., .F.,
 ( 4, 4 ),
 ( 0.8097120833243680593, 0.9322955464061821740 ),
 .UNSPECIFIED. ) ;
#43812 = CARTESIAN_POINT ( 'NONE',  ( 210.0000000000000568, 0.000000000000000000, 40.81828755692798438 ) ) ;
#43813 = CARTESIAN_POINT ( 'NONE',  ( 193.3040265531851105, 1.750000000000010658, -79.18171244307201562 ) ) ;
#43814 = CARTESIAN_POINT ( 'NONE',  ( 50.00000000000000000, -50.00000000000000000, 800.0000000000000000 ) ) ;
#43815 = VECTOR ( 'NONE', #23013, 1000.000000000000000 ) ;
#43816 = CARTESIAN_POINT ( 'NONE',  ( -0.2773062244624664441, 1.251557370488897813, 9.948547179989621014 ) ) ;
#43817 = CARTESIAN_POINT ( 'NONE',  ( 177.5000000000000000, 74.83106485270648989, -130.5992382549688955 ) ) ;
#43818 = CARTESIAN_POINT ( 'NONE',  ( -1.377636575563021992, 0.6021164824561227036, 9.953784399990620813 ) ) ;
#43819 = CIRCLE ( 'NONE', #21693, 4.000000000000003553 ) ;
#43820 = DIRECTION ( 'NONE',  ( -1.000000000000000000, 0.000000000000000000, 0.000000000000000000 ) ) ;
#43821 = DIRECTION ( 'NONE',  ( 0.000000000000000000, -0.000000000000000000, -1.000000000000000000 ) ) ;
#43822 = CARTESIAN_POINT ( 'NONE',  ( 47.87295225382209907, 14.46560184742433641, -2.408242355805840784 ) ) ;
#43823 = CARTESIAN_POINT ( 'NONE',  ( 341.9999999999999432, 171.9999999999999432, -347.0000000000000568 ) ) ;
#43824 = EDGE_CURVE ( 'NONE', #2268, #41040, #35112, .T. ) ;
#43825 = EDGE_CURVE ( 'NONE', #27084, #15777, #37291, .T. ) ;
#43826 = VECTOR ( 'NONE', #18027, 999.9999999999998863 ) ;
#43827 = CARTESIAN_POINT ( 'NONE',  ( 10.00000000000000000, -250.0000000000000000, 225.0000000000000000 ) ) ;
#43828 = VERTEX_POINT ( 'NONE', #14406 ) ;
#43829 = CARTESIAN_POINT ( 'NONE',  ( -204.9459734468149463, 2.143131898507880377E-16, 159.0682875569279702 ) ) ;
#43830 = EDGE_CURVE ( 'NONE', #45897, #297, #2843, .T. ) ;
#43831 = CARTESIAN_POINT ( 'NONE',  ( 135.0000000000012790, 17.00000000000000000, 30.00000000000000000 ) ) ;
#43832 = CARTESIAN_POINT ( 'NONE',  ( 349.9999999999999432, -164.9999999999999432, 343.9999999999997726 ) ) ;
#43833 = VECTOR ( 'NONE', #14022, 1000.000000000000000 ) ;
#43834 = CARTESIAN_POINT ( 'NONE',  ( 5.551115123125782702E-14, -180.9999999999999716, 357.9999999999997726 ) ) ;
#43835 = ADVANCED_FACE ( 'NONE', ( #22612, #50259 ), #45926, .T. ) ;
#43836 = EDGE_CURVE ( 'NONE', #21938, #13831, #10807, .T. ) ;
#43837 =( BOUNDED_CURVE ( )  B_SPLINE_CURVE ( 3, ( #35220, #15445, #27256, #23135 ),
 .UNSPECIFIED., .F., .F. ) 
 B_SPLINE_CURVE_WITH_KNOTS ( ( 4, 4 ),
 ( 0.000000000000000000, 1.570796326794896558 ),
 .UNSPECIFIED. ) 
 CURVE ( )  GEOMETRIC_REPRESENTATION_ITEM ( )  RATIONAL_B_SPLINE_CURVE ( ( 1.000000000000000000, 0.8047378541243649375, 0.8047378541243649375, 1.000000000000000000 ) ) 
 REPRESENTATION_ITEM ( '' )  );
#43838 = EDGE_LOOP ( 'NONE', ( #1310, #27767, #33315, #10081, #44638, #49746, #7834, #40287, #35841, #42170, #32633, #41735 ) ) ;
#43839 = LINE ( 'NONE', #47151, #30514 ) ;
#43840 = CARTESIAN_POINT ( 'NONE',  ( 85.00000000000090949, 17.00000000000000000, -24.99999999999999289 ) ) ;
#43841 = ORIENTED_EDGE ( 'NONE', *, *, #23991, .T. ) ;
#43842 = CARTESIAN_POINT ( 'NONE',  ( 130.0000000000015064, 17.00000000000000000, 60.00000000000000000 ) ) ;
#43843 = PLANE ( 'NONE',  #41314 ) ;
#43844 = CARTESIAN_POINT ( 'NONE',  ( -45.67084718096785423, 1.750000000000009548, -0.2068387089191121020 ) ) ;
#43845 =( BOUNDED_CURVE ( )  B_SPLINE_CURVE ( 3, ( #36697, #40767, #1521, #13551 ),
 .UNSPECIFIED., .F., .F. ) 
 B_SPLINE_CURVE_WITH_KNOTS ( ( 4, 4 ),
 ( 1.570796326794896558, 3.141592653589793116 ),
 .UNSPECIFIED. ) 
 CURVE ( )  GEOMETRIC_REPRESENTATION_ITEM ( )  RATIONAL_B_SPLINE_CURVE ( ( 1.000000000000000000, 0.8047378541243649375, 0.8047378541243649375, 1.000000000000000000 ) ) 
 REPRESENTATION_ITEM ( '' )  );
#43846 = ADVANCED_FACE ( 'NONE', ( #15425 ), #26967, .T. ) ;
#43847 = VERTEX_POINT ( 'NONE', #41608 ) ;
#43848 = DIRECTION ( 'NONE',  ( -3.172065784643302499E-16, -1.000000000000000000, 2.537652627714642000E-15 ) ) ;
#43849 = VERTEX_POINT ( 'NONE', #38028 ) ;
#43850 = ORIENTED_EDGE ( 'NONE', *, *, #16717, .T. ) ;
#43851 = EDGE_LOOP ( 'NONE', ( #42150, #24343 ) ) ;
#43852 = CARTESIAN_POINT ( 'NONE',  ( 175.0000000000000000, 0.000000000000000000, -122.5000000000000000 ) ) ;
#43853 = CARTESIAN_POINT ( 'NONE',  ( 111.5540265531850679, 0.000000000000000000, 165.0000000000000000 ) ) ;
#43854 = CIRCLE ( 'NONE', #13527, 1.750000000000015543 ) ;
#43855 = ORIENTED_EDGE ( 'NONE', *, *, #17834, .F. ) ;
#43856 = CARTESIAN_POINT ( 'NONE',  ( -119.9999999999987921, 17.00000000000000000, 5.000000000000004441 ) ) ;
#43857 = CARTESIAN_POINT ( 'NONE',  ( -15.00000000000000000, 0.000000000000000000, 0.000000000000000000 ) ) ;
#43858 = VECTOR ( 'NONE', #15434, 1000.000000000000000 ) ;
#43859 =( BOUNDED_CURVE ( )  B_SPLINE_CURVE ( 3, ( #32984, #10115, #33982, #41670 ),
 .UNSPECIFIED., .F., .F. ) 
 B_SPLINE_CURVE_WITH_KNOTS ( ( 4, 4 ),
 ( 0.000000000000000000, 1.570796326794896558 ),
 .UNSPECIFIED. ) 
 CURVE ( )  GEOMETRIC_REPRESENTATION_ITEM ( )  RATIONAL_B_SPLINE_CURVE ( ( 1.000000000000000000, 0.8047378541243649375, 0.8047378541243649375, 1.000000000000000000 ) ) 
 REPRESENTATION_ITEM ( '' )  );
#43860 = CARTESIAN_POINT ( 'NONE',  ( -26.76882631152605185, 42.35470813487695807, -8.917361510505369182 ) ) ;
#43861 = ORIENTED_EDGE ( 'NONE', *, *, #16208, .F. ) ;
#43862 = DIRECTION ( 'NONE',  ( 0.000000000000000000, -1.000000000000000000, 0.000000000000000000 ) ) ;
#43863 = VERTEX_POINT ( 'NONE', #2593 ) ;
#43864 = CARTESIAN_POINT ( 'NONE',  ( 0.6595498452743703277, -16.59563386392009576, 3.266473740018926541 ) ) ;
#43865 = AXIS2_PLACEMENT_3D ( 'NONE', #45242, #6525, #10387 ) ;
#43866 = CARTESIAN_POINT ( 'NONE',  ( 154.3291528190321458, -1.750000000000009548, 41.84341382277508359 ) ) ;
#43867 = VECTOR ( 'NONE', #23823, 1000.000000000000000 ) ;
#43868 = ORIENTED_EDGE ( 'NONE', *, *, #29003, .T. ) ;
#43869 = LINE ( 'NONE', #5120, #44211 ) ;
#43870 =( GEOMETRIC_REPRESENTATION_CONTEXT ( 3 ) GLOBAL_UNCERTAINTY_ASSIGNED_CONTEXT ( ( #15216 ) ) GLOBAL_UNIT_ASSIGNED_CONTEXT ( ( #32165, #4949, #5458 ) ) REPRESENTATION_CONTEXT ( 'NONE', 'WORKASPACE' ) );
#43871 = DIRECTION ( 'NONE',  ( -0.000000000000000000, 1.000000000000000000, 0.000000000000000000 ) ) ;
#43872 = ORIENTED_EDGE ( 'NONE', *, *, #35248, .T. ) ;
#43873 = VECTOR ( 'NONE', #28936, 1000.000000000000000 ) ;
#43874 = EDGE_CURVE ( 'NONE', #32522, #20901, #41859, .T. ) ;
#43875 = CARTESIAN_POINT ( 'NONE',  ( 0.9870575514054733546, 1.980598328282569653, 9.881002359080278907 ) ) ;
#43876 = CARTESIAN_POINT ( 'NONE',  ( 0.6215990105956902267, -1.608617984725389860, 9.928159647716132241 ) ) ;
#43877 = CARTESIAN_POINT ( 'NONE',  ( 210.0000000000000568, 0.000000000000000000, 162.5682875569279702 ) ) ;
#43878 = LINE ( 'NONE', #12325, #28832 ) ;
#43879 = ORIENTED_EDGE ( 'NONE', *, *, #26579, .F. ) ;
#43880 = DIRECTION ( 'NONE',  ( -1.000000000000000000, 0.000000000000000000, 0.000000000000000000 ) ) ;
#43881 = LINE ( 'NONE', #35202, #33271 ) ;
#43882 = DIRECTION ( 'NONE',  ( 0.7233555441435720601, -0.6904757466825007794, 0.000000000000000000 ) ) ;
#43883 = VERTEX_POINT ( 'NONE', #34688 ) ;
#43884 = VERTEX_POINT ( 'NONE', #46686 ) ;
#43885 = APPLICATION_PROTOCOL_DEFINITION ( 'draft international standard', 'automotive_design', 1998, #435 ) ;
#43886 = DIRECTION ( 'NONE',  ( 1.000000000000000000, -0.000000000000000000, -0.000000000000000000 ) ) ;
#43887 = DIRECTION ( 'NONE',  ( -1.000000000000000000, 0.000000000000000000, 0.000000000000000000 ) ) ;
#43888 = CARTESIAN_POINT ( 'NONE',  ( -165.0000000000000284, 16.00000000000000000, -114.9999999999999858 ) ) ;
#43890 = VECTOR ( 'NONE', #28360, 1000.000000000000000 ) ;
#43889 = DIRECTION ( 'NONE',  ( -1.000000000000000000, 0.000000000000000000, 0.000000000000000000 ) ) ;
#43891 = CARTESIAN_POINT ( 'NONE',  ( -14.99999999999970868, 16.00000000000000000, -60.00000000000000000 ) ) ;
#43892 = ORIENTED_EDGE ( 'NONE', *, *, #17121, .F. ) ;
#43893 = AXIS2_PLACEMENT_3D ( 'NONE', #42438, #6794, #38620 ) ;
#43894 = CARTESIAN_POINT ( 'NONE',  ( 228.9999999999999716, -169.9999999999999716, 62.29650858650038003 ) ) ;
#43895 = CARTESIAN_POINT ( 'NONE',  ( 0.000000000000000000, 0.000000000000000000, 790.0000000000000000 ) ) ;
#43896 = EDGE_CURVE ( 'NONE', #4645, #49554, #38294, .T. ) ;
#43897 = CIRCLE ( 'NONE', #7886, 0.4999999999999992228 ) ;
#43898 = ORIENTED_EDGE ( 'NONE', *, *, #17978, .F. ) ;
#43899 = CARTESIAN_POINT ( 'NONE',  ( 151.5540265531850537, 1.025126265847089435, -40.93171244307204404 ) ) ;
#43900 = ORIENTED_EDGE ( 'NONE', *, *, #40948, .F. ) ;
#43901 = DIRECTION ( 'NONE',  ( 0.000000000000000000, 0.000000000000000000, 1.000000000000000000 ) ) ;
#43902 = VECTOR ( 'NONE', #25977, 1000.000000000000000 ) ;
#43903 = VERTEX_POINT ( 'NONE', #31080 ) ;
#43904 = EDGE_CURVE ( 'NONE', #29317, #45409, #30831, .T. ) ;
#43905 = CARTESIAN_POINT ( 'NONE',  ( -206.6959734468149463, 1.750000000000009992, 160.8182875569279702 ) ) ;
#43906 = DIRECTION ( 'NONE',  ( -0.000000000000000000, -0.000000000000000000, -1.000000000000000000 ) ) ;
#43907 = DIRECTION ( 'NONE',  ( 1.000000000000000000, 0.000000000000000000, -1.860490536778032451E-50 ) ) ;
#43908 = ORIENTED_EDGE ( 'NONE', *, *, #20903, .T. ) ;
#43909 = VECTOR ( 'NONE', #5806, 1000.000000000000000 ) ;
#43910 = CARTESIAN_POINT ( 'NONE',  ( -6.619412807845042046, 7.495556955913086128, 9.646707543097347681 ) ) ;
#43911 = CARTESIAN_POINT ( 'NONE',  ( 6.123233995736766282E-16, 28.48684210526315752, 5.000000000000000000 ) ) ;
#43912 = EDGE_LOOP ( 'NONE', ( #33402, #2562, #45331, #23171 ) ) ;
#43913 = DIRECTION ( 'NONE',  ( 1.156482317317870492E-16, -1.000000000000000000, -0.000000000000000000 ) ) ;
#43914 = CARTESIAN_POINT ( 'NONE',  ( 358.0000000000001137, 181.0000000000000284, 349.9999999999998295 ) ) ;
#43915 = CARTESIAN_POINT ( 'NONE',  ( 1.578643388466006714, -1.550786058692517511, 9.881002359080275355 ) ) ;
#43916 = DIRECTION ( 'NONE',  ( -1.000000000000000000, -0.000000000000000000, -0.000000000000000000 ) ) ;
#43917 = ORIENTED_EDGE ( 'NONE', *, *, #38385, .T. ) ;
#43918 = ORIENTED_EDGE ( 'NONE', *, *, #7021, .F. ) ;
#43919 = LINE ( 'NONE', #36765, #25945 ) ;
#43920 = VECTOR ( 'NONE', #42082, 1000.000000000000000 ) ;
#43921 = ORIENTED_EDGE ( 'NONE', *, *, #39498, .T. ) ;
#43922 = VECTOR ( 'NONE', #18733, 1000.000000000000227 ) ;
#43923 = DIRECTION ( 'NONE',  ( 1.132880637372608740E-16, 4.718402560806925739E-50, 1.000000000000000000 ) ) ;
#43924 = DIRECTION ( 'NONE',  ( 0.000000000000000000, -1.000000000000000000, 0.000000000000000000 ) ) ;
#43925 = DIRECTION ( 'NONE',  ( 3.172065745548403743E-16, 1.000000000000000000, 0.000000000000000000 ) ) ;
#43926 = VECTOR ( 'NONE', #13765, 1000.000000000000000 ) ;
#43927 = VERTEX_POINT ( 'NONE', #25973 ) ;
#43928 = B_SPLINE_CURVE_WITH_KNOTS ( 'NONE', 3,
 ( #13373, #5672, #14119, #20819 ),
 .UNSPECIFIED., .F., .F.,
 ( 4, 4 ),
 ( 1.788112030672749005E-18, 0.009404495247862344059 ),
 .UNSPECIFIED. ) ;
#43929 = CARTESIAN_POINT ( 'NONE',  ( 210.0000000000000568, 0.000000000000000000, 40.81828755692798438 ) ) ;
#43930 = DIRECTION ( 'NONE',  ( -0.000000000000000000, -0.000000000000000000, -1.000000000000000000 ) ) ;
#43931 = EDGE_CURVE ( 'NONE', #27906, #47424, #33920, .T. ) ;
#43932 = CARTESIAN_POINT ( 'NONE',  ( 339.9999999999998863, -168.9999999999999432, 341.9999999999997726 ) ) ;
#43934 = VECTOR ( 'NONE', #28422, 1000.000000000000000 ) ;
#43933 = DIRECTION ( 'NONE',  ( -2.874857526315639190E-31, 1.000000000000000000, -2.537652627714642000E-15 ) ) ;
#43935 = EDGE_LOOP ( 'NONE', ( #6182, #31062, #31918, #10091 ) ) ;
#43936 = EDGE_LOOP ( 'NONE', ( #10562, #39480, #4535, #27913 ) ) ;
#43937 = MECHANICAL_DESIGN_GEOMETRIC_PRESENTATION_REPRESENTATION (  '', ( #6273 ), #26740 ) ;
#43938 = ORIENTED_EDGE ( 'NONE', *, *, #17337, .F. ) ;
#43939 = CARTESIAN_POINT ( 'NONE',  ( 4.531159320492035292, 41.49457383023836599, -8.080361901872242569 ) ) ;
#43940 = CARTESIAN_POINT ( 'NONE',  ( 115.0540265531850395, -1.025126265847081664, -117.4317124430720440 ) ) ;
#43941 = CARTESIAN_POINT ( 'NONE',  ( 350.0000000000000000, -164.9999999999999432, -340.0000000000001705 ) ) ;
#43942 = ORIENTED_EDGE ( 'NONE', *, *, #40094, .F. ) ;
#43943 = CARTESIAN_POINT ( 'NONE',  ( 113.3040265531850537, 1.749999999999996891, 160.8182875569279702 ) ) ;
#43944 = VERTEX_POINT ( 'NONE', #14916 ) ;
#43945 = VECTOR ( 'NONE', #22338, 1000.000000000000000 ) ;
#43946 = DIRECTION ( 'NONE',  ( -0.000000000000000000, -0.000000000000000000, -1.000000000000000000 ) ) ;
#43947 = VERTEX_POINT ( 'NONE', #49760 ) ;
#43948 = DIRECTION ( 'NONE',  ( 0.000000000000000000, 0.000000000000000000, -1.000000000000000000 ) ) ;
#43949 = PLANE ( 'NONE',  #3895 ) ;
#43950 = LINE ( 'NONE', #17268, #32413 ) ;
#43951 = DIRECTION ( 'NONE',  ( -0.000000000000000000, -1.000000000000000000, -0.000000000000000000 ) ) ;
#43952 = CARTESIAN_POINT ( 'NONE',  ( -7.608425291889091113, 36.72004717559254772, 7.697694107796188234 ) ) ;
#43953 = CARTESIAN_POINT ( 'NONE',  ( 85.00000000000184741, 16.00000000000000000, 65.00000000000000000 ) ) ;
#43954 = VERTEX_POINT ( 'NONE', #15171 ) ;
#43955 = DIRECTION ( 'NONE',  ( 4.625929269271687073E-16, -0.000000000000000000, 1.000000000000000000 ) ) ;
#43956 = CARTESIAN_POINT ( 'NONE',  ( 80.00000000000061107, 16.00000000000000000, -30.00000000000000000 ) ) ;
#43957 = CARTESIAN_POINT ( 'NONE',  ( -84.94597344681494633, 2.143131898507880377E-16, 42.56828755692798438 ) ) ;
#43958 = CARTESIAN_POINT ( 'NONE',  ( 164.9999999999999716, -9.999999999999953815, -111.0000000000001563 ) ) ;
#43960 = VERTEX_POINT ( 'NONE', #42605 ) ;
#43959 = VECTOR ( 'NONE', #41726, 1000.000000000000000 ) ;
#43961 = DIRECTION ( 'NONE',  ( 1.000000000000000000, 0.000000000000000000, 0.000000000000000000 ) ) ;
#43962 = VERTEX_POINT ( 'NONE', #22108 ) ;
#43963 = EDGE_CURVE ( 'NONE', #31470, #49119, #30573, .T. ) ;
#43964 = LINE ( 'NONE', #20631, #44348 ) ;
#43965 = EDGE_LOOP ( 'NONE', ( #3232, #11379, #5175, #41863 ) ) ;
#43966 = DIRECTION ( 'NONE',  ( 1.000000000000000000, 0.000000000000000000, 0.000000000000000000 ) ) ;
#43967 = CARTESIAN_POINT ( 'NONE',  ( 355.9999999999999432, -183.0000000000001137, -358.0000000000003411 ) ) ;
#43968 = CARTESIAN_POINT ( 'NONE',  ( -0.3862712429686895876, 1.188820645368940720, 10.00000000000000000 ) ) ;
#43969 = CARTESIAN_POINT ( 'NONE',  ( 16.52264463346132572, -2.779753662172757878, 9.403735324607438884 ) ) ;
#43970 = EDGE_CURVE ( 'NONE', #7277, #46718, #38788, .T. ) ;
#43971 = ORIENTED_EDGE ( 'NONE', *, *, #43704, .T. ) ;
#43972 = VERTEX_POINT ( 'NONE', #26462 ) ;
#43973 = DIRECTION ( 'NONE',  ( 0.000000000000000000, 0.000000000000000000, 1.000000000000000000 ) ) ;
#43974 = VECTOR ( 'NONE', #36960, 1000.000000000000000 ) ;
#43975 = CARTESIAN_POINT ( 'NONE',  ( 33.43156050989131955, -4.370686678976570150, 8.807470649214879543 ) ) ;
#43976 = EDGE_CURVE ( 'NONE', #16962, #50249, #6286, .T. ) ;
#43977 = ORIENTED_EDGE ( 'NONE', *, *, #19975, .T. ) ;
#43978 = ORIENTED_EDGE ( 'NONE', *, *, #24902, .T. ) ;
#43979 = DIRECTION ( 'NONE',  ( -1.586032892321652236E-16, -1.000000000000000000, -0.000000000000000000 ) ) ;
#43980 = FACE_OUTER_BOUND ( 'NONE', #5151, .T. ) ;
#43981 = CARTESIAN_POINT ( 'NONE',  ( -124.9459734468149463, 2.143131898507847836E-16, 165.0000000000000000 ) ) ;
#43982 = CYLINDRICAL_SURFACE ( 'NONE', #14937, 1.750000000000010214 ) ;
#43983 = ORIENTED_EDGE ( 'NONE', *, *, #6186, .F. ) ;
#43984 = ORIENTED_EDGE ( 'NONE', *, *, #42266, .T. ) ;
#43985 = ORIENTED_EDGE ( 'NONE', *, *, #15969, .F. ) ;
#43986 = EDGE_CURVE ( 'NONE', #13983, #26888, #41693, .T. ) ;
#43987 = EDGE_CURVE ( 'NONE', #38451, #50334, #30928, .T. ) ;
#43988 = CARTESIAN_POINT ( 'NONE',  ( -165.3973046169136012, 54.43801056904003133, -94.69675437945474528 ) ) ;
#43989 = EDGE_CURVE ( 'NONE', #18739, #7906, #2624, .T. ) ;
#43990 = EDGE_CURVE ( 'NONE', #36961, #26037, #49661, .T. ) ;
#43991 = AXIS2_PLACEMENT_3D ( 'NONE', #24838, #20468, #1493 ) ;
#43992 = CARTESIAN_POINT ( 'NONE',  ( -8.843309649387274263, 14.11631751497152720, -2.870787844569587133 ) ) ;
#43993 = ORIENTED_EDGE ( 'NONE', *, *, #6089, .T. ) ;
#43994 = ORIENTED_EDGE ( 'NONE', *, *, #46886, .F. ) ;
#43995 = CARTESIAN_POINT ( 'NONE',  ( -1.250000000000000222, 0.000000000000000000, 3.333333333333333481 ) ) ;
#43996 =( BOUNDED_CURVE ( )  B_SPLINE_CURVE ( 3, ( #5463, #44196, #29073, #24222 ),
 .UNSPECIFIED., .F., .F. ) 
 B_SPLINE_CURVE_WITH_KNOTS ( ( 4, 4 ),
 ( 4.712388980384689674, 6.283185307179586232 ),
 .UNSPECIFIED. ) 
 CURVE ( )  GEOMETRIC_REPRESENTATION_ITEM ( )  RATIONAL_B_SPLINE_CURVE ( ( 1.000000000000000000, 0.8047378541243649375, 0.8047378541243649375, 1.000000000000000000 ) ) 
 REPRESENTATION_ITEM ( '' )  );
#43997 = CARTESIAN_POINT ( 'NONE',  ( -86.69597344681496054, 0.000000000000000000, 165.0000000000000000 ) ) ;
#43998 = ORIENTED_EDGE ( 'NONE', *, *, #19919, .T. ) ;
#43999 = ORIENTED_EDGE ( 'NONE', *, *, #28778, .F. ) ;
#44000 = CARTESIAN_POINT ( 'NONE',  ( 358.0000000000001137, 178.0000000000000284, 352.9999999999998295 ) ) ;
#44001 = EDGE_LOOP ( 'NONE', ( #6680, #38045, #25743, #1794 ) ) ;
#44002 = CARTESIAN_POINT ( 'NONE',  ( 73.30402655318508209, 0.000000000000000000, 165.0000000000000000 ) ) ;
#44003 = CARTESIAN_POINT ( 'NONE',  ( 344.0000000000000000, -174.9999999999999432, 339.9999999999998295 ) ) ;
#44004 = LINE ( 'NONE', #5271, #41797 ) ;
#44005 = DIRECTION ( 'NONE',  ( -0.000000000000000000, -0.000000000000000000, -1.000000000000000000 ) ) ;
#44006 = ORIENTED_EDGE ( 'NONE', *, *, #30342, .F. ) ;
#44007 = DIRECTION ( 'NONE',  ( 0.000000000000000000, -1.000000000000000000, 0.000000000000000000 ) ) ;
#44008 = DIRECTION ( 'NONE',  ( 0.000000000000000000, 0.000000000000000000, 1.000000000000000000 ) ) ;
#44009 = B_SPLINE_SURFACE_WITH_KNOTS ( 'NONE', 3, 3, ( 
 ( #9919, #40220, #25578, #9165 ),
 ( #21717, #37405, #28426, #24571 ),
 ( #5055, #16877, #24826, #20715 ),
 ( #36392, #5315, #1235, #32539 ) ),
 .UNSPECIFIED., .F., .F., .F.,
 ( 4, 4 ),
 ( 4, 4 ),
 ( 0.000000000000000000, 1.000000000000000000 ),
 ( 0.000000000000000000, 1.000000000000000000 ),
 .UNSPECIFIED. ) ;
#44010 = CARTESIAN_POINT ( 'NONE',  ( -18.69789054174323084, 27.49790346457746182, -2.408242355805840784 ) ) ;
#44011 = EDGE_CURVE ( 'NONE', #7115, #40366, #23107, .T. ) ;
#44012 = LINE ( 'NONE', #19914, #45947 ) ;
#44013 = EDGE_CURVE ( 'NONE', #20947, #23039, #16438, .T. ) ;
#44014 = EDGE_CURVE ( 'NONE', #8314, #16057, #1401, .T. ) ;
#44015 = CARTESIAN_POINT ( 'NONE',  ( 350.0000000000000000, -168.9999999999999432, -358.0000000000002274 ) ) ;
#44016 = ADVANCED_FACE ( 'NONE', ( #790 ), #15673, .F. ) ;
#44017 = PLANE ( 'NONE',  #33230 ) ;
#44018 = LINE ( 'NONE', #21432, #916 ) ;
#44019 = EDGE_CURVE ( 'NONE', #21569, #1107, #8496, .T. ) ;
#44020 = ORIENTED_EDGE ( 'NONE', *, *, #26859, .T. ) ;
#44021 = AXIS2_PLACEMENT_3D ( 'NONE', #43507, #4517, #670 ) ;
#44022 = CARTESIAN_POINT ( 'NONE',  ( 210.0000000000000568, 0.000000000000000000, 80.81828755692798438 ) ) ;
#44023 = VERTEX_POINT ( 'NONE', #12087 ) ;
#44024 = LINE ( 'NONE', #17094, #2443 ) ;
#44025 = CARTESIAN_POINT ( 'NONE',  ( 25.04522487443081502, -22.77512090857307925, 8.356839323120299312 ) ) ;
#44026 = CARTESIAN_POINT ( 'NONE',  ( 31.55402655318503236, -1.025126265847089435, 2.568287556927986159 ) ) ;
#44027 = ORIENTED_EDGE ( 'NONE', *, *, #37207, .T. ) ;
#44028 = CARTESIAN_POINT ( 'NONE',  ( 210.0000000000000568, 0.000000000000000000, 120.8182875569279702 ) ) ;
#44029 = ORIENTED_EDGE ( 'NONE', *, *, #8273, .F. ) ;
#44030 = VERTEX_POINT ( 'NONE', #16679 ) ;
#44031 = CARTESIAN_POINT ( 'NONE',  ( 1.275927284277173834, -0.1224368140627448004, 9.976582533991679824 ) ) ;
#44032 = LINE ( 'NONE', #12241, #27927 ) ;
#44033 = ORIENTED_EDGE ( 'NONE', *, *, #36688, .F. ) ;
#44034 = CARTESIAN_POINT ( 'NONE',  ( 32.27890028733795447, 1.750000000000010436, 79.79316129108087807 ) ) ;
#44035 = DIRECTION ( 'NONE',  ( 0.000000000000000000, 1.000000000000000000, -2.537652627714643577E-15 ) ) ;
#44036 = ADVANCED_FACE ( 'NONE', ( #4643 ), #3871, .F. ) ;
#44037 = ORIENTED_EDGE ( 'NONE', *, *, #16194, .T. ) ;
#44038 = ORIENTED_EDGE ( 'NONE', *, *, #37137, .T. ) ;
#44039 = DIRECTION ( 'NONE',  ( 1.156482317317870492E-16, -1.000000000000000000, -0.000000000000000000 ) ) ;
#44040 = ADVANCED_FACE ( 'NONE', ( #42859 ), #27485, .T. ) ;
#44041 = ORIENTED_EDGE ( 'NONE', *, *, #48428, .T. ) ;
#44042 = B_SPLINE_CURVE_WITH_KNOTS ( 'NONE', 3,
 ( #9283, #2332, #25436, #9527 ),
 .UNSPECIFIED., .F., .F.,
 ( 4, 4 ),
 ( 1.119743386075808773E-15, 0.0004154657329505087246 ),
 .UNSPECIFIED. ) ;
#44043 = CARTESIAN_POINT ( 'NONE',  ( 0.6440276692615888310, 16.64212148744554298, -9.683996418299976483 ) ) ;
#44044 = DIRECTION ( 'NONE',  ( -4.758098676964957447E-16, -1.000000000000000000, 7.143884938411937192E-48 ) ) ;
#44045 = LINE ( 'NONE', #8912, #9508 ) ;
#44046 = EDGE_CURVE ( 'NONE', #21569, #47711, #43878, .T. ) ;
#44047 = EDGE_LOOP ( 'NONE', ( #50673, #32540, #22112, #29562 ) ) ;
#44048 = EDGE_CURVE ( 'NONE', #45429, #45821, #36164, .T. ) ;
#44049 = LINE ( 'NONE', #44796, #48026 ) ;
#44050 = CARTESIAN_POINT ( 'NONE',  ( 350.0000000000001137, 181.0000000000000284, 339.9999999999997726 ) ) ;
#44051 = ORIENTED_EDGE ( 'NONE', *, *, #41129, .T. ) ;
#44052 = ORIENTED_EDGE ( 'NONE', *, *, #8107, .F. ) ;
#44053 = ORIENTED_EDGE ( 'NONE', *, *, #48069, .T. ) ;
#44054 = LINE ( 'NONE', #44538, #13954 ) ;
#44055 = EDGE_CURVE ( 'NONE', #34812, #34800, #23627, .T. ) ;
#44056 = ADVANCED_FACE ( 'NONE', ( #8749 ), #39289, .T. ) ;
#44057 = CARTESIAN_POINT ( 'NONE',  ( -1.780432407520014415, -1.041450996408466612, 9.894754715216725671 ) ) ;
#44058 = ORIENTED_EDGE ( 'NONE', *, *, #13318, .T. ) ;
#44059 = CARTESIAN_POINT ( 'NONE',  ( 33.30402655318503946, 1.750000000000010658, -79.18171244307201562 ) ) ;
#44060 = DIRECTION ( 'NONE',  ( 0.000000000000000000, -2.537652627714643577E-15, -1.000000000000000000 ) ) ;
#44061 = CARTESIAN_POINT ( 'NONE',  ( 210.0000000000000568, 0.000000000000000000, 120.8182875569279702 ) ) ;
#44062 = CARTESIAN_POINT ( 'NONE',  ( -556.8973046169135159, 54.43801056904003133, -64.63743994998280584 ) ) ;
#44063 = CARTESIAN_POINT ( 'NONE',  ( 210.0000000000000568, 0.000000000000000000, -79.18171244307201562 ) ) ;
#44064 = AXIS2_PLACEMENT_3D ( 'NONE', #19416, #31744, #34835 ) ;
#44065 = CARTESIAN_POINT ( 'NONE',  ( 113.3040265531850537, -1.749999999999997335, -119.1817124430720440 ) ) ;
#44066 = CARTESIAN_POINT ( 'NONE',  ( -204.9459734468148895, -1.025126265847089657, -80.93171244307201562 ) ) ;
#44067 = FACE_OUTER_BOUND ( 'NONE', #49571, .T. ) ;
#44068 = CYLINDRICAL_SURFACE ( 'NONE', #6773, 1.750000000000015543 ) ;
#44069 = CARTESIAN_POINT ( 'NONE',  ( -124.9459734468149463, 2.143131898507847836E-16, 119.0682875569279844 ) ) ;
#44070 = LINE ( 'NONE', #6095, #25507 ) ;
#44071 = UNCERTAINTY_MEASURE_WITH_UNIT (LENGTH_MEASURE( 1.000000000000000082E-05 ), #19723, 'distance_accuracy_value', 'NONE');
#44072 = EDGE_CURVE ( 'NONE', #39708, #24104, #6624, .T. ) ;
#44073 =( BOUNDED_CURVE ( )  B_SPLINE_CURVE ( 3, ( #2222, #24565, #25316, #37146 ),
 .UNSPECIFIED., .F., .F. ) 
 B_SPLINE_CURVE_WITH_KNOTS ( ( 4, 4 ),
 ( 1.570796326794896558, 3.141592653589793116 ),
 .UNSPECIFIED. ) 
 CURVE ( )  GEOMETRIC_REPRESENTATION_ITEM ( )  RATIONAL_B_SPLINE_CURVE ( ( 1.000000000000000000, 0.8047378541243649375, 0.8047378541243649375, 1.000000000000000000 ) ) 
 REPRESENTATION_ITEM ( '' )  );
#44074 = DIRECTION ( 'NONE',  ( 0.000000000000000000, 2.537652627714642000E-15, 1.000000000000000000 ) ) ;
#44075 = ORIENTED_EDGE ( 'NONE', *, *, #11868, .F. ) ;
#44076 = CARTESIAN_POINT ( 'NONE',  ( 181.0000000000000284, -168.9999999999999432, -115.0000000000001847 ) ) ;
#44077 = FACE_OUTER_BOUND ( 'NONE', #4004, .T. ) ;
#44078 = LINE ( 'NONE', #24602, #2078 ) ;
#44079 = PRODUCT_RELATED_PRODUCT_CATEGORY ( 'part', '', ( #33111 ) ) ;
#44080 = CARTESIAN_POINT ( 'NONE',  ( 167.0000000000000000, -174.9999999999999716, -99.00000000000014211 ) ) ;
#44081 = ORIENTED_EDGE ( 'NONE', *, *, #49343, .F. ) ;
#44082 = FACE_OUTER_BOUND ( 'NONE', #38565, .T. ) ;
#44083 = ORIENTED_EDGE ( 'NONE', *, *, #49413, .T. ) ;
#44084 = CARTESIAN_POINT ( 'NONE',  ( 16.16402646813543242, -4.033894069732437693, -3.546734833711462365 ) ) ;
#44086 = ADVANCED_FACE ( 'NONE', ( #20535 ), #23884, .F. ) ;
#44085 = DIRECTION ( 'NONE',  ( -1.000000000000000000, 0.000000000000000000, -7.793956916774525800E-48 ) ) ;
#44087 = DIRECTION ( 'NONE',  ( 0.000000000000000000, 0.000000000000000000, 1.000000000000000000 ) ) ;
#44088 = EDGE_LOOP ( 'NONE', ( #23194, #36835, #18605, #3010 ) ) ;
#44089 = DIRECTION ( 'NONE',  ( -0.000000000000000000, -0.000000000000000000, -1.000000000000000000 ) ) ;
#44090 = VERTEX_POINT ( 'NONE', #21289 ) ;
#44091 = ORIENTED_EDGE ( 'NONE', *, *, #39802, .F. ) ;
#44092 = AXIS2_PLACEMENT_3D ( 'NONE', #44940, #44698, #40870 ) ;
#44093 = ORIENTED_EDGE ( 'NONE', *, *, #32738, .T. ) ;
#44094 = CARTESIAN_POINT ( 'NONE',  ( -206.6959734468149463, 0.000000000000000000, 165.0000000000000000 ) ) ;
#44095 = EDGE_CURVE ( 'NONE', #3325, #8469, #37820, .T. ) ;
#44096 = ORIENTED_EDGE ( 'NONE', *, *, #6413, .F. ) ;
#44097 = LINE ( 'NONE', #28225, #6576 ) ;
#44098 = LINE ( 'NONE', #33091, #48797 ) ;
#44099 = CYLINDRICAL_SURFACE ( 'NONE', #33809, 2.000000000000001776 ) ;
#44100 = DIRECTION ( 'NONE',  ( 1.000000000000000000, -0.000000000000000000, -0.000000000000000000 ) ) ;
#44101 = ORIENTED_EDGE ( 'NONE', *, *, #19397, .F. ) ;
#44102 = DIRECTION ( 'NONE',  ( 0.000000000000000000, 0.000000000000000000, 1.000000000000000000 ) ) ;
#44103 = ADVANCED_FACE ( 'NONE', ( #41295 ), #44119, .T. ) ;
#44104 = VERTEX_POINT ( 'NONE', #24650 ) ;
#44105 = EDGE_CURVE ( 'NONE', #15550, #42730, #25151, .T. ) ;
#44106 = DIRECTION ( 'NONE',  ( 0.000000000000000000, 0.9230769230769231282, 0.3846153846153844702 ) ) ;
#44107 = FACE_OUTER_BOUND ( 'NONE', #35542, .T. ) ;
#44108 = ORIENTED_EDGE ( 'NONE', *, *, #28149, .T. ) ;
#44109 = LINE ( 'NONE', #21281, #5725 ) ;
#44110 = EDGE_CURVE ( 'NONE', #21871, #13960, #44861, .T. ) ;
#44111 = DIRECTION ( 'NONE',  ( 0.000000000000000000, -1.000000000000000000, 5.664403186863042467E-17 ) ) ;
#44112 = B_SPLINE_SURFACE_WITH_KNOTS ( 'NONE', 3, 3, ( 
 ( #33790, #49379, #14265, #29931 ),
 ( #45546, #19889, #11440, #157 ),
 ( #31207, #19642, #20842, #24706 ),
 ( #4254, #19124, #7862, #40353 ) ),
 .UNSPECIFIED., .F., .F., .F.,
 ( 4, 4 ),
 ( 4, 4 ),
 ( 0.000000000000000000, 1.000000000000000000 ),
 ( 0.000000000000000000, 1.000000000000000000 ),
 .UNSPECIFIED. ) ;
#44113 = ORIENTED_EDGE ( 'NONE', *, *, #3765, .T. ) ;
#44114 = DIRECTION ( 'NONE',  ( -1.586032880504786307E-16, 1.654361225106055350E-24, -1.000000000000000000 ) ) ;
#44115 = ADVANCED_FACE ( 'NONE', ( #25397 ), #13820, .T. ) ;
#44116 = CARTESIAN_POINT ( 'NONE',  ( 0.7142790906314127053, -1.400791805248631672, 9.945241992664893615 ) ) ;
#44117 = CARTESIAN_POINT ( 'NONE',  ( 151.5540265531850537, 1.025126265847088991, -157.4317124430720582 ) ) ;
#44118 = EDGE_CURVE ( 'NONE', #214, #38516, #29256, .T. ) ;
#44119 = PLANE ( 'NONE',  #6699 ) ;
#44120 = ORIENTED_EDGE ( 'NONE', *, *, #43154, .T. ) ;
#44121 = CARTESIAN_POINT ( 'NONE',  ( -5.670847180967843570, 1.750000000000023315, -40.20683870891912903 ) ) ;
#44122 = DIRECTION ( 'NONE',  ( 0.6904757466825005574, -0.7233555441435722821, 0.000000000000000000 ) ) ;
#44123 = EDGE_CURVE ( 'NONE', #7917, #6960, #9237, .T. ) ;
#44124 = CARTESIAN_POINT ( 'NONE',  ( -0.3370904143228943828, -0.2449105217885308716, 10.00000000000000000 ) ) ;
#44125 = ORIENTED_EDGE ( 'NONE', *, *, #10927, .F. ) ;
#44126 = ORIENTED_EDGE ( 'NONE', *, *, #6890, .F. ) ;
#44127 = SHAPE_DEFINITION_REPRESENTATION ( #30252, #50327 ) ;
#44128 = AXIS2_PLACEMENT_3D ( 'NONE', #1933, #21416, #13471 ) ;
#44129 = CARTESIAN_POINT ( 'NONE',  ( 355.9999999999998863, -165.0000000000001137, -90.00000000000018474 ) ) ;
#44130 =( BOUNDED_CURVE ( )  B_SPLINE_CURVE ( 3, ( #5285, #47593, #9137, #40448 ),
 .UNSPECIFIED., .F., .F. ) 
 B_SPLINE_CURVE_WITH_KNOTS ( ( 4, 4 ),
 ( 4.712388980384689674, 6.283185307179586232 ),
 .UNSPECIFIED. ) 
 CURVE ( )  GEOMETRIC_REPRESENTATION_ITEM ( )  RATIONAL_B_SPLINE_CURVE ( ( 1.000000000000000000, 0.8047378541243649375, 0.8047378541243649375, 1.000000000000000000 ) ) 
 REPRESENTATION_ITEM ( '' )  );
#44131 = DIRECTION ( 'NONE',  ( 0.000000000000000000, 0.000000000000000000, -1.000000000000000000 ) ) ;
#44132 = VECTOR ( 'NONE', #42064, 1000.000000000000000 ) ;
#44133 = CARTESIAN_POINT ( 'NONE',  ( -27.33593271309441519, 41.94268121623345991, -9.367992836599954742 ) ) ;
#44134 = CARTESIAN_POINT ( 'NONE',  ( -128.4459734468149463, -1.025126265847082108, 82.56828755692798438 ) ) ;
#44135 = CARTESIAN_POINT ( 'NONE',  ( -30.21887974406478250, 14.69854701517550666, -8.016098858316199838 ) ) ;
#44136 = ORIENTED_EDGE ( 'NONE', *, *, #47320, .F. ) ;
#44137 = LINE ( 'NONE', #27996, #23076 ) ;
#44138 =( BOUNDED_CURVE ( )  B_SPLINE_CURVE ( 3, ( #25936, #17465, #33140, #49223 ),
 .UNSPECIFIED., .F., .F. ) 
 B_SPLINE_CURVE_WITH_KNOTS ( ( 4, 4 ),
 ( 1.570796326794889675, 3.141592653589793116 ),
 .UNSPECIFIED. ) 
 CURVE ( )  GEOMETRIC_REPRESENTATION_ITEM ( )  RATIONAL_B_SPLINE_CURVE ( ( 1.000000000000000000, 0.8047378541243634942, 0.8047378541243634942, 1.000000000000000000 ) ) 
 REPRESENTATION_ITEM ( '' )  );
#44139 = CARTESIAN_POINT ( 'NONE',  ( 358.3431457505076310, -165.0000000000001137, -340.0000000000003979 ) ) ;
#44140 = CARTESIAN_POINT ( 'NONE',  ( -86.69597344681494633, 1.750000000000010658, 80.81828755692798438 ) ) ;
#44141 = CLOSED_SHELL ( 'NONE', ( #13547, #38395, #43477, #14569, #2413, #33993, #18896, #8537, #45560, #49789, #31065, #5764, #3401, #48213, #9887, #24613, #48966, #18612, #40282, #40726, #48728, #48698, #7394, #9388, #23439, #32513, #45952, #30027, #27230, #47226, #27119, #37554, #5739, #45556, #48759, #37603, #10645, #49963, #7317, #12495, #23934, #22417, #48486, #38747, #35352, #28717, #7352, #14854, #12699, #21311, #31576, #48444, #8341, #21060, #48639, #27618, #37558, #2688, #45213, #7246, #45568, #28942, #50137, #18962, #13950, #1798, #3273, #19401, #30403, #24445, #48725, #39757, #26427, #26860, #29301, #7784, #40940, #11739, #22707, #18453, #31862, #31231, #30445, #21002, #5735, #27499, #38159, #15355, #31360, #7825, #194, #44922, #44040, #20035, #23086, #29324, #43425, #19039, #39635, #26004, #26717, #45521, #20853, #16255, #2148, #34609, #20791, #17215, #12662, #25594, #45922, #27075, #37828, #32473, #20250, #49947, #1125, #36942, #33484, #2939, #7365, #24603, #15479, #8216, #39888, #32275, #11229, #18464, #32414, #42425, #37895, #16847, #2293, #4286, #12696, #50623, #10140, #13000, #3294, #10146, #34016, #7724, #12124, #47574, #29746, #46010, #1786, #40594, #15920, #34770, #32140, #14320, #30579, #38603, #40225, #20475, #37735, #452, #2317, #49591, #22668, #43266, #13298, #25654, #39179, #30195, #604, #15573, #37959, #26568, #143, #5178, #18499, #29315, #7964, #2353, #2699, #28038, #21856, #12994, #34129, #10086, #1994, #8760, #36198, #47281, #27266, #20502, #2003, #2892, #45871, #39972, #43213, #36230, #42766, #27446, #34101, #3564, #37277, #47635, #7774, #25123, #37969, #45411, #26442, #14829, #19545, #45367, #6671, #48925, #49414, #43203, #4221, #25929, #30544, #40723, #34673, #9962, #21900, #15178, #7827, #15866, #35050, #41348, #13770, #49302, #13363, #653, #39044, #232, #34301, #45247, #36567, #33341, #18586, #23976, #39720, #30079, #7762, #19575, #5780, #38716, #35601, #22006, #815, #12751, #1996, #47175, #9591, #703, #11390, #25065, #23386, #26115, #33420, #5201, #4975, #49702, #14930, #36174, #10018, #8456, #49266, #21487, #43770, #38674, #18409, #46708, #31837, #3710, #45074, #34011, #38887, #45753, #37557, #19781, #28072, #38253, #4531, #24876, #41498, #18395, #9257, #44387, #3260, #9246, #32570, #23709, #11453, #5593, #182, #25550, #2983, #48105, #27784, #20965, #3289, #36496, #801, #22452, #22044, #10941, #3593, #25099, #32312, #6891, #49064, #9173, #47905, #27352, #12374, #34017, #16500, #40670, #47205, #9278, #13747, #31992, #3328, #45672, #38685, #33218, #48970, #526, #43740, #29363, #5592, #25656, #40556, #12628, #8328, #47, #38824, #581, #41990, #18496, #23047, #19229, #35990, #44103, #47213, #23639, #39967, #4967, #41510, #44678, #23066, #44399, #31137, #39016, #45900, #20571, #18920, #30581, #41504, #20177, #14209, #26167, #24607, #27201, #11304, #14355, #47752, #35412, #19876, #13419, #19837, #36917, #14642, #31153, #46253, #40997, #17949, #35646, #944, #45875, #37958, #12967, #30997, #29261, #12965, #32544, #15570, #42022, #38736, #2940, #9758, #46807, #28446, #48236, #20594, #26426, #47441, #46866, #29613, #18902, #48788, #43846, #10484, #30717, #22478, #8297, #15524, #27238, #7120, #34134, #24610, #11951, #23342, #22522, #29346, #15152, #36848, #19263, #3948, #41341, #40418, #22397, #5475, #16541, #29579, #45505, #31651, #16624, #48831, #23949, #8883, #24007, #2013, #2440, #46734, #6814, #23460, #15220, #10541, #22457, #42767, #39355, #41045, #41209, #30929, #25674, #50315, #24894, #34271, #49898, #45896, #44180, #10252, #39017, #19411, #38394, #28085, #49339, #45314, #45432, #21178, #13760, #21119, #23156, #8669, #48148, #6165, #29998, #37175, #10774, #29364, #15531, #13067, #8153, #40373, #13206, #44568, #39521, #40034, #28975 ) ) ;
#44142 = FACE_OUTER_BOUND ( 'NONE', #41423, .T. ) ;
#44143 = ORIENTED_EDGE ( 'NONE', *, *, #10266, .F. ) ;
#44144 = DIRECTION ( 'NONE',  ( 0.000000000000000000, 0.2223603367690619725, -0.9749645535258958384 ) ) ;
#44145 = ORIENTED_EDGE ( 'NONE', *, *, #38656, .T. ) ;
#44146 = FACE_OUTER_BOUND ( 'NONE', #26634, .T. ) ;
#44147 = EDGE_LOOP ( 'NONE', ( #26793, #30003, #13542, #20722 ) ) ;
#44148 = CARTESIAN_POINT ( 'NONE',  ( 185.0000000000000284, -174.9999999999999716, -111.0000000000001563 ) ) ;
#44149 = CARTESIAN_POINT ( 'NONE',  ( -205.6708471809678827, 1.750000000000010214, -120.2068387089191219 ) ) ;
#44150 = CYLINDRICAL_SURFACE ( 'NONE', #22411, 1.750000000000015543 ) ;
#44151 = FACE_OUTER_BOUND ( 'NONE', #46419, .T. ) ;
#44152 = ORIENTED_EDGE ( 'NONE', *, *, #46638, .F. ) ;
#44153 = EDGE_CURVE ( 'NONE', #49290, #19115, #17280, .T. ) ;
#44154 = CARTESIAN_POINT ( 'NONE',  ( -6.695973446814940111, 1.750000000000024203, -79.18171244307201562 ) ) ;
#44155 = EDGE_LOOP ( 'NONE', ( #48058, #41982, #38285, #24905, #5415 ) ) ;
#44156 = DIRECTION ( 'NONE',  ( 0.000000000000000000, -1.000000000000000000, 0.000000000000000000 ) ) ;
#44157 = CARTESIAN_POINT ( 'NONE',  ( 42.99990394833793061, 47.95759300784327905, 5.000000000000000000 ) ) ;
#44158 = B_SPLINE_CURVE_WITH_KNOTS ( 'NONE', 3,
 ( #22862, #31608, #42101, #7996 ),
 .UNSPECIFIED., .F., .F.,
 ( 4, 4 ),
 ( 0.001152428489661398280, 0.001623376834729528930 ),
 .UNSPECIFIED. ) ;
#44159 = LINE ( 'NONE', #4917, #40974 ) ;
#44160 = CARTESIAN_POINT ( 'NONE',  ( -115.0000000000000284, 17.00000000000000000, -90.00000000000000000 ) ) ;
#44161 = ORIENTED_EDGE ( 'NONE', *, *, #43545, .T. ) ;
#44162 = EDGE_LOOP ( 'NONE', ( #5472, #27561, #11364, #4781, #46687, #13055 ) ) ;
#44163 = DIRECTION ( 'NONE',  ( -1.000000000000000000, -0.000000000000000000, -0.000000000000000000 ) ) ;
#44164 = VECTOR ( 'NONE', #24794, 1000.000000000000000 ) ;
#44165 = EDGE_CURVE ( 'NONE', #46611, #1904, #24896, .T. ) ;
#44166 = AXIS2_PLACEMENT_3D ( 'NONE', #42625, #50538, #35215 ) ;
#44167 = ORIENTED_EDGE ( 'NONE', *, *, #48154, .T. ) ;
#44168 = ADVANCED_FACE ( 'NONE', ( #28989 ), #36977, .T. ) ;
#44169 = CARTESIAN_POINT ( 'NONE',  ( 356.0000000000000000, -167.0000000000001137, 341.9999999999999432 ) ) ;
#44170 = CARTESIAN_POINT ( 'NONE',  ( 193.3040265531851105, -1.750000000000010214, 40.81828755692798438 ) ) ;
#44171 = CARTESIAN_POINT ( 'NONE',  ( 33.30402655318503946, -1.750000000000010658, -119.1817124430720440 ) ) ;
#44172 = ORIENTED_EDGE ( 'NONE', *, *, #19605, .T. ) ;
#44173 = CARTESIAN_POINT ( 'NONE',  ( -128.4459734468149463, 1.025126265847081886, -120.9317124430720440 ) ) ;
#44174 = VECTOR ( 'NONE', #27476, 1000.000000000000000 ) ;
#44175 = LINE ( 'NONE', #12883, #2161 ) ;
#44176 = CARTESIAN_POINT ( 'NONE',  ( 358.0000000000001137, 169.0000000000000000, 343.9999999999998863 ) ) ;
#44177 = CARTESIAN_POINT ( 'NONE',  ( 210.0000000000000568, 0.000000000000000000, -77.43171244307200141 ) ) ;
#44178 = EDGE_CURVE ( 'NONE', #14334, #907, #41048, .T. ) ;
#44179 = FACE_OUTER_BOUND ( 'NONE', #32152, .T. ) ;
#44180 = ADVANCED_FACE ( 'NONE', ( #17695 ), #33360, .T. ) ;
#44181 = CARTESIAN_POINT ( 'NONE',  ( 358.0000000000000000, -174.9999999999999432, 343.9999999999998295 ) ) ;
#44182 = ORIENTED_EDGE ( 'NONE', *, *, #17336, .F. ) ;
#44183 = VERTEX_POINT ( 'NONE', #34366 ) ;
#44184 = ORIENTED_EDGE ( 'NONE', *, *, #43004, .F. ) ;
#44185 = CARTESIAN_POINT ( 'NONE',  ( 4.641001526964561030, 50.00000000000000000, -8.016098858316205167 ) ) ;
#44186 = EDGE_CURVE ( 'NONE', #5556, #5426, #11265, .T. ) ;
#44187 = CARTESIAN_POINT ( 'NONE',  ( -14.99999999999906919, 16.00000000000000000, 0.000000000000000000 ) ) ;
#44188 = CARTESIAN_POINT ( 'NONE',  ( 358.0000000000000000, 167.8284271247463550, -342.8284271247465540 ) ) ;
#44189 = EDGE_LOOP ( 'NONE', ( #24277, #13442, #36596, #21026, #32959, #47652 ) ) ;
#44190 = CARTESIAN_POINT ( 'NONE',  ( -32.43949840348904701, -7.871562655726274116, -9.367992836599954742 ) ) ;
#44191 = EDGE_LOOP ( 'NONE', ( #7695, #1152, #26749, #11936 ) ) ;
#44192 = CARTESIAN_POINT ( 'NONE',  ( 1.250000000000000222, 0.000000000000000000, 10.00000000000000000 ) ) ;
#44193 = DIRECTION ( 'NONE',  ( -1.000000000000000000, -0.000000000000000000, -0.000000000000000000 ) ) ;
#44194 = FACE_BOUND ( 'NONE', #13131, .T. ) ;
#44195 = CARTESIAN_POINT ( 'NONE',  ( 210.0000000000000568, 2.143131898507881856E-16, -120.9317124430720582 ) ) ;
#44196 = CARTESIAN_POINT ( 'NONE',  ( -45.67084718096785423, -1.750000000000010436, 119.7931612910808781 ) ) ;
#44197 = DIRECTION ( 'NONE',  ( 0.000000000000000000, -1.000000000000000000, 0.000000000000000000 ) ) ;
#44198 = ORIENTED_EDGE ( 'NONE', *, *, #36560, .F. ) ;
#44199 = CARTESIAN_POINT ( 'NONE',  ( -8.445973446814976526, 0.000000000000000000, 165.0000000000000000 ) ) ;
#44200 = CARTESIAN_POINT ( 'NONE',  ( 343.9999999999999432, 174.9999999999996589, -358.0000000000003411 ) ) ;
#44201 = LINE ( 'NONE', #9078, #34019 ) ;
#44202 = AXIS2_PLACEMENT_3D ( 'NONE', #40522, #21019, #48418 ) ;
#44203 = VECTOR ( 'NONE', #6421, 1000.000000000000000 ) ;
#44204 = B_SPLINE_CURVE_WITH_KNOTS ( 'NONE', 3,
 ( #38135, #17604, #37136, #41462 ),
 .UNSPECIFIED., .F., .F.,
 ( 4, 4 ),
 ( 0.002099423004388898967, 0.008237935836937843731 ),
 .UNSPECIFIED. ) ;
#44205 = B_SPLINE_CURVE_WITH_KNOTS ( 'NONE', 3,
 ( #42746, #43009, #7625, #35097 ),
 .UNSPECIFIED., .F., .F.,
 ( 4, 4 ),
 ( 0.002645289245949297274, 0.008783374267191987328 ),
 .UNSPECIFIED. ) ;
#44206 = VECTOR ( 'NONE', #19091, 1000.000000000000000 ) ;
#44207 = CARTESIAN_POINT ( 'NONE',  ( 84.99999999999997158, 17.00000000000000000, -90.00000000000000000 ) ) ;
#44208 = ORIENTED_EDGE ( 'NONE', *, *, #32443, .F. ) ;
#44209 = CARTESIAN_POINT ( 'NONE',  ( 71.55402655318505367, 0.000000000000000000, -80.93171244307204404 ) ) ;
#44210 = VERTEX_POINT ( 'NONE', #23049 ) ;
#44211 = VECTOR ( 'NONE', #48686, 1000.000000000000000 ) ;
#44212 = CARTESIAN_POINT ( 'NONE',  ( 1.901953004002553405, 1.028591558669216255, 9.885585981620943485 ) ) ;
#44213 = DIRECTION ( 'NONE',  ( -0.000000000000000000, -1.000000000000000000, -0.000000000000000000 ) ) ;
#44214 = EDGE_CURVE ( 'NONE', #28470, #25557, #34216, .T. ) ;
#44215 = ORIENTED_EDGE ( 'NONE', *, *, #4904, .F. ) ;
#44216 = CARTESIAN_POINT ( 'NONE',  ( -126.6959734468149321, 1.749999999999997113, -39.18171244307202983 ) ) ;
#44217 = DIRECTION ( 'NONE',  ( -0.000000000000000000, -1.000000000000000000, -0.000000000000000000 ) ) ;
#44218 = CARTESIAN_POINT ( 'NONE',  ( -0.3862712429686895876, 1.188820645368940720, -10.00000000000000000 ) ) ;
#44219 = CARTESIAN_POINT ( 'NONE',  ( -210.0000000000000568, 0.000000000000000000, 120.8182875569279702 ) ) ;
#44220 = EDGE_LOOP ( 'NONE', ( #19927, #3417, #24375, #17, #17366, #40969 ) ) ;
#44221 = ORIENTED_EDGE ( 'NONE', *, *, #22115, .T. ) ;
#44222 = CARTESIAN_POINT ( 'NONE',  ( -166.6959734468149463, 0.000000000000000000, 165.0000000000000000 ) ) ;
#44223 = CARTESIAN_POINT ( 'NONE',  ( 12.78770032058947237, 31.68259716188277864, 7.455576670931136185 ) ) ;
#44224 = ORIENTED_EDGE ( 'NONE', *, *, #11386, .T. ) ;
#44225 = EDGE_LOOP ( 'NONE', ( #22501, #46827, #44719, #4787 ) ) ;
#44226 = DIRECTION ( 'NONE',  ( 0.000000000000000000, 1.000000000000000000, 0.000000000000000000 ) ) ;
#44227 = DIRECTION ( 'NONE',  ( 0.000000000000000000, -1.000000000000000000, 0.000000000000000000 ) ) ;
#44228 = CARTESIAN_POINT ( 'NONE',  ( -204.9459734468149463, 2.143131898507880377E-16, -0.9317124430720247208 ) ) ;
#44229 = DIRECTION ( 'NONE',  ( 0.000000000000000000, 5.664403186863042467E-17, 1.000000000000000000 ) ) ;
#44230 = ORIENTED_EDGE ( 'NONE', *, *, #47719, .F. ) ;
#44231 = VERTEX_POINT ( 'NONE', #11004 ) ;
#44232 = ORIENTED_EDGE ( 'NONE', *, *, #8953, .T. ) ;
#44233 = VECTOR ( 'NONE', #29914, 1000.000000000000000 ) ;
#44234 = FACE_OUTER_BOUND ( 'NONE', #30131, .T. ) ;
#44235 = VECTOR ( 'NONE', #32190, 1000.000000000000000 ) ;
#44236 = CIRCLE ( 'NONE', #49906, 1.750000000000001554 ) ;
#44237 = DIRECTION ( 'NONE',  ( 8.357767709911579088E-16, -1.000000000000000000, 1.822804496942680259E-16 ) ) ;
#44238 = ORIENTED_EDGE ( 'NONE', *, *, #40565, .T. ) ;
#44239 = VERTEX_POINT ( 'NONE', #42305 ) ;
#44240 = ADVANCED_FACE ( 'NONE', ( #22800, #14595, #26660, #14085, #46110, #22297, #49201, #42047, #7423, #45363, #2544, #22546, #38723, #30013, #49453, #6395, #33609, #15108, #49951, #18186, #38482, #18439, #50196, #34617, #14855, #10253, #38233, #25911, #46380, #29749, #10499 ), #14341, .F. ) ;
#44241 = VECTOR ( 'NONE', #11446, 1000.000000000000000 ) ;
#44242 = CARTESIAN_POINT ( 'NONE',  ( -10.30302290646040575, -13.08520913973572419, -9.683996418299976483 ) ) ;
#44243 = CIRCLE ( 'NONE', #5761, 1.750000000000008438 ) ;
#44244 = CARTESIAN_POINT ( 'NONE',  ( 0.1287570809895660084, -0.3962735484563127408, 10.00000000000000000 ) ) ;
#44245 = ORIENTED_EDGE ( 'NONE', *, *, #12642, .F. ) ;
#44246 = ORIENTED_EDGE ( 'NONE', *, *, #33547, .F. ) ;
#44247 = CARTESIAN_POINT ( 'NONE',  ( 35.05402655318504657, 2.143131898507880377E-16, 79.06828755692797017 ) ) ;
#44248 = CARTESIAN_POINT ( 'NONE',  ( -0.3862712429686809279, -1.188820645368943163, -10.00000000000000000 ) ) ;
#44249 = ORIENTED_EDGE ( 'NONE', *, *, #42434, .F. ) ;
#44250 = VECTOR ( 'NONE', #43408, 1000.000000000000000 ) ;
#44251 = CARTESIAN_POINT ( 'NONE',  ( -165.0000000000000284, 16.00000000000000000, -24.99999999999999289 ) ) ;
#44252 = DIRECTION ( 'NONE',  ( -1.000000000000000000, -0.000000000000000000, -0.000000000000000000 ) ) ;
#44253 = CARTESIAN_POINT ( 'NONE',  ( 181.0000000000000284, -174.9999999999999716, -95.00000000000014211 ) ) ;
#44254 = PLANE ( 'NONE',  #3600 ) ;
#44255 = ORIENTED_EDGE ( 'NONE', *, *, #48136, .T. ) ;
#44256 = CARTESIAN_POINT ( 'NONE',  ( -16.16402646813540755, 4.033894069732547827, -3.546734833711462365 ) ) ;
#44257 = DIRECTION ( 'NONE',  ( -1.000000000000000000, 0.000000000000000000, 1.860490536778032451E-50 ) ) ;
#44258 = B_SPLINE_CURVE_WITH_KNOTS ( 'NONE', 3,
 ( #29656, #26322, #2458, #13748 ),
 .UNSPECIFIED., .F., .F.,
 ( 4, 4 ),
 ( 1.734723475976807094E-18, 8.326314925919050278E-06 ),
 .UNSPECIFIED. ) ;
#44259 = CARTESIAN_POINT ( 'NONE',  ( -2.948105490345101387, -9.555557232197246620, 9.282506307616472441 ) ) ;
#44260 = LINE ( 'NONE', #40695, #37377 ) ;
#44261 = CARTESIAN_POINT ( 'NONE',  ( 155.0540265531850537, 2.143131898507880377E-16, 165.0000000000000000 ) ) ;
#44262 = CARTESIAN_POINT ( 'NONE',  ( -128.4459734468149179, 0.000000000000000000, 79.06828755692799859 ) ) ;
#44263 = LINE ( 'NONE', #681, #15188 ) ;
#44264 = CARTESIAN_POINT ( 'NONE',  ( 84.99999999999997158, 17.00000000000000000, -90.00000000000000000 ) ) ;
#44265 =( BOUNDED_CURVE ( )  B_SPLINE_CURVE ( 3, ( #37545, #14423, #26738, #30585 ),
 .UNSPECIFIED., .F., .F. ) 
 B_SPLINE_CURVE_WITH_KNOTS ( ( 4, 4 ),
 ( 1.570796326794896558, 3.141592653589793116 ),
 .UNSPECIFIED. ) 
 CURVE ( )  GEOMETRIC_REPRESENTATION_ITEM ( )  RATIONAL_B_SPLINE_CURVE ( ( 1.000000000000000000, 0.8047378541243649375, 0.8047378541243649375, 1.000000000000000000 ) ) 
 REPRESENTATION_ITEM ( '' )  );
#44266 = ORIENTED_EDGE ( 'NONE', *, *, #8020, .F. ) ;
#44267 = CARTESIAN_POINT ( 'NONE',  ( -14.48769039275601145, -30.44468701195584970, 8.807470649214879543 ) ) ;
#44268 = VECTOR ( 'NONE', #3381, 1000.000000000000000 ) ;
#44269 = CARTESIAN_POINT ( 'NONE',  ( -87.72109971266203843, 1.750000000000009548, 159.7931612910809065 ) ) ;
#44270 = ORIENTED_EDGE ( 'NONE', *, *, #9155, .F. ) ;
#44271 = CARTESIAN_POINT ( 'NONE',  ( -127.7210997126620242, 1.749999999999996225, 1.843413822775058497 ) ) ;
#44272 = CARTESIAN_POINT ( 'NONE',  ( 0.000000000000000000, 17.00000000000000000, 0.000000000000000000 ) ) ;
#44273 = LINE ( 'NONE', #39707, #11894 ) ;
#44274 = VERTEX_POINT ( 'NONE', #6647 ) ;
#44275 = CARTESIAN_POINT ( 'NONE',  ( -206.6959734468149463, -1.750000000000009992, 0.8182875569279768335 ) ) ;
#44276 = VERTEX_POINT ( 'NONE', #26906 ) ;
#44277 = CARTESIAN_POINT ( 'NONE',  ( -16.99749102614300966, 1.320765928724422222, 8.953103998512858652 ) ) ;
#44278 = CARTESIAN_POINT ( 'NONE',  ( -168.4459734468149463, 0.000000000000000000, -80.93171244307201562 ) ) ;
#44279 = ORIENTED_EDGE ( 'NONE', *, *, #37768, .F. ) ;
#44280 = LINE ( 'NONE', #25068, #19671 ) ;
#44281 = PLANE ( 'NONE',  #38031 ) ;
#44282 = ORIENTED_EDGE ( 'NONE', *, *, #25495, .T. ) ;
#44283 = VERTEX_POINT ( 'NONE', #45621 ) ;
#44284 =( BOUNDED_CURVE ( )  B_SPLINE_CURVE ( 3, ( #2129, #1877, #22628, #18256 ),
 .UNSPECIFIED., .F., .F. ) 
 B_SPLINE_CURVE_WITH_KNOTS ( ( 4, 4 ),
 ( 3.141592653589793116, 4.712388980384689674 ),
 .UNSPECIFIED. ) 
 CURVE ( )  GEOMETRIC_REPRESENTATION_ITEM ( )  RATIONAL_B_SPLINE_CURVE ( ( 1.000000000000000000, 0.8047378541243649375, 0.8047378541243649375, 1.000000000000000000 ) ) 
 REPRESENTATION_ITEM ( '' )  );
#44285 = PLANE ( 'NONE',  #5455 ) ;
#44286 = ORIENTED_EDGE ( 'NONE', *, *, #45602, .T. ) ;
#44287 = CYLINDRICAL_SURFACE ( 'NONE', #8612, 4.000000000000003553 ) ;
#44288 = CARTESIAN_POINT ( 'NONE',  ( 181.0000000000000000, -164.9999999999999432, -360.0000000000002274 ) ) ;
#44289 = LINE ( 'NONE', #36655, #43097 ) ;
#44290 = ORIENTED_EDGE ( 'NONE', *, *, #17405, .F. ) ;
#44291 = EDGE_CURVE ( 'NONE', #13960, #28737, #3544, .T. ) ;
#44292 = DIRECTION ( 'NONE',  ( 0.000000000000000000, -0.000000000000000000, -1.000000000000000000 ) ) ;
#44293 = CARTESIAN_POINT ( 'NONE',  ( 210.0000000000000568, 0.000000000000000000, 2.568287556927987048 ) ) ;
#44294 = ORIENTED_EDGE ( 'NONE', *, *, #21343, .T. ) ;
#44295 = ORIENTED_EDGE ( 'NONE', *, *, #30614, .T. ) ;
#44296 = ORIENTED_EDGE ( 'NONE', *, *, #31938, .T. ) ;
#44297 = CARTESIAN_POINT ( 'NONE',  ( -88.44597344681497475, 0.000000000000000000, 79.06828755692795596 ) ) ;
#44298 = EDGE_CURVE ( 'NONE', #27596, #5585, #37975, .T. ) ;
#44299 = CARTESIAN_POINT ( 'NONE',  ( 0.000000000000000000, -164.9999999999999432, -344.0000000000001705 ) ) ;
#44300 = VERTEX_POINT ( 'NONE', #30257 ) ;
#44301 = EDGE_CURVE ( 'NONE', #41021, #42350, #35661, .T. ) ;
#44302 = CARTESIAN_POINT ( 'NONE',  ( 152.2789002873379900, 1.750000000000009548, 41.84341382277508359 ) ) ;
#44303 = CARTESIAN_POINT ( 'NONE',  ( -84.94597344681497475, 0.000000000000000000, 162.5682875569279702 ) ) ;
#44304 = CARTESIAN_POINT ( 'NONE',  ( 210.0000000000000568, 0.000000000000000000, 82.56828755692799859 ) ) ;
#44305 = EDGE_CURVE ( 'NONE', #45850, #4734, #17120, .T. ) ;
#44306 = VECTOR ( 'NONE', #12872, 1000.000000000000000 ) ;
#44307 = LINE ( 'NONE', #33046, #34205 ) ;
#44308 = CARTESIAN_POINT ( 'NONE',  ( 2.500000000000050182, -204.9999999999999716, -234.7500000000000000 ) ) ;
#44309 = CARTESIAN_POINT ( 'NONE',  ( -177.4999999999999716, 74.83106485270648989, -130.5992382549688955 ) ) ;
#44310 = FACE_OUTER_BOUND ( 'NONE', #11695, .T. ) ;
#44311 = DIRECTION ( 'NONE',  ( 1.000000000000000000, 0.000000000000000000, -0.000000000000000000 ) ) ;
#44312 = CARTESIAN_POINT ( 'NONE',  ( -4.945973446814903696, 2.143131898507912917E-16, 39.06828755692792754 ) ) ;
#44313 = EDGE_CURVE ( 'NONE', #28555, #10095, #10744, .T. ) ;
#44314 = VECTOR ( 'NONE', #43520, 1000.000000000000000 ) ;
#44315 = CARTESIAN_POINT ( 'NONE',  ( 360.0000000000001137, 181.0000000000000284, 349.9999999999998295 ) ) ;
#44316 = DIRECTION ( 'NONE',  ( 0.000000000000000000, 0.000000000000000000, 1.000000000000000000 ) ) ;
#44317 = CARTESIAN_POINT ( 'NONE',  ( -208.4459734468149463, 0.000000000000000000, 159.0682875569279702 ) ) ;
#44318 = EDGE_LOOP ( 'NONE', ( #2642, #10912, #16774, #42328, #44108, #3604 ) ) ;
#44319 = CARTESIAN_POINT ( 'NONE',  ( 2.538055338523173443, 50.00000000000000000, -9.367992836599951190 ) ) ;
#44320 = DIRECTION ( 'NONE',  ( -1.000000000000000000, 0.000000000000000000, 0.000000000000000000 ) ) ;
#44321 = CARTESIAN_POINT ( 'NONE',  ( 195.9526953830863079, 159.2880105690400399, 472.8425600500171981 ) ) ;
#44322 = EDGE_CURVE ( 'NONE', #19392, #7505, #16372, .T. ) ;
#44323 = ADVANCED_FACE ( 'NONE', ( #43054 ), #13411, .T. ) ;
#44324 = CARTESIAN_POINT ( 'NONE',  ( -115.0000000000000284, 17.00000000000000000, -90.00000000000000000 ) ) ;
#44326 = ORIENTED_EDGE ( 'NONE', *, *, #45226, .F. ) ;
#44325 = EDGE_CURVE ( 'NONE', #9127, #38516, #39489, .T. ) ;
#44327 = CARTESIAN_POINT ( 'NONE',  ( -206.6959734468149463, 0.000000000000000000, 165.0000000000000000 ) ) ;
#44328 = ADVANCED_FACE ( 'NONE', ( #31790 ), #46618, .F. ) ;
#44329 = CARTESIAN_POINT ( 'NONE',  ( -128.4459734468149463, -1.025126265847081886, 39.06828755692799149 ) ) ;
#44330 = VERTEX_POINT ( 'NONE', #8689 ) ;
#44331 = EDGE_CURVE ( 'NONE', #35777, #32189, #24347, .T. ) ;
#44332 = DIRECTION ( 'NONE',  ( -0.000000000000000000, -1.000000000000000000, -0.000000000000000000 ) ) ;
#44333 = CARTESIAN_POINT ( 'NONE',  ( 164.9999999999999716, -256.5000000000000000, -114.9999999999999432 ) ) ;
#44334 = CARTESIAN_POINT ( 'NONE',  ( 164.9999999999999716, 17.00000000000000000, -60.00000000000001421 ) ) ;
#44335 = AXIS2_PLACEMENT_3D ( 'NONE', #14101, #33378, #25672 ) ;
#44336 = ADVANCED_FACE ( 'NONE', ( #20225 ), #3813, .F. ) ;
#44337 = ORIENTED_EDGE ( 'NONE', *, *, #36982, .F. ) ;
#44338 = ORIENTED_EDGE ( 'NONE', *, *, #23050, .F. ) ;
#44339 = VERTEX_POINT ( 'NONE', #43308 ) ;
#44340 = AXIS2_PLACEMENT_3D ( 'NONE', #39491, #234, #4329 ) ;
#44341 = ORIENTED_EDGE ( 'NONE', *, *, #21185, .F. ) ;
#44342 = CARTESIAN_POINT ( 'NONE',  ( 75.05402655318509630, 2.143131898507880377E-16, 79.06828755692797017 ) ) ;
#44343 = CARTESIAN_POINT ( 'NONE',  ( 7.499999999999948486, -194.9999999999999716, -240.0000000000000000 ) ) ;
#44344 = EDGE_LOOP ( 'NONE', ( #13553, #22794, #2773, #3416 ) ) ;
#44345 = DIRECTION ( 'NONE',  ( 0.000000000000000000, -1.000000000000000000, 1.822804496942679766E-16 ) ) ;
#44346 = LINE ( 'NONE', #1778, #11159 ) ;
#44347 = FACE_OUTER_BOUND ( 'NONE', #46275, .T. ) ;
#44348 = VECTOR ( 'NONE', #39898, 1000.000000000000000 ) ;
#44349 = DIRECTION ( 'NONE',  ( -1.000000000000000000, 0.000000000000000000, 0.000000000000000000 ) ) ;
#44350 = EDGE_CURVE ( 'NONE', #2419, #39109, #3435, .T. ) ;
#44351 = ORIENTED_EDGE ( 'NONE', *, *, #28379, .T. ) ;
#44352 = CYLINDRICAL_SURFACE ( 'NONE', #41202, 0.5000000000000004441 ) ;
#44353 = EDGE_CURVE ( 'NONE', #8231, #5904, #12269, .T. ) ;
#44354 = EDGE_LOOP ( 'NONE', ( #22518, #39471, #10920, #4035 ) ) ;
#44355 = EDGE_CURVE ( 'NONE', #18141, #42504, #3464, .T. ) ;
#44356 = LINE ( 'NONE', #5115, #28380 ) ;
#44357 = DIRECTION ( 'NONE',  ( 1.000000000000000000, 0.000000000000000000, 0.000000000000000000 ) ) ;
#44358 = EDGE_LOOP ( 'NONE', ( #43749, #32446, #9377, #32085 ) ) ;
#44359 = EDGE_LOOP ( 'NONE', ( #19247, #43917, #45683, #5446, #28996, #25293 ) ) ;
#44360 = ORIENTED_EDGE ( 'NONE', *, *, #21238, .T. ) ;
#44361 = LINE ( 'NONE', #21036, #27866 ) ;
#44362 = LINE ( 'NONE', #20529, #42221 ) ;
#44363 = VERTEX_POINT ( 'NONE', #19963 ) ;
#44364 = EDGE_CURVE ( 'NONE', #21827, #35427, #19192, .T. ) ;
#44365 = CARTESIAN_POINT ( 'NONE',  ( 0.3370904143228947158, 0.2449105217885311492, 10.00000000000000000 ) ) ;
#44366 = FILL_AREA_STYLE_COLOUR ( '', #23795 ) ;
#44367 = CARTESIAN_POINT ( 'NONE',  ( 10.30302290646030627, 13.08520913973580058, -9.683996418299976483 ) ) ;
#44368 = ORIENTED_EDGE ( 'NONE', *, *, #10866, .T. ) ;
#44369 =( BOUNDED_CURVE ( )  B_SPLINE_CURVE ( 3, ( #15354, #42033, #46360, #50447 ),
 .UNSPECIFIED., .F., .F. ) 
 B_SPLINE_CURVE_WITH_KNOTS ( ( 4, 4 ),
 ( 1.570796326794896558, 3.141592653589793116 ),
 .UNSPECIFIED. ) 
 CURVE ( )  GEOMETRIC_REPRESENTATION_ITEM ( )  RATIONAL_B_SPLINE_CURVE ( ( 1.000000000000000000, 0.8047378541243649375, 0.8047378541243649375, 1.000000000000000000 ) ) 
 REPRESENTATION_ITEM ( '' )  );
#44370 = CARTESIAN_POINT ( 'NONE',  ( -44.94597344681493922, 2.143131898507880377E-16, 119.0682875569279702 ) ) ;
#44371 = CARTESIAN_POINT ( 'NONE',  ( 168.9999999999998579, -184.9999999999999716, -340.0000000000001137 ) ) ;
#44372 = VECTOR ( 'NONE', #42098, 1000.000000000000000 ) ;
#44373 = ORIENTED_EDGE ( 'NONE', *, *, #48967, .T. ) ;
#44374 = ADVANCED_FACE ( 'NONE', ( #34882 ), #8179, .F. ) ;
#44375 = VERTEX_POINT ( 'NONE', #23828 ) ;
#44376 = CARTESIAN_POINT ( 'NONE',  ( 165.0000000000000000, 2.775557561562891351E-14, -115.0000000000001563 ) ) ;
#44377 = DIRECTION ( 'NONE',  ( 0.000000000000000000, 1.000000000000000000, 0.000000000000000000 ) ) ;
#44378 = VECTOR ( 'NONE', #36035, 1000.000000000000000 ) ;
#44379 = EDGE_CURVE ( 'NONE', #18308, #29317, #48243, .T. ) ;
#44380 = CARTESIAN_POINT ( 'NONE',  ( -20.40054609052957701, 26.26366202847989229, -3.760136334089591248 ) ) ;
#44381 = CARTESIAN_POINT ( 'NONE',  ( 0.3862712429686810944, 1.188820645368943607, 3.333333333333333481 ) ) ;
#44382 = ORIENTED_EDGE ( 'NONE', *, *, #43209, .T. ) ;
#44383 = LINE ( 'NONE', #24914, #3404 ) ;
#44384 = CARTESIAN_POINT ( 'NONE',  ( -14.29087950072019098, -9.652079258044555132, 8.727788335465566760 ) ) ;
#44385 = FACE_OUTER_BOUND ( 'NONE', #42668, .T. ) ;
#44386 = CARTESIAN_POINT ( 'NONE',  ( -14.99999999999845812, 17.00000000000000000, 60.00000000000000000 ) ) ;
#44388 = ORIENTED_EDGE ( 'NONE', *, *, #12059, .F. ) ;
#44387 = ADVANCED_FACE ( 'NONE', ( #4327 ), #28438, .T. ) ;
#44389 = DIRECTION ( 'NONE',  ( -1.000000000000000000, -0.000000000000000000, -0.000000000000000000 ) ) ;
#44390 = EDGE_CURVE ( 'NONE', #55, #33080, #2420, .T. ) ;
#44391 = ORIENTED_EDGE ( 'NONE', *, *, #32914, .F. ) ;
#44392 = CARTESIAN_POINT ( 'NONE',  ( -207.7210997126620384, -1.750000000000009548, -38.15658617722494483 ) ) ;
#44393 = ORIENTED_EDGE ( 'NONE', *, *, #22169, .F. ) ;
#44394 = CARTESIAN_POINT ( 'NONE',  ( 74.32915281903215998, 1.750000000000009548, -158.1565861772249377 ) ) ;
#44395 = CYLINDRICAL_SURFACE ( 'NONE', #1192, 1.750000000000001554 ) ;
#44396 = EDGE_CURVE ( 'NONE', #18600, #40520, #49072, .T. ) ;
#44397 = CARTESIAN_POINT ( 'NONE',  ( 130.0000000000018474, 16.00000000000000000, 65.00000000000000000 ) ) ;
#44398 = ORIENTED_EDGE ( 'NONE', *, *, #20329, .F. ) ;
#44399 = ADVANCED_FACE ( 'NONE', ( #22179 ), #14474, .T. ) ;
#44400 = EDGE_CURVE ( 'NONE', #24759, #34532, #13513, .T. ) ;
#44401 = LINE ( 'NONE', #35992, #22028 ) ;
#44402 = ORIENTED_EDGE ( 'NONE', *, *, #31827, .T. ) ;
#44403 = CARTESIAN_POINT ( 'NONE',  ( -164.9999999999994031, 17.00000000000000000, -54.99999999999999289 ) ) ;
#44404 = CARTESIAN_POINT ( 'NONE',  ( 344.0000000000000000, -165.0000000000001137, -340.0000000000002842 ) ) ;
#44405 = VECTOR ( 'NONE', #28873, 1000.000000000000000 ) ;
#44406 = CARTESIAN_POINT ( 'NONE',  ( -8.445973446814976526, 0.000000000000000000, 165.0000000000000000 ) ) ;
#44407 = CARTESIAN_POINT ( 'NONE',  ( 358.0000000000000000, -169.0000000000001137, 344.0000000000000000 ) ) ;
#44408 = AXIS2_PLACEMENT_3D ( 'NONE', #11384, #10876, #50073 ) ;
#44409 = ORIENTED_EDGE ( 'NONE', *, *, #3960, .F. ) ;
#44410 = ORIENTED_EDGE ( 'NONE', *, *, #18171, .T. ) ;
#44411 = DIRECTION ( 'NONE',  ( 0.000000000000000000, 0.000000000000000000, 1.000000000000000000 ) ) ;
#44412 = ORIENTED_EDGE ( 'NONE', *, *, #13563, .T. ) ;
#44413 = ADVANCED_FACE ( 'NONE', ( #10118 ), #28677, .F. ) ;
#44414 = VECTOR ( 'NONE', #29480, 1000.000000000000000 ) ;
#44415 = DIRECTION ( 'NONE',  ( 1.000000000000000000, -0.000000000000000000, -0.000000000000000000 ) ) ;
#44416 = CARTESIAN_POINT ( 'NONE',  ( -125.6708471809678542, -1.749999999999997113, -80.20683870891909351 ) ) ;
#44417 = CARTESIAN_POINT ( 'NONE',  ( -165.3973046169136012, 54.43801056904003133, -17.65743994998275213 ) ) ;
#44418 = ORIENTED_EDGE ( 'NONE', *, *, #22703, .F. ) ;
#44419 = CARTESIAN_POINT ( 'NONE',  ( -127.7210997126620242, 1.749999999999997113, -120.2068387089191219 ) ) ;
#44420 = CYLINDRICAL_SURFACE ( 'NONE', #45559, 1.750000000000015543 ) ;
#44421 = B_SPLINE_SURFACE_WITH_KNOTS ( 'NONE', 3, 3, ( 
 ( #13740, #25806, #45524, #9396 ),
 ( #21952, #6044, #10406, #6311 ),
 ( #25297, #26057, #1703, #41705 ),
 ( #44773, #6553, #49603, #14500 ) ),
 .UNSPECIFIED., .F., .F., .F.,
 ( 4, 4 ),
 ( 4, 4 ),
 ( 0.000000000000000000, 1.000000000000000000 ),
 ( 0.000000000000000000, 1.000000000000000000 ),
 .UNSPECIFIED. ) ;
#44422 = CARTESIAN_POINT ( 'NONE',  ( 175.0000000000000000, 15.00000000000000000, 122.5000000000000142 ) ) ;
#44423 = CYLINDRICAL_SURFACE ( 'NONE', #38245, 1.750000000000010214 ) ;
#44424 = CARTESIAN_POINT ( 'NONE',  ( 31.55402655318503236, 0.000000000000000000, -0.9317124430720247208 ) ) ;
#44425 =( BOUNDED_CURVE ( )  B_SPLINE_CURVE ( 3, ( #24995, #43716, #48536, #40395 ),
 .UNSPECIFIED., .F., .F. ) 
 B_SPLINE_CURVE_WITH_KNOTS ( ( 4, 4 ),
 ( 3.141592653589793116, 4.712388980384689674 ),
 .UNSPECIFIED. ) 
 CURVE ( )  GEOMETRIC_REPRESENTATION_ITEM ( )  RATIONAL_B_SPLINE_CURVE ( ( 1.000000000000000000, 0.8047378541243649375, 0.8047378541243649375, 1.000000000000000000 ) ) 
 REPRESENTATION_ITEM ( '' )  );
#44426 = LINE ( 'NONE', #48252, #43582 ) ;
#44427 = VERTEX_POINT ( 'NONE', #9176 ) ;
#44428 = ORIENTED_EDGE ( 'NONE', *, *, #50255, .F. ) ;
#44429 = ORIENTED_EDGE ( 'NONE', *, *, #172, .T. ) ;
#44430 = CARTESIAN_POINT ( 'NONE',  ( 4.339432828817248122, 37.24807810779213213, -8.192531242611266862 ) ) ;
#44431 = DIRECTION ( 'NONE',  ( -0.000000000000000000, -0.000000000000000000, -1.000000000000000000 ) ) ;
#44432 =( BOUNDED_CURVE ( )  B_SPLINE_CURVE ( 3, ( #28457, #7949, #39249, #507 ),
 .UNSPECIFIED., .F., .F. ) 
 B_SPLINE_CURVE_WITH_KNOTS ( ( 4, 4 ),
 ( 3.141592653589793116, 4.712388980384689674 ),
 .UNSPECIFIED. ) 
 CURVE ( )  GEOMETRIC_REPRESENTATION_ITEM ( )  RATIONAL_B_SPLINE_CURVE ( ( 1.000000000000000000, 0.8047378541243649375, 0.8047378541243649375, 1.000000000000000000 ) ) 
 REPRESENTATION_ITEM ( '' )  );
#44433 = CARTESIAN_POINT ( 'NONE',  ( 135.0000000000015632, 17.00000000000000000, 60.00000000000000000 ) ) ;
#44434 = ORIENTED_EDGE ( 'NONE', *, *, #38802, .T. ) ;
#44435 = CARTESIAN_POINT ( 'NONE',  ( -14.29087950072019098, -9.652079258044555132, 8.727788335465566760 ) ) ;
#44436 = ORIENTED_EDGE ( 'NONE', *, *, #33705, .T. ) ;
#44437 = CARTESIAN_POINT ( 'NONE',  ( -3.996390545799824334, 16.57371371864897469, 8.953103998512858652 ) ) ;
#44438 = CARTESIAN_POINT ( 'NONE',  ( 210.0000000000000568, 0.000000000000000000, -117.4317124430720298 ) ) ;
#44439 = PLANE ( 'NONE',  #8641 ) ;
#44440 = DIRECTION ( 'NONE',  ( -0.000000000000000000, -0.000000000000000000, -1.000000000000000000 ) ) ;
#44441 = DIRECTION ( 'NONE',  ( 1.000000000000000000, 0.000000000000000000, 0.000000000000000000 ) ) ;
#44442 = LINE ( 'NONE', #13670, #25657 ) ;
#44443 = ORIENTED_EDGE ( 'NONE', *, *, #32894, .T. ) ;
#44444 = DIRECTION ( 'NONE',  ( -1.000000000000000000, -0.000000000000000000, -0.000000000000000000 ) ) ;
#44445 = VECTOR ( 'NONE', #18564, 1000.000000000000000 ) ;
#44446 = CARTESIAN_POINT ( 'NONE',  ( -0.1469336902871204442, -1.496274467947957376, 9.953784399990622589 ) ) ;
#44447 = AXIS2_PLACEMENT_3D ( 'NONE', #33634, #48220, #45391 ) ;
#44448 = EDGE_CURVE ( 'NONE', #23110, #23498, #48543, .T. ) ;
#44449 = CARTESIAN_POINT ( 'NONE',  ( -5.000000000000000000, -175.0000000000000284, 346.2500000000002274 ) ) ;
#44450 = EDGE_CURVE ( 'NONE', #26268, #23532, #10382, .T. ) ;
#44451 = ORIENTED_EDGE ( 'NONE', *, *, #6106, .T. ) ;
#44452 = VECTOR ( 'NONE', #9977, 1000.000000000000000 ) ;
#44453 = CARTESIAN_POINT ( 'NONE',  ( 168.9999999999999716, -79.49999999999997158, -350.0000000000001705 ) ) ;
#44454 = EDGE_LOOP ( 'NONE', ( #10441, #41226, #5757, #24139 ) ) ;
#44455 = CARTESIAN_POINT ( 'NONE',  ( -124.9459734468149463, 2.143131898507847836E-16, 165.0000000000000000 ) ) ;
#44456 = DIRECTION ( 'NONE',  ( -0.000000000000000000, -1.000000000000000000, -0.000000000000000000 ) ) ;
#44457 = EDGE_CURVE ( 'NONE', #22853, #25007, #41424, .T. ) ;
#44458 = CARTESIAN_POINT ( 'NONE',  ( 210.0000000000000568, 0.000000000000000000, 160.8182875569279702 ) ) ;
#44459 = ORIENTED_EDGE ( 'NONE', *, *, #7273, .F. ) ;
#44460 = EDGE_CURVE ( 'NONE', #23532, #10351, #5065, .T. ) ;
#44461 = EDGE_CURVE ( 'NONE', #4495, #1717, #6518, .T. ) ;
#44462 = ORIENTED_EDGE ( 'NONE', *, *, #6094, .F. ) ;
#44463 = CARTESIAN_POINT ( 'NONE',  ( -1.011271242968693862, 0.7347315653655780432, 10.00000000000000000 ) ) ;
#44464 = LINE ( 'NONE', #41395, #17269 ) ;
#44465 = CARTESIAN_POINT ( 'NONE',  ( -0.1287570809895576818, -0.3962735484563154609, 10.00000000000000000 ) ) ;
#44466 = EDGE_CURVE ( 'NONE', #22708, #25574, #1492, .T. ) ;
#44467 = EDGE_LOOP ( 'NONE', ( #40065, #25968, #30167, #46311 ) ) ;
#44468 = ORIENTED_EDGE ( 'NONE', *, *, #12832, .F. ) ;
#44469 = FACE_OUTER_BOUND ( 'NONE', #32265, .T. ) ;
#44470 = FACE_OUTER_BOUND ( 'NONE', #5977, .T. ) ;
#44471 = EDGE_LOOP ( 'NONE', ( #47409, #48469, #44724, #46492 ) ) ;
#44472 = ORIENTED_EDGE ( 'NONE', *, *, #42143, .T. ) ;
#44473 = DIRECTION ( 'NONE',  ( -6.765175596986472868E-16, 0.9749645535258953943, -0.2223603367690637489 ) ) ;
#44474 = CARTESIAN_POINT ( 'NONE',  ( 240.0000000000000000, -164.9999999999999716, 444.9999999999998295 ) ) ;
#44475 = FACE_OUTER_BOUND ( 'NONE', #27537, .T. ) ;
#44476 = AXIS2_PLACEMENT_3D ( 'NONE', #46839, #15340, #448 ) ;
#44477 = FACE_OUTER_BOUND ( 'NONE', #20880, .T. ) ;
#44478 = ORIENTED_EDGE ( 'NONE', *, *, #17055, .T. ) ;
#44479 = ORIENTED_EDGE ( 'NONE', *, *, #50556, .F. ) ;
#44480 = AXIS2_PLACEMENT_3D ( 'NONE', #40992, #36925, #17388 ) ;
#44481 = ORIENTED_EDGE ( 'NONE', *, *, #28374, .F. ) ;
#44482 = DIRECTION ( 'NONE',  ( 0.000000000000000000, 0.000000000000000000, -1.000000000000000000 ) ) ;
#44483 = CARTESIAN_POINT ( 'NONE',  ( -27.33593271309441519, 41.94268121623345280, -9.367992836599951190 ) ) ;
#44484 = AXIS2_PLACEMENT_3D ( 'NONE', #46633, #35668, #7686 ) ;
#44485 = CARTESIAN_POINT ( 'NONE',  ( 193.3040265531851105, 1.750000000000010214, -39.18171244307202983 ) ) ;
#44486 = EDGE_LOOP ( 'NONE', ( #22329, #6496, #17750, #25257 ) ) ;
#44487 = ORIENTED_EDGE ( 'NONE', *, *, #25301, .F. ) ;
#44488 = CYLINDRICAL_SURFACE ( 'NONE', #8754, 1.750000000000001554 ) ;
#44489 = DIRECTION ( 'NONE',  ( 0.000000000000000000, 0.000000000000000000, 1.000000000000000000 ) ) ;
#44490 = EDGE_LOOP ( 'NONE', ( #16119, #49128, #13503, #31116 ) ) ;
#44491 = VERTEX_POINT ( 'NONE', #18307 ) ;
#44492 = EDGE_CURVE ( 'NONE', #19484, #26976, #8927, .T. ) ;
#44493 = CARTESIAN_POINT ( 'NONE',  ( 33.86622497129647513, -3.037805405904928868, 7.906207997025717304 ) ) ;
#44494 = CARTESIAN_POINT ( 'NONE',  ( -126.6959734468149321, 1.749999999999997335, 80.81828755692798438 ) ) ;
#44495 = VERTEX_POINT ( 'NONE', #20725 ) ;
#44496 = DIRECTION ( 'NONE',  ( 0.000000000000000000, 0.000000000000000000, 1.000000000000000000 ) ) ;
#44497 = DIRECTION ( 'NONE',  ( 0.000000000000000000, 0.000000000000000000, -1.000000000000000000 ) ) ;
#44498 = CARTESIAN_POINT ( 'NONE',  ( -85.67084718096784002, -1.750000000000009548, -160.2068387089191219 ) ) ;
#44499 = CARTESIAN_POINT ( 'NONE',  ( -54.99999999999997868, 52.49999999999999289, 5.000000000000000000 ) ) ;
#44500 = ORIENTED_EDGE ( 'NONE', *, *, #9216, .F. ) ;
#44501 = CARTESIAN_POINT ( 'NONE',  ( -0.3862712429686809279, -1.188820645368943163, -3.333333333333333481 ) ) ;
#44502 = DIRECTION ( 'NONE',  ( -0.000000000000000000, -0.000000000000000000, -1.000000000000000000 ) ) ;
#44503 = CARTESIAN_POINT ( 'NONE',  ( -164.9459734468149463, 2.143131898507880377E-16, -117.4317124430720725 ) ) ;
#44504 = CARTESIAN_POINT ( 'NONE',  ( 0.9925179869589159098, 0.000000000000000000, 0.000000000000000000 ) ) ;
#44505 = CARTESIAN_POINT ( 'NONE',  ( -88.44597344681497475, 0.000000000000000000, -0.9317124430720524764 ) ) ;
#44506 = CIRCLE ( 'NONE', #25714, 2.000000000000001776 ) ;
#44507 = DIRECTION ( 'NONE',  ( -0.000000000000000000, -0.000000000000000000, 1.000000000000000000 ) ) ;
#44508 = VECTOR ( 'NONE', #26857, 1000.000000000000000 ) ;
#44509 = CARTESIAN_POINT ( 'NONE',  ( -1.377509002708424468, 0.6027468487255034368, 9.927319414211229542 ) ) ;
#44510 = DIRECTION ( 'NONE',  ( -1.000000000000000000, 0.000000000000000000, 0.000000000000000000 ) ) ;
#44511 = VECTOR ( 'NONE', #37260, 1000.000000000000000 ) ;
#44512 = ORIENTED_EDGE ( 'NONE', *, *, #43464, .F. ) ;
#44513 = CARTESIAN_POINT ( 'NONE',  ( -46.69597344681494633, 1.750000000000010658, 120.8182875569279702 ) ) ;
#44514 = FACE_OUTER_BOUND ( 'NONE', #44454, .T. ) ;
#44515 = DIRECTION ( 'NONE',  ( 0.000000000000000000, 0.000000000000000000, 1.000000000000000000 ) ) ;
#44516 = EDGE_CURVE ( 'NONE', #16304, #46031, #24582, .T. ) ;
#44517 = CARTESIAN_POINT ( 'NONE',  ( 75.05402655318509630, 1.025126265847089435, 2.568287556927986159 ) ) ;
#44518 = CYLINDRICAL_SURFACE ( 'NONE', #20086, 2.000000000000001776 ) ;
#44519 = ORIENTED_EDGE ( 'NONE', *, *, #20462, .T. ) ;
#44520 = DIRECTION ( 'NONE',  ( 0.000000000000000000, 0.000000000000000000, -1.000000000000000000 ) ) ;
#44521 = B_SPLINE_SURFACE_WITH_KNOTS ( 'NONE', 3, 3, ( 
 ( #6704, #45924, #22350, #10549 ),
 ( #38026, #26214, #2841, #18501 ),
 ( #34181, #14656, #30316, #42096 ),
 ( #22610, #38292, #3100, #14914 ) ),
 .UNSPECIFIED., .F., .F., .F.,
 ( 4, 4 ),
 ( 4, 4 ),
 ( 0.000000000000000000, 1.000000000000000000 ),
 ( 0.000000000000000000, 1.000000000000000000 ),
 .UNSPECIFIED. ) ;
#44522 = ORIENTED_EDGE ( 'NONE', *, *, #22506, .T. ) ;
#44523 = CARTESIAN_POINT ( 'NONE',  ( -165.3973046169136012, 70.03596893647589638, -94.69675437945477370 ) ) ;
#44524 = PLANE ( 'NONE',  #49986 ) ;
#44525 = ORIENTED_EDGE ( 'NONE', *, *, #40619, .F. ) ;
#44526 = CARTESIAN_POINT ( 'NONE',  ( 31.55402655318503236, 0.000000000000000000, 79.06828755692797017 ) ) ;
#44527 = LINE ( 'NONE', #16606, #347 ) ;
#44528 = ORIENTED_EDGE ( 'NONE', *, *, #10780, .T. ) ;
#44529 = ORIENTED_EDGE ( 'NONE', *, *, #45267, .F. ) ;
#44530 = CARTESIAN_POINT ( 'NONE',  ( 2.538055338523177440, 50.00000000000000711, -9.367992836599954742 ) ) ;
#44531 = CARTESIAN_POINT ( 'NONE',  ( 16.76006782980217125, -2.050259795448531541, 9.178419661560148768 ) ) ;
#44532 = CARTESIAN_POINT ( 'NONE',  ( -1.256098972485658383, -0.9750543259410950903, 9.933337059263825708 ) ) ;
#44533 = ORIENTED_EDGE ( 'NONE', *, *, #37829, .F. ) ;
#44534 = CARTESIAN_POINT ( 'NONE',  ( -88.44597344681494633, -1.025126265847089879, -77.43171244307200141 ) ) ;
#44535 = ORIENTED_EDGE ( 'NONE', *, *, #8060, .F. ) ;
#44536 = ORIENTED_EDGE ( 'NONE', *, *, #10815, .F. ) ;
#44537 = ORIENTED_EDGE ( 'NONE', *, *, #21107, .T. ) ;
#44538 = CARTESIAN_POINT ( 'NONE',  ( -194.9999999999999432, 173.0000000000000000, 252.0000000000000000 ) ) ;
#44539 = AXIS2_PLACEMENT_3D ( 'NONE', #9945, #2996, #15060 ) ;
#44540 = ORIENTED_EDGE ( 'NONE', *, *, #46790, .T. ) ;
#44541 = CIRCLE ( 'NONE', #37213, 1.880036658038868991 ) ;
#44542 = EDGE_CURVE ( 'NONE', #17971, #36229, #40233, .T. ) ;
#44543 = CARTESIAN_POINT ( 'NONE',  ( 0.000000000000000000, -174.9999999999999147, 500.0000000000001137 ) ) ;
#44544 = CARTESIAN_POINT ( 'NONE',  ( -5.670847180967843570, 1.750000000000023537, -118.1565861772249519 ) ) ;
#44545 = CARTESIAN_POINT ( 'NONE',  ( -164.9999999999987779, 17.00000000000000000, 30.00000000000000000 ) ) ;
#44546 = CARTESIAN_POINT ( 'NONE',  ( 36.76598589393955052, 7.383243274241862331, -8.192531242611266862 ) ) ;
#44547 = CARTESIAN_POINT ( 'NONE',  ( -206.6959734468149463, 1.750000000000010214, 40.81828755692798438 ) ) ;
#44548 = LINE ( 'NONE', #44814, #17725 ) ;
#44549 = FACE_OUTER_BOUND ( 'NONE', #40227, .T. ) ;
#44550 = CARTESIAN_POINT ( 'NONE',  ( 0.8155877869298099325, 0.9072449372238458043, 9.963925895597341764 ) ) ;
#44551 = DIRECTION ( 'NONE',  ( -1.000000000000000000, -0.000000000000000000, -0.000000000000000000 ) ) ;
#44552 = CARTESIAN_POINT ( 'NONE',  ( -20.40054609052957701, 26.26366202847989229, -3.760136334089591248 ) ) ;
#44553 =( BOUNDED_CURVE ( )  B_SPLINE_CURVE ( 3, ( #46461, #46717, #18782, #49544 ),
 .UNSPECIFIED., .F., .F. ) 
 B_SPLINE_CURVE_WITH_KNOTS ( ( 4, 4 ),
 ( 4.712388980384689674, 6.283185307179586232 ),
 .UNSPECIFIED. ) 
 CURVE ( )  GEOMETRIC_REPRESENTATION_ITEM ( )  RATIONAL_B_SPLINE_CURVE ( ( 1.000000000000000000, 0.8047378541243649375, 0.8047378541243649375, 1.000000000000000000 ) ) 
 REPRESENTATION_ITEM ( '' )  );
#44554 = VECTOR ( 'NONE', #48580, 1000.000000000000000 ) ;
#44555 = CARTESIAN_POINT ( 'NONE',  ( -24.47767542868268364, 23.18653802921800278, 8.807470649214879543 ) ) ;
#44556 = VERTEX_POINT ( 'NONE', #17132 ) ;
#44557 = DIRECTION ( 'NONE',  ( -1.000000000000000000, 0.000000000000000000, 0.000000000000000000 ) ) ;
#44558 =( BOUNDED_CURVE ( )  B_SPLINE_CURVE ( 3, ( #30923, #27993, #44134, #36474 ),
 .UNSPECIFIED., .F., .F. ) 
 B_SPLINE_CURVE_WITH_KNOTS ( ( 4, 4 ),
 ( 1.570796326794896558, 3.141592653589793116 ),
 .UNSPECIFIED. ) 
 CURVE ( )  GEOMETRIC_REPRESENTATION_ITEM ( )  RATIONAL_B_SPLINE_CURVE ( ( 1.000000000000000000, 0.8047378541243649375, 0.8047378541243649375, 1.000000000000000000 ) ) 
 REPRESENTATION_ITEM ( '' )  );
#44559 = LINE ( 'NONE', #9191, #50694 ) ;
#44560 = DIRECTION ( 'NONE',  ( 0.000000000000000000, -0.000000000000000000, 1.000000000000000000 ) ) ;
#44561 = CARTESIAN_POINT ( 'NONE',  ( 193.3040265531851105, 1.750000000000009992, 0.8182875569279768335 ) ) ;
#44562 = ORIENTED_EDGE ( 'NONE', *, *, #5165, .T. ) ;
#44563 = CARTESIAN_POINT ( 'NONE',  ( -168.4459734468149463, 0.000000000000000000, -117.4317124430720725 ) ) ;
#44564 = CARTESIAN_POINT ( 'NONE',  ( -126.6959734468149321, -1.749999999999997113, 40.81828755692798438 ) ) ;
#44565 = VECTOR ( 'NONE', #50057, 1000.000000000000000 ) ;
#44566 = VERTEX_POINT ( 'NONE', #32549 ) ;
#44567 = LINE ( 'NONE', #43591, #18890 ) ;
#44568 = ADVANCED_FACE ( 'NONE', ( #13017 ), #41928, .F. ) ;
#44569 = AXIS2_PLACEMENT_3D ( 'NONE', #23141, #38819, #46964 ) ;
#44570 = FACE_OUTER_BOUND ( 'NONE', #47015, .T. ) ;
#44571 = DIRECTION ( 'NONE',  ( -1.000000000000000000, 0.000000000000000000, 0.000000000000000000 ) ) ;
#44572 =( BOUNDED_CURVE ( )  B_SPLINE_CURVE ( 3, ( #13385, #25194, #40840, #41098 ),
 .UNSPECIFIED., .F., .F. ) 
 B_SPLINE_CURVE_WITH_KNOTS ( ( 4, 4 ),
 ( 0.000000000000000000, 1.570796326794896558 ),
 .UNSPECIFIED. ) 
 CURVE ( )  GEOMETRIC_REPRESENTATION_ITEM ( )  RATIONAL_B_SPLINE_CURVE ( ( 1.000000000000000000, 0.8047378541243649375, 0.8047378541243649375, 1.000000000000000000 ) ) 
 REPRESENTATION_ITEM ( '' )  );
#44573 = ORIENTED_EDGE ( 'NONE', *, *, #38380, .F. ) ;
#44574 = CARTESIAN_POINT ( 'NONE',  ( 71.55402655318505367, -1.025126265847089657, -80.93171244307201562 ) ) ;
#44575 = ORIENTED_EDGE ( 'NONE', *, *, #8680, .F. ) ;
#44576 = ORIENTED_EDGE ( 'NONE', *, *, #15514, .F. ) ;
#44577 = VECTOR ( 'NONE', #37130, 1000.000000000000000 ) ;
#44578 = ORIENTED_EDGE ( 'NONE', *, *, #34343, .F. ) ;
#44579 = CARTESIAN_POINT ( 'NONE',  ( 15.00000000000000000, 8.986842105263161073, -18.46084505325461578 ) ) ;
#44580 = CARTESIAN_POINT ( 'NONE',  ( -4.945973446814903696, 2.143131898507912917E-16, -80.93171244307204404 ) ) ;
#44581 = VERTEX_POINT ( 'NONE', #30643 ) ;
#44582 = CARTESIAN_POINT ( 'NONE',  ( 0.1287570809895660084, -0.3962735484563127408, 10.00000000000000000 ) ) ;
#44583 = CARTESIAN_POINT ( 'NONE',  ( 342.0000000000000568, 167.8284271247462129, 342.8284271247459287 ) ) ;
#44584 = EDGE_CURVE ( 'NONE', #21400, #46071, #19586, .T. ) ;
#44585 = CARTESIAN_POINT ( 'NONE',  ( -0.9601844228325777664, 0.8491947203466829741, 9.967237415621765351 ) ) ;
#44586 = EDGE_CURVE ( 'NONE', #40675, #49396, #14809, .T. ) ;
#44587 = CARTESIAN_POINT ( 'NONE',  ( 169.0000000000000000, -180.9999999999999716, -115.0000000000001279 ) ) ;
#44588 = ORIENTED_EDGE ( 'NONE', *, *, #27378, .T. ) ;
#44589 = DIRECTION ( 'NONE',  ( -1.000000000000000000, 0.000000000000000000, 1.860490536778032451E-50 ) ) ;
#44590 = ADVANCED_FACE ( 'NONE', ( #27300 ), #38351, .F. ) ;
#44591 = VECTOR ( 'NONE', #39127, 1000.000000000000000 ) ;
#44592 = EDGE_LOOP ( 'NONE', ( #4700, #4063, #2874, #50381 ) ) ;
#44593 = CARTESIAN_POINT ( 'NONE',  ( -7.721099712662037540, -1.750000000000022871, 1.843413822775074040 ) ) ;
#44594 = CYLINDRICAL_SURFACE ( 'NONE', #36816, 1.750000000000015543 ) ;
#44595 = EDGE_LOOP ( 'NONE', ( #45994, #27565, #26791, #5957, #22656, #26516 ) ) ;
#44596 = AXIS2_PLACEMENT_3D ( 'NONE', #34973, #19793, #11603 ) ;
#44597 = ORIENTED_EDGE ( 'NONE', *, *, #6729, .F. ) ;
#44598 = ORIENTED_EDGE ( 'NONE', *, *, #9208, .F. ) ;
#44599 = DIRECTION ( 'NONE',  ( 0.000000000000000000, 0.000000000000000000, -1.000000000000000000 ) ) ;
#44600 = CARTESIAN_POINT ( 'NONE',  ( 151.5540265531850537, 0.000000000000000000, 2.568287556927978166 ) ) ;
#44601 = ADVANCED_FACE ( 'NONE', ( #19337 ), #3162, .F. ) ;
#44602 = ORIENTED_EDGE ( 'NONE', *, *, #31640, .F. ) ;
#44603 = EDGE_CURVE ( 'NONE', #50662, #29288, #24005, .T. ) ;
#44604 = CARTESIAN_POINT ( 'NONE',  ( -1.186340292695371668, 0.3298841998003470555, 9.975326647350893694 ) ) ;
#44605 = CARTESIAN_POINT ( 'NONE',  ( 1.275927284277173834, -0.1224368140627448004, 9.976582533991679824 ) ) ;
#44606 = DIRECTION ( 'NONE',  ( -1.000000000000000000, 0.000000000000000000, 0.000000000000000000 ) ) ;
#44607 = EDGE_CURVE ( 'NONE', #1676, #37965, #1036, .T. ) ;
#44608 = EDGE_CURVE ( 'NONE', #21378, #22127, #14984, .T. ) ;
#44609 = ORIENTED_EDGE ( 'NONE', *, *, #23584, .F. ) ;
#44610 = VECTOR ( 'NONE', #21455, 1000.000000000000000 ) ;
#44611 = CARTESIAN_POINT ( 'NONE',  ( 210.0000000000000568, 0.000000000000000000, -157.4317124430720298 ) ) ;
#44612 = LINE ( 'NONE', #9241, #2168 ) ;
#44613 = EDGE_CURVE ( 'NONE', #43433, #32767, #11886, .T. ) ;
#44614 = CARTESIAN_POINT ( 'NONE',  ( 75.05402655318509630, 2.143131898507880377E-16, -117.4317124430720156 ) ) ;
#44615 = VERTEX_POINT ( 'NONE', #45990 ) ;
#44617 = B_SPLINE_CURVE_WITH_KNOTS ( 'NONE', 3,
 ( #43595, #4362, #35428, #20000 ),
 .UNSPECIFIED., .F., .F.,
 ( 4, 4 ),
 ( 0.000000000000000000, 0.002458791966311105019 ),
 .UNSPECIFIED. ) ;
#44616 = VECTOR ( 'NONE', #10384, 1000.000000000000000 ) ;
#44618 = ORIENTED_EDGE ( 'NONE', *, *, #18638, .F. ) ;
#44619 = PRODUCT_CONTEXT ( 'NONE', #21033, 'mechanical' ) ;
#44620 = CARTESIAN_POINT ( 'NONE',  ( 339.9999999999999432, -174.9999999999999432, 343.9999999999998295 ) ) ;
#44621 = PLANE ( 'NONE',  #14379 ) ;
#44622 = CARTESIAN_POINT ( 'NONE',  ( 1.275994128725544741, -0.1230186051320594776, 9.948547179989619238 ) ) ;
#44623 = DIRECTION ( 'NONE',  ( -1.000000000000000000, -0.000000000000000000, -0.000000000000000000 ) ) ;
#44624 = EDGE_LOOP ( 'NONE', ( #22272, #17318, #43984, #40046 ) ) ;
#44625 = CARTESIAN_POINT ( 'NONE',  ( 0.000000000000000000, 17.00000000000000000, 0.000000000000000000 ) ) ;
#44626 = CARTESIAN_POINT ( 'NONE',  ( 0.3862712429686894766, -1.188820645368940276, -10.00000000000000000 ) ) ;
#44627 = CARTESIAN_POINT ( 'NONE',  ( -4.999999999999979572, -6.505213034913003924E-16, 0.000000000000000000 ) ) ;
#44628 = EDGE_CURVE ( 'NONE', #7447, #37534, #23140, .T. ) ;
#44629 = DIRECTION ( 'NONE',  ( 1.333906992743555050E-23, -1.000000000000000000, 0.000000000000000000 ) ) ;
#44630 = VERTEX_POINT ( 'NONE', #7037 ) ;
#44631 = VECTOR ( 'NONE', #34794, 1000.000000000000000 ) ;
#44632 = EDGE_CURVE ( 'NONE', #76, #3380, #17174, .T. ) ;
#44633 = CARTESIAN_POINT ( 'NONE',  ( -168.4459734468149463, 0.000000000000000000, -40.93171244307202983 ) ) ;
#44634 = ORIENTED_EDGE ( 'NONE', *, *, #24300, .F. ) ;
#44635 = EDGE_CURVE ( 'NONE', #26837, #44023, #14775, .T. ) ;
#44636 = DIRECTION ( 'NONE',  ( -1.000000000000000000, 0.000000000000000000, 0.000000000000000000 ) ) ;
#44637 = AXIS2_PLACEMENT_3D ( 'NONE', #43832, #4824, #28200 ) ;
#44638 = ORIENTED_EDGE ( 'NONE', *, *, #41290, .T. ) ;
#44639 = CARTESIAN_POINT ( 'NONE',  ( 153.3040265531850537, 1.750000000000010658, 120.8182875569279702 ) ) ;
#44640 = EDGE_CURVE ( 'NONE', #835, #31251, #47005, .T. ) ;
#44641 = CARTESIAN_POINT ( 'NONE',  ( 340.0000000000000568, 167.0000000000000000, 355.9999999999997726 ) ) ;
#44642 = ORIENTED_EDGE ( 'NONE', *, *, #40051, .F. ) ;
#44643 = EDGE_CURVE ( 'NONE', #26888, #50033, #8292, .T. ) ;
#44644 =( GEOMETRIC_REPRESENTATION_CONTEXT ( 3 ) GLOBAL_UNCERTAINTY_ASSIGNED_CONTEXT ( ( #8706 ) ) GLOBAL_UNIT_ASSIGNED_CONTEXT ( ( #5214, #47269, #50411 ) ) REPRESENTATION_CONTEXT ( 'NONE', 'WORKASPACE' ) );
#44645 = DIRECTION ( 'NONE',  ( 0.000000000000000000, 0.000000000000000000, 1.000000000000000000 ) ) ;
#44646 = EDGE_LOOP ( 'NONE', ( #43454, #17372, #34084, #26629, #6533 ) ) ;
#44647 = LINE ( 'NONE', #9524, #24551 ) ;
#44648 = VECTOR ( 'NONE', #11774, 1000.000000000000000 ) ;
#44649 = CARTESIAN_POINT ( 'NONE',  ( 181.0000000000000000, -7.999999999999952038, 339.9999999999998295 ) ) ;
#44650 = AXIS2_PLACEMENT_3D ( 'NONE', #16367, #31785, #46868 ) ;
#44651 = CARTESIAN_POINT ( 'NONE',  ( 135.0000000000009663, 17.00000000000000000, -24.99999999999999289 ) ) ;
#44652 = VERTEX_POINT ( 'NONE', #50335 ) ;
#44653 = AXIS2_PLACEMENT_3D ( 'NONE', #3879, #16198, #11072 ) ;
#44654 = ORIENTED_EDGE ( 'NONE', *, *, #12308, .T. ) ;
#44655 = CARTESIAN_POINT ( 'NONE',  ( 210.0000000000000568, 0.000000000000000000, -119.1817124430720440 ) ) ;
#44656 = AXIS2_PLACEMENT_3D ( 'NONE', #33051, #8936, #44311 ) ;
#44657 = ORIENTED_EDGE ( 'NONE', *, *, #25612, .F. ) ;
#44658 = DIRECTION ( 'NONE',  ( -1.000000000000000000, -1.156482317317870492E-16, 0.000000000000000000 ) ) ;
#44659 = CARTESIAN_POINT ( 'NONE',  ( 32.57170742938662755, 18.58316106410423174, 7.697694107796188234 ) ) ;
#44660 =( BOUNDED_CURVE ( )  B_SPLINE_CURVE ( 3, ( #23315, #35149, #34931, #15622 ),
 .UNSPECIFIED., .F., .F. ) 
 B_SPLINE_CURVE_WITH_KNOTS ( ( 4, 4 ),
 ( 0.000000000000000000, 1.570796326794896558 ),
 .UNSPECIFIED. ) 
 CURVE ( )  GEOMETRIC_REPRESENTATION_ITEM ( )  RATIONAL_B_SPLINE_CURVE ( ( 1.000000000000000000, 0.8047378541243649375, 0.8047378541243649375, 1.000000000000000000 ) ) 
 REPRESENTATION_ITEM ( '' )  );
#44661 = ADVANCED_FACE ( 'NONE', ( #42929 ), #7808, .F. ) ;
#44662 = ORIENTED_EDGE ( 'NONE', *, *, #22908, .T. ) ;
#44663 = DIRECTION ( 'NONE',  ( -1.000000000000000000, 0.000000000000000000, 0.000000000000000000 ) ) ;
#44664 = CYLINDRICAL_SURFACE ( 'NONE', #44723, 1.750000000000001554 ) ;
#44665 = EDGE_LOOP ( 'NONE', ( #29804, #36950, #20902, #41763, #49940 ) ) ;
#44666 = CARTESIAN_POINT ( 'NONE',  ( 343.9999999999999432, -185.0000000000000284, 359.9999999999998295 ) ) ;
#44667 = PLANE ( 'NONE',  #12005 ) ;
#44668 = FACE_OUTER_BOUND ( 'NONE', #13098, .T. ) ;
#44669 = CARTESIAN_POINT ( 'NONE',  ( 74.32915281903215998, -1.750000000000009326, -158.1565861772249377 ) ) ;
#44670 = EDGE_CURVE ( 'NONE', #33964, #11965, #3018, .T. ) ;
#44671 = AXIS2_PLACEMENT_3D ( 'NONE', #25490, #21906, #41138 ) ;
#44673 = ORIENTED_EDGE ( 'NONE', *, *, #24389, .F. ) ;
#44672 = EDGE_CURVE ( 'NONE', #12712, #18308, #39765, .T. ) ;
#44674 = ORIENTED_EDGE ( 'NONE', *, *, #20465, .T. ) ;
#44675 = ORIENTED_EDGE ( 'NONE', *, *, #9663, .F. ) ;
#44676 = VECTOR ( 'NONE', #22972, 1000.000000000000000 ) ;
#44677 = DIRECTION ( 'NONE',  ( 0.000000000000000000, 0.000000000000000000, 1.000000000000000000 ) ) ;
#44678 = ADVANCED_FACE ( 'NONE', ( #1372 ), #32415, .T. ) ;
#44679 = CARTESIAN_POINT ( 'NONE',  ( 49.46074318306830975, -9.578883844006833570, 8.807470649214879543 ) ) ;
#44680 = CARTESIAN_POINT ( 'NONE',  ( 355.9999999999999432, -183.0000000000001421, -358.0000000000003411 ) ) ;
#44681 = EDGE_CURVE ( 'NONE', #44427, #18915, #20096, .T. ) ;
#44682 = VECTOR ( 'NONE', #7496, 1000.000000000000000 ) ;
#44683 = CARTESIAN_POINT ( 'NONE',  ( -4.763548243873389154, 16.57409059453848599, 8.727788335465566760 ) ) ;
#44684 = VERTEX_POINT ( 'NONE', #8312 ) ;
#44685 = B_SPLINE_CURVE_WITH_KNOTS ( 'NONE', 3,
 ( #20869, #23966, #47532, #1134 ),
 .UNSPECIFIED., .F., .F.,
 ( 4, 4 ),
 ( 0.7491799374948679979, 1.000000000000000000 ),
 .UNSPECIFIED. ) ;
#44686 = ADVANCED_FACE ( 'NONE', ( #364 ), #31674, .F. ) ;
#44687 = CARTESIAN_POINT ( 'NONE',  ( 210.0000000000000568, 2.143131898507876926E-16, -80.93171244307202983 ) ) ;
#44688 = ORIENTED_EDGE ( 'NONE', *, *, #50355, .F. ) ;
#44689 = CARTESIAN_POINT ( 'NONE',  ( 2.491056982571220768, -9.716321351877633461, 9.390253821402618328 ) ) ;
#44690 = VECTOR ( 'NONE', #217, 1000.000000000000000 ) ;
#44691 = CARTESIAN_POINT ( 'NONE',  ( 210.0000000000000568, 2.143131898507881856E-16, -80.93171244307202983 ) ) ;
#44692 = CARTESIAN_POINT ( 'NONE',  ( 240.0000000000000000, -164.9999999999999716, 474.9999999999998863 ) ) ;
#44693 = CARTESIAN_POINT ( 'NONE',  ( -210.0000000000000568, 0.000000000000000000, -79.18171244307201562 ) ) ;
#44694 = DIRECTION ( 'NONE',  ( -1.000000000000000000, 0.000000000000000000, -0.000000000000000000 ) ) ;
#44695 = CARTESIAN_POINT ( 'NONE',  ( 130.0000000000018474, 17.00000000000000000, 65.00000000000000000 ) ) ;
#44696 = ORIENTED_EDGE ( 'NONE', *, *, #26594, .F. ) ;
#44697 = FACE_OUTER_BOUND ( 'NONE', #5035, .T. ) ;
#44698 = DIRECTION ( 'NONE',  ( 1.000000000000000000, 0.000000000000000000, 0.000000000000000000 ) ) ;
#44699 = CARTESIAN_POINT ( 'NONE',  ( -0.3862712429686895876, 1.188820645368940720, 3.333333333333333481 ) ) ;
#44700 = AXIS2_PLACEMENT_3D ( 'NONE', #30193, #6594, #21992 ) ;
#44701 = VECTOR ( 'NONE', #10412, 1000.000000000000000 ) ;
#44702 = LINE ( 'NONE', #37807, #42764 ) ;
#44703 = ORIENTED_EDGE ( 'NONE', *, *, #40649, .T. ) ;
#44704 = ADVANCED_FACE ( 'NONE', ( #23951 ), #24718, .F. ) ;
#44705 = CARTESIAN_POINT ( 'NONE',  ( 165.0000000000000000, -93.50000000000005684, -115.0000000000001563 ) ) ;
#44706 = ORIENTED_EDGE ( 'NONE', *, *, #23029, .F. ) ;
#44707 = CARTESIAN_POINT ( 'NONE',  ( 341.9999999999999432, -171.9999999999999147, 346.9999999999998295 ) ) ;
#44708 = DIRECTION ( 'NONE',  ( -1.586032880504786307E-16, 1.654361225106055350E-24, -1.000000000000000000 ) ) ;
#44709 = PRODUCT_DEFINITION ( 'UNKNOWN', '', #36507, #8310 ) ;
#44710 = ORIENTED_EDGE ( 'NONE', *, *, #17733, .T. ) ;
#44711 = AXIS2_PLACEMENT_3D ( 'NONE', #48171, #36443, #26326 ) ;
#44712 = LINE ( 'NONE', #45202, #49148 ) ;
#44713 = CARTESIAN_POINT ( 'NONE',  ( -0.6679403265625625252, 1.504705676290988725, 9.936700280135882579 ) ) ;
#44714 = CIRCLE ( 'NONE', #33262, 1.880036658038868103 ) ;
#44715 = CARTESIAN_POINT ( 'NONE',  ( -0.3862712429686895876, 1.188820645368940720, 3.333333333333333481 ) ) ;
#44716 = CARTESIAN_POINT ( 'NONE',  ( -7.608425291889091113, 36.72004717559254772, 7.697694107796188234 ) ) ;
#44717 = EDGE_CURVE ( 'NONE', #20659, #22708, #47259, .T. ) ;
#44718 = ORIENTED_EDGE ( 'NONE', *, *, #11533, .T. ) ;
#44719 = ORIENTED_EDGE ( 'NONE', *, *, #13274, .T. ) ;
#44720 = CARTESIAN_POINT ( 'NONE',  ( -1.411185367335151541, -16.64174154430383012, -9.458680755252684591 ) ) ;
#44721 = CARTESIAN_POINT ( 'NONE',  ( -0.3862712429686977478, 1.188820645368937390, 3.333333333333333481 ) ) ;
#44722 =( BOUNDED_CURVE ( )  B_SPLINE_CURVE ( 3, ( #37237, #26407, #2060, #41806 ),
 .UNSPECIFIED., .F., .F. ) 
 B_SPLINE_CURVE_WITH_KNOTS ( ( 4, 4 ),
 ( 3.141592653589793116, 4.712388980384689674 ),
 .UNSPECIFIED. ) 
 CURVE ( )  GEOMETRIC_REPRESENTATION_ITEM ( )  RATIONAL_B_SPLINE_CURVE ( ( 1.000000000000000000, 0.8047378541243649375, 0.8047378541243649375, 1.000000000000000000 ) ) 
 REPRESENTATION_ITEM ( '' )  );
#44723 = AXIS2_PLACEMENT_3D ( 'NONE', #40351, #9051, #21340 ) ;
#44724 = ORIENTED_EDGE ( 'NONE', *, *, #4675, .F. ) ;
#44725 = VERTEX_POINT ( 'NONE', #12395 ) ;
#44726 = DIRECTION ( 'NONE',  ( 0.000000000000000000, 0.000000000000000000, -1.000000000000000000 ) ) ;
#44727 = LINE ( 'NONE', #1658, #20874 ) ;
#44728 = CARTESIAN_POINT ( 'NONE',  ( -168.4459734468149463, 0.000000000000000000, 159.0682875569279702 ) ) ;
#44729 = CARTESIAN_POINT ( 'NONE',  ( 80.00000000000216005, 17.00000000000000000, 95.00000000000000000 ) ) ;
#44730 = CIRCLE ( 'NONE', #40698, 10.00000000000000000 ) ;
#44731 = ORIENTED_EDGE ( 'NONE', *, *, #33478, .T. ) ;
#44732 = VERTEX_POINT ( 'NONE', #8562 ) ;
#44733 = ORIENTED_EDGE ( 'NONE', *, *, #36328, .T. ) ;
#44734 =( BOUNDED_CURVE ( )  B_SPLINE_CURVE ( 3, ( #41647, #50302, #49546, #6492 ),
 .UNSPECIFIED., .F., .F. ) 
 B_SPLINE_CURVE_WITH_KNOTS ( ( 4, 4 ),
 ( 0.000000000000000000, 1.570796326794896558 ),
 .UNSPECIFIED. ) 
 CURVE ( )  GEOMETRIC_REPRESENTATION_ITEM ( )  RATIONAL_B_SPLINE_CURVE ( ( 1.000000000000000000, 0.8047378541243649375, 0.8047378541243649375, 1.000000000000000000 ) ) 
 REPRESENTATION_ITEM ( '' )  );
#44735 = VECTOR ( 'NONE', #11566, 1000.000000000000000 ) ;
#44736 = DIRECTION ( 'NONE',  ( 0.000000000000000000, 0.000000000000000000, 1.000000000000000000 ) ) ;
#44737 = CARTESIAN_POINT ( 'NONE',  ( 193.3040265531851105, 1.750000000000010658, 120.8182875569279702 ) ) ;
#44738 = EDGE_CURVE ( 'NONE', #2035, #19349, #18749, .T. ) ;
#44739 = EDGE_CURVE ( 'NONE', #46959, #34536, #27560, .T. ) ;
#44740 = VERTEX_POINT ( 'NONE', #19836 ) ;
#44741 = ORIENTED_EDGE ( 'NONE', *, *, #16836, .F. ) ;
#44742 = CARTESIAN_POINT ( 'NONE',  ( -46.69597344681494633, -1.750000000000010214, -39.18171244307202983 ) ) ;
#44743 = CARTESIAN_POINT ( 'NONE',  ( -205.6708471809678827, -1.750000000000009326, 1.843413822775066269 ) ) ;
#44744 = EDGE_CURVE ( 'NONE', #37129, #38973, #2723, .T. ) ;
#44745 = VERTEX_POINT ( 'NONE', #9062 ) ;
#44746 = ORIENTED_EDGE ( 'NONE', *, *, #43451, .F. ) ;
#44747 = EDGE_CURVE ( 'NONE', #2022, #47416, #22334, .T. ) ;
#44748 = LINE ( 'NONE', #6779, #44616 ) ;
#44749 = DIRECTION ( 'NONE',  ( -0.000000000000000000, -0.000000000000000000, -1.000000000000000000 ) ) ;
#44750 = ORIENTED_EDGE ( 'NONE', *, *, #36211, .F. ) ;
#44751 = EDGE_CURVE ( 'NONE', #12843, #23977, #5206, .T. ) ;
#44752 = CARTESIAN_POINT ( 'NONE',  ( 151.5540265531850537, 0.000000000000000000, 122.5682875569279702 ) ) ;
#44753 = DIRECTION ( 'NONE',  ( 0.000000000000000000, 0.000000000000000000, 1.000000000000000000 ) ) ;
#44754 = DIRECTION ( 'NONE',  ( 0.000000000000000000, -2.265761274745217480E-16, 1.000000000000000000 ) ) ;
#44755 = DIRECTION ( 'NONE',  ( 0.000000000000000000, -1.000000000000000000, 0.000000000000000000 ) ) ;
#44756 = VECTOR ( 'NONE', #32392, 1000.000000000000000 ) ;
#44757 = CARTESIAN_POINT ( 'NONE',  ( 151.5540265531850537, -1.025126265847089435, 2.568287556927986159 ) ) ;
#44758 = VECTOR ( 'NONE', #43122, 1000.000000000000000 ) ;
#44759 = ORIENTED_EDGE ( 'NONE', *, *, #42108, .F. ) ;
#44760 = CARTESIAN_POINT ( 'NONE',  ( -1.011271242968683426, -0.7347315653655928092, 10.00000000000000000 ) ) ;
#44761 = CARTESIAN_POINT ( 'NONE',  ( 47.88254548617766204, -14.43607691413525984, -3.760136334089591248 ) ) ;
#44762 = EDGE_CURVE ( 'NONE', #16264, #40358, #32875, .T. ) ;
#44763 = DIRECTION ( 'NONE',  ( -1.000000000000000000, -0.000000000000000000, -0.000000000000000000 ) ) ;
#44764 = CARTESIAN_POINT ( 'NONE',  ( -50.00000000000000000, -50.00000000000000000, 800.0000000000000000 ) ) ;
#44765 = VECTOR ( 'NONE', #3096, 1000.000000000000000 ) ;
#44766 = DIRECTION ( 'NONE',  ( -1.000000000000000000, 0.000000000000000000, 0.000000000000000000 ) ) ;
#44767 = CARTESIAN_POINT ( 'NONE',  ( 164.9999999999999716, -164.9999999999999432, -356.0000000000001705 ) ) ;
#44768 = LINE ( 'NONE', #38370, #4083 ) ;
#44769 = LINE ( 'NONE', #28394, #23870 ) ;
#44770 = VECTOR ( 'NONE', #7916, 1000.000000000000000 ) ;
#44771 = EDGE_LOOP ( 'NONE', ( #39869, #23696, #32887, #18900 ) ) ;
#44772 = PLANE ( 'NONE',  #27302 ) ;
#44773 = CARTESIAN_POINT ( 'NONE',  ( -48.33712804702535948, -13.03701565032741527, -9.367992836599954742 ) ) ;
#44774 = DIRECTION ( 'NONE',  ( -1.000000000000000000, 0.000000000000000000, 0.000000000000000000 ) ) ;
#44775 = CARTESIAN_POINT ( 'NONE',  ( 6.174150299305392053, -45.68101107938186800, 8.807470649214879543 ) ) ;
#44776 = DIRECTION ( 'NONE',  ( 0.000000000000000000, 0.000000000000000000, 1.000000000000000000 ) ) ;
#44777 = ORIENTED_EDGE ( 'NONE', *, *, #19260, .T. ) ;
#44778 = DIRECTION ( 'NONE',  ( 0.000000000000000000, 1.000000000000000000, 6.938893903907222067E-15 ) ) ;
#44779 = ORIENTED_EDGE ( 'NONE', *, *, #31009, .F. ) ;
#44780 = CARTESIAN_POINT ( 'NONE',  ( -34.08355720199904226, 2.371364769369340042, 7.455576670931136185 ) ) ;
#44781 = B_SPLINE_CURVE_WITH_KNOTS ( 'NONE', 3,
 ( #13967, #2431, #29881, #25275 ),
 .UNSPECIFIED., .F., .F.,
 ( 4, 4 ),
 ( 2.680765238357722860E-17, 0.0004072981213157027118 ),
 .UNSPECIFIED. ) ;
#44782 = EDGE_CURVE ( 'NONE', #19656, #10604, #44957, .T. ) ;
#44783 = CARTESIAN_POINT ( 'NONE',  ( 111.5540265531850537, -1.025126265847081886, 119.0682875569279702 ) ) ;
#44784 = AXIS2_PLACEMENT_3D ( 'NONE', #31777, #12014, #4059 ) ;
#44785 = ORIENTED_EDGE ( 'NONE', *, *, #43896, .F. ) ;
#44786 = DIRECTION ( 'NONE',  ( -0.000000000000000000, -0.000000000000000000, 1.000000000000000000 ) ) ;
#44787 = DIRECTION ( 'NONE',  ( 0.000000000000000000, 0.000000000000000000, -1.000000000000000000 ) ) ;
#44788 = ORIENTED_EDGE ( 'NONE', *, *, #28012, .T. ) ;
#44789 = ORIENTED_EDGE ( 'NONE', *, *, #8698, .T. ) ;
#44790 = B_SPLINE_CURVE_WITH_KNOTS ( 'NONE', 3,
 ( #43952, #48268, #24475, #36290, #20864, #4955 ),
 .UNSPECIFIED., .F., .F.,
 ( 4, 2, 4 ),
 ( 4.635316164197443437E-17, 0.009882509389272372408, 0.01976501877854469624 ),
 .UNSPECIFIED. ) ;
#44791 = CARTESIAN_POINT ( 'NONE',  ( -1.249999999999999778, 0.000000000000000000, 3.333333333333333481 ) ) ;
#44792 = CARTESIAN_POINT ( 'NONE',  ( -208.4459734468149463, 0.000000000000000000, -120.9317124430720156 ) ) ;
#44793 = CARTESIAN_POINT ( 'NONE',  ( -5.888214538810513154, -16.20866436362413410, 8.727788335465566760 ) ) ;
#44794 = ORIENTED_EDGE ( 'NONE', *, *, #7758, .F. ) ;
#44795 = ADVANCED_FACE ( 'NONE', ( #43196 ), #17261, .F. ) ;
#44796 = CARTESIAN_POINT ( 'NONE',  ( 341.9999999999999432, 175.0000000000000284, -106.0000000000001990 ) ) ;
#44797 = EDGE_CURVE ( 'NONE', #43553, #40295, #14717, .T. ) ;
#44798 = CARTESIAN_POINT ( 'NONE',  ( 0.000000000000000000, 181.0000000000000284, 339.9999999999997726 ) ) ;
#44799 = CARTESIAN_POINT ( 'NONE',  ( 73.30402655318508209, 0.000000000000000000, 165.0000000000000000 ) ) ;
#44800 = ORIENTED_EDGE ( 'NONE', *, *, #21037, .T. ) ;
#44801 = ORIENTED_EDGE ( 'NONE', *, *, #8392, .T. ) ;
#44802 = EDGE_LOOP ( 'NONE', ( #35368, #27573, #9111, #48219 ) ) ;
#44803 = DIRECTION ( 'NONE',  ( -1.000000000000000000, 0.000000000000000000, 0.000000000000000000 ) ) ;
#44804 = DIRECTION ( 'NONE',  ( 0.6805276818820472640, -0.4944323023721970412, 0.5407575913134972101 ) ) ;
#44805 = ORIENTED_EDGE ( 'NONE', *, *, #8468, .F. ) ;
#44806 = VECTOR ( 'NONE', #3925, 1000.000000000000000 ) ;
#44807 = EDGE_CURVE ( 'NONE', #30535, #15604, #37539, .T. ) ;
#44808 = CARTESIAN_POINT ( 'NONE',  ( -207.7210997126620384, -1.750000000000010214, -118.1565861772249519 ) ) ;
#44809 = CARTESIAN_POINT ( 'NONE',  ( -207.7210997126620384, -1.750000000000009548, 39.79316129108089228 ) ) ;
#44810 = ADVANCED_FACE ( 'NONE', ( #14147 ), #22116, .T. ) ;
#44811 = DIRECTION ( 'NONE',  ( -0.000000000000000000, -0.000000000000000000, -1.000000000000000000 ) ) ;
#44812 = CARTESIAN_POINT ( 'NONE',  ( 71.55402655318505367, 1.025126265847089213, 42.56828755692799149 ) ) ;
#44813 = CYLINDRICAL_SURFACE ( 'NONE', #36416, 3.749999999999975575 ) ;
#44815 = ADVANCED_FACE ( 'NONE', ( #44924 ), #10326, .T. ) ;
#44814 = CARTESIAN_POINT ( 'NONE',  ( 2.500000000000051070, -214.9999999999999716, -234.7500000000000000 ) ) ;
#44816 = LINE ( 'NONE', #48390, #5381 ) ;
#44817 = CARTESIAN_POINT ( 'NONE',  ( 210.0000000000000568, 0.000000000000000000, 120.8182875569279702 ) ) ;
#44818 = CARTESIAN_POINT ( 'NONE',  ( -10.70590866674912967, 12.76446523155714985, -3.546734833711462365 ) ) ;
#44819 = CIRCLE ( 'NONE', #47268, 5.000000000000000000 ) ;
#44820 = CARTESIAN_POINT ( 'NONE',  ( 1.011271242968683648, 0.7347315653655930312, 10.00000000000000000 ) ) ;
#44821 = ORIENTED_EDGE ( 'NONE', *, *, #43078, .F. ) ;
#44822 = LINE ( 'NONE', #13537, #25362 ) ;
#44823 = LINE ( 'NONE', #44321, #16000 ) ;
#44824 = CARTESIAN_POINT ( 'NONE',  ( 30.00000000000062172, 16.00000000000000000, -54.99999999999999289 ) ) ;
#44825 = ORIENTED_EDGE ( 'NONE', *, *, #29716, .F. ) ;
#44826 =( NAMED_UNIT ( * ) SI_UNIT ( $, .STERADIAN. ) SOLID_ANGLE_UNIT ( ) );
#44827 = DIRECTION ( 'NONE',  ( -1.000000000000000000, 0.000000000000000000, 0.000000000000000000 ) ) ;
#44828 = ORIENTED_EDGE ( 'NONE', *, *, #8935, .F. ) ;
#44829 = LINE ( 'NONE', #48907, #14803 ) ;
#44830 = DIRECTION ( 'NONE',  ( 0.000000000000000000, -1.000000000000000000, 1.604368532695312981E-16 ) ) ;
#44831 = CARTESIAN_POINT ( 'NONE',  ( 193.3040265531851105, 1.750000000000010658, 120.8182875569279702 ) ) ;
#44832 = ORIENTED_EDGE ( 'NONE', *, *, #35030, .F. ) ;
#44833 = CARTESIAN_POINT ( 'NONE',  ( 33.30402655318503946, -1.750000000000010658, -119.1817124430720440 ) ) ;
#44834 = ORIENTED_EDGE ( 'NONE', *, *, #43237, .T. ) ;
#44835 = ORIENTED_EDGE ( 'NONE', *, *, #9100, .T. ) ;
#44836 = EDGE_CURVE ( 'NONE', #19934, #50192, #6223, .T. ) ;
#44837 = LINE ( 'NONE', #23420, #37713 ) ;
#44838 = ORIENTED_EDGE ( 'NONE', *, *, #3049, .F. ) ;
#44839 = CARTESIAN_POINT ( 'NONE',  ( -70.00000000000002842, 17.00000000000000000, -90.00000000000000000 ) ) ;
#44840 = DIRECTION ( 'NONE',  ( 0.000000000000000000, 0.000000000000000000, -1.000000000000000000 ) ) ;
#44841 = ORIENTED_EDGE ( 'NONE', *, *, #43479, .T. ) ;
#44842 = CARTESIAN_POINT ( 'NONE',  ( 355.9999999999999432, 183.0000000000002558, -358.0000000000003411 ) ) ;
#44843 = CARTESIAN_POINT ( 'NONE',  ( 339.9999999999999432, -180.9999999999999716, -344.0000000000001705 ) ) ;
#44844 = DIRECTION ( 'NONE',  ( 1.132880637372608740E-16, 4.718402560806925739E-50, 1.000000000000000000 ) ) ;
#44845 = CARTESIAN_POINT ( 'NONE',  ( 164.9999999999999716, -272.5000000000000000, -110.9999999999999005 ) ) ;
#44846 = ORIENTED_EDGE ( 'NONE', *, *, #41866, .F. ) ;
#44847 = DIRECTION ( 'NONE',  ( 0.000000000000000000, 5.664403186863042467E-17, 1.000000000000000000 ) ) ;
#44848 = ORIENTED_EDGE ( 'NONE', *, *, #37611, .F. ) ;
#44849 = VECTOR ( 'NONE', #1123, 1000.000000000000000 ) ;
#44850 = LINE ( 'NONE', #36450, #43127 ) ;
#44851 = PLANE ( 'NONE',  #7303 ) ;
#44852 = ORIENTED_EDGE ( 'NONE', *, *, #15821, .T. ) ;
#44853 = ORIENTED_EDGE ( 'NONE', *, *, #23673, .T. ) ;
#44854 = VERTEX_POINT ( 'NONE', #2600 ) ;
#44855 = CARTESIAN_POINT ( 'NONE',  ( -164.9459734468149463, 2.143131898507880377E-16, -157.4317124430720582 ) ) ;
#44856 = CARTESIAN_POINT ( 'NONE',  ( -7.608425291889091113, 36.72004717559254772, 7.697694107796188234 ) ) ;
#44857 = ORIENTED_EDGE ( 'NONE', *, *, #21901, .F. ) ;
#44858 = CARTESIAN_POINT ( 'NONE',  ( 2.500000000000050182, -204.9999999999999716, -230.2499999999999716 ) ) ;
#44859 = CARTESIAN_POINT ( 'NONE',  ( 1.142975459103954705, 16.61830776097024653, -2.870787844569587133 ) ) ;
#44860 =( BOUNDED_CURVE ( )  B_SPLINE_CURVE ( 3, ( #27590, #28333, #8836, #44216 ),
 .UNSPECIFIED., .F., .F. ) 
 B_SPLINE_CURVE_WITH_KNOTS ( ( 4, 4 ),
 ( 3.141592653589793116, 4.712388980384689674 ),
 .UNSPECIFIED. ) 
 CURVE ( )  GEOMETRIC_REPRESENTATION_ITEM ( )  RATIONAL_B_SPLINE_CURVE ( ( 1.000000000000000000, 0.8047378541243649375, 0.8047378541243649375, 1.000000000000000000 ) ) 
 REPRESENTATION_ITEM ( '' )  );
#44861 = LINE ( 'NONE', #17928, #42757 ) ;
#44862 = ORIENTED_EDGE ( 'NONE', *, *, #49313, .T. ) ;
#44863 = DIRECTION ( 'NONE',  ( 0.000000000000000000, 0.000000000000000000, -1.000000000000000000 ) ) ;
#44865 = EDGE_CURVE ( 'NONE', #36589, #18600, #46598, .T. ) ;
#44864 = LINE ( 'NONE', #5894, #5445 ) ;
#44866 =( BOUNDED_CURVE ( )  B_SPLINE_CURVE ( 3, ( #34430, #41857, #50008, #7220 ),
 .UNSPECIFIED., .F., .F. ) 
 B_SPLINE_CURVE_WITH_KNOTS ( ( 4, 4 ),
 ( 1.570796326794896558, 3.141592653589793116 ),
 .UNSPECIFIED. ) 
 CURVE ( )  GEOMETRIC_REPRESENTATION_ITEM ( )  RATIONAL_B_SPLINE_CURVE ( ( 1.000000000000000000, 0.8047378541243649375, 0.8047378541243649375, 1.000000000000000000 ) ) 
 REPRESENTATION_ITEM ( '' )  );
#44867 = VECTOR ( 'NONE', #42426, 1000.000000000000000 ) ;
#44868 = CARTESIAN_POINT ( 'NONE',  ( -31.28234235046239320, -11.28615439405757392, -3.760136334089591248 ) ) ;
#44869 = ORIENTED_EDGE ( 'NONE', *, *, #30408, .T. ) ;
#44870 = CONTEXT_DEPENDENT_SHAPE_REPRESENTATION ( #7313, #7319 ) ;
#44871 = DIRECTION ( 'NONE',  ( -0.000000000000000000, -0.000000000000000000, -1.000000000000000000 ) ) ;
#44872 = CARTESIAN_POINT ( 'NONE',  ( 339.9999999999999432, -166.9999999999999432, -356.0000000000002274 ) ) ;
#44873 = CARTESIAN_POINT ( 'NONE',  ( -30.25247992116029394, 39.82368563463828792, -3.760136334089591248 ) ) ;
#44874 = CYLINDRICAL_SURFACE ( 'NONE', #43693, 1.750000000000008438 ) ;
#44875 = VERTEX_POINT ( 'NONE', #25978 ) ;
#44876 = DIRECTION ( 'NONE',  ( 0.000000000000000000, -0.000000000000000000, -1.000000000000000000 ) ) ;
#44877 = CARTESIAN_POINT ( 'NONE',  ( 14.48769039275578407, 30.44468701195595983, 8.807470649214879543 ) ) ;
#44878 =( BOUNDED_CURVE ( )  B_SPLINE_CURVE ( 3, ( #45058, #48887, #5578, #29198 ),
 .UNSPECIFIED., .F., .F. ) 
 B_SPLINE_CURVE_WITH_KNOTS ( ( 4, 4 ),
 ( 0.000000000000000000, 1.570796326794896558 ),
 .UNSPECIFIED. ) 
 CURVE ( )  GEOMETRIC_REPRESENTATION_ITEM ( )  RATIONAL_B_SPLINE_CURVE ( ( 1.000000000000000000, 0.8047378541243649375, 0.8047378541243649375, 1.000000000000000000 ) ) 
 REPRESENTATION_ITEM ( '' )  );
#44879 = CARTESIAN_POINT ( 'NONE',  ( -45.67084718096785423, 1.750000000000009548, -158.1565861772249377 ) ) ;
#44880 = DIRECTION ( 'NONE',  ( 0.000000000000000000, 0.000000000000000000, -1.000000000000000000 ) ) ;
#44882 = EDGE_CURVE ( 'NONE', #27106, #30474, #25266, .T. ) ;
#44881 = DIRECTION ( 'NONE',  ( 0.000000000000000000, 0.000000000000000000, 1.000000000000000000 ) ) ;
#44883 = B_SPLINE_CURVE_WITH_KNOTS ( 'NONE', 3,
 ( #9045, #24196, #20332, #24700 ),
 .UNSPECIFIED., .F., .F.,
 ( 4, 4 ),
 ( 0.0001349653321192963314, 0.009897389366564843943 ),
 .UNSPECIFIED. ) ;
#44884 = ORIENTED_EDGE ( 'NONE', *, *, #36055, .T. ) ;
#44885 = LINE ( 'NONE', #36747, #1039 ) ;
#44887 = ORIENTED_EDGE ( 'NONE', *, *, #14838, .F. ) ;
#44886 = VECTOR ( 'NONE', #28939, 1000.000000000000000 ) ;
#44888 = CARTESIAN_POINT ( 'NONE',  ( -4.945973446814917018, 1.025126265847097207, 159.0682875569279418 ) ) ;
#44889 = VERTEX_POINT ( 'NONE', #40617 ) ;
#44890 = DIRECTION ( 'NONE',  ( 1.000000000000000000, 0.000000000000000000, -9.251858538542979716E-16 ) ) ;
#44891 = CARTESIAN_POINT ( 'NONE',  ( 35.05402655318504657, 2.143131898507880377E-16, 79.06828755692797017 ) ) ;
#44892 = VERTEX_POINT ( 'NONE', #29558 ) ;
#44893 = LINE ( 'NONE', #37264, #41704 ) ;
#44894 = EDGE_LOOP ( 'NONE', ( #29711, #35384, #45614, #5, #28298, #28922 ) ) ;
#44895 = CARTESIAN_POINT ( 'NONE',  ( 151.5540265531850537, -1.025126265847089213, -160.9317124430720014 ) ) ;
#44896 = CARTESIAN_POINT ( 'NONE',  ( 341.6568542494924259, 165.0000000000000000, 339.9999999999998295 ) ) ;
#44897 = PLANE ( 'NONE',  #37729 ) ;
#44898 = CARTESIAN_POINT ( 'NONE',  ( -47.72109971266203132, -1.750000000000009548, -40.20683870891912193 ) ) ;
#44899 = CARTESIAN_POINT ( 'NONE',  ( 85.00000000000213163, 17.00000000000000000, 95.00000000000000000 ) ) ;
#44900 = ORIENTED_EDGE ( 'NONE', *, *, #7616, .F. ) ;
#44901 = ORIENTED_EDGE ( 'NONE', *, *, #15196, .T. ) ;
#44902 = CARTESIAN_POINT ( 'NONE',  ( 73.30402655318508209, 0.000000000000000000, -165.0000000000000000 ) ) ;
#44903 = VERTEX_POINT ( 'NONE', #44433 ) ;
#44904 = FACE_OUTER_BOUND ( 'NONE', #47735, .T. ) ;
#44905 = CARTESIAN_POINT ( 'NONE',  ( -128.4459734468149179, 0.000000000000000000, 122.5682875569279418 ) ) ;
#44906 = ORIENTED_EDGE ( 'NONE', *, *, #12856, .F. ) ;
#44907 = CARTESIAN_POINT ( 'NONE',  ( 177.5000000000000284, 112.5000000000000000, -10.00000000000000000 ) ) ;
#44908 = CARTESIAN_POINT ( 'NONE',  ( -166.6959734468149463, 1.750000000000009992, 0.8182875569279768335 ) ) ;
#44909 = ORIENTED_EDGE ( 'NONE', *, *, #21122, .T. ) ;
#44910 = CARTESIAN_POINT ( 'NONE',  ( 167.0000000000000000, -174.9999999999999716, -111.0000000000001563 ) ) ;
#44911 = CARTESIAN_POINT ( 'NONE',  ( 185.0000000000000000, -184.9999999999999716, -344.0000000000001137 ) ) ;
#44912 = CARTESIAN_POINT ( 'NONE',  ( 35.00000000000152767, 17.00000000000000000, 60.00000000000000000 ) ) ;
#44913 = CARTESIAN_POINT ( 'NONE',  ( 1.228394325311184421, -1.341866297401743235, 9.903764339332088440 ) ) ;
#44914 = ORIENTED_EDGE ( 'NONE', *, *, #27720, .F. ) ;
#44915 = VECTOR ( 'NONE', #32501, 1000.000000000000000 ) ;
#44916 = ADVANCED_FACE ( 'NONE', ( #13399 ), #6050, .T. ) ;
#44917 = ORIENTED_EDGE ( 'NONE', *, *, #1503, .T. ) ;
#44918 =( BOUNDED_CURVE ( )  B_SPLINE_CURVE ( 3, ( #44370, #28750, #4646, #9240 ),
 .UNSPECIFIED., .F., .F. ) 
 B_SPLINE_CURVE_WITH_KNOTS ( ( 4, 4 ),
 ( 0.000000000000000000, 1.570796326794896558 ),
 .UNSPECIFIED. ) 
 CURVE ( )  GEOMETRIC_REPRESENTATION_ITEM ( )  RATIONAL_B_SPLINE_CURVE ( ( 1.000000000000000000, 0.8047378541243649375, 0.8047378541243649375, 1.000000000000000000 ) ) 
 REPRESENTATION_ITEM ( '' )  );
#44919 = DIRECTION ( 'NONE',  ( 1.000000000000000000, 0.000000000000000000, 0.000000000000000000 ) ) ;
#44920 = CARTESIAN_POINT ( 'NONE',  ( -87.72109971266203843, -1.750000000000010214, 81.84341382277507648 ) ) ;
#44922 = ADVANCED_FACE ( 'NONE', ( #1869 ), #13660, .T. ) ;
#44921 = CARTESIAN_POINT ( 'NONE',  ( 16.52264463346132572, -2.779753662172757878, 9.403735324607438884 ) ) ;
#44923 = CARTESIAN_POINT ( 'NONE',  ( -126.6959734468149321, -1.749999999999996891, 0.8182875569279768335 ) ) ;
#44924 = FACE_OUTER_BOUND ( 'NONE', #26369, .T. ) ;
#44925 = EDGE_LOOP ( 'NONE', ( #26617, #45066, #20852, #28753 ) ) ;
#44926 = EDGE_CURVE ( 'NONE', #17677, #13610, #5927, .T. ) ;
#44927 = DIRECTION ( 'NONE',  ( -1.000000000000000000, 0.000000000000000000, -1.612977847700450206E-50 ) ) ;
#44928 = ORIENTED_EDGE ( 'NONE', *, *, #39938, .F. ) ;
#44929 =( NAMED_UNIT ( * ) SI_UNIT ( $, .STERADIAN. ) SOLID_ANGLE_UNIT ( ) );
#44930 = EDGE_CURVE ( 'NONE', #3579, #37204, #30511, .T. ) ;
#44931 = CARTESIAN_POINT ( 'NONE',  ( 177.5000000000000284, -102.5000000000000142, -10.00000000000000000 ) ) ;
#44932 = CARTESIAN_POINT ( 'NONE',  ( 0.000000000000000000, -168.9999999999999432, -340.0000000000001705 ) ) ;
#44933 = CARTESIAN_POINT ( 'NONE',  ( -4.945973446814916130, -1.025126265847097429, 119.0682875569279133 ) ) ;
#44934 = CYLINDRICAL_SURFACE ( 'NONE', #33235, 1.750000000000008438 ) ;
#44935 = DIRECTION ( 'NONE',  ( -1.000000000000000000, 0.000000000000000000, -0.000000000000000000 ) ) ;
#44936 = CARTESIAN_POINT ( 'NONE',  ( 181.0000000000000000, -272.5000000000000000, -94.99999999999988631 ) ) ;
#44937 = ORIENTED_EDGE ( 'NONE', *, *, #24635, .T. ) ;
#44938 = CARTESIAN_POINT ( 'NONE',  ( -0.9494396179258391966, 9.954826186926261755, 9.646707543097345905 ) ) ;
#44939 = PRODUCT ( 'hopper', 'hopper', '', ( #12582 ) ) ;
#44940 = CARTESIAN_POINT ( 'NONE',  ( -65.00000000000002842, 17.00000000000000000, -114.9999999999999858 ) ) ;
#44941 = CARTESIAN_POINT ( 'NONE',  ( -45.64490844644706868, -21.32281559348764333, 8.807470649214879543 ) ) ;
#44942 = CARTESIAN_POINT ( 'NONE',  ( -124.9459734468149463, 2.143131898507847836E-16, 2.568287556927950632 ) ) ;
#44943 = VERTEX_POINT ( 'NONE', #45931 ) ;
#44944 = CYLINDRICAL_SURFACE ( 'NONE', #19603, 4.000000000000003553 ) ;
#44945 = EDGE_LOOP ( 'NONE', ( #12314, #12565, #40338, #23774 ) ) ;
#44946 = CARTESIAN_POINT ( 'NONE',  ( 15.00000000000000000, -46.51315789473684248, -5.916985404131818171 ) ) ;
#44947 = LINE ( 'NONE', #41132, #43826 ) ;
#44948 = EDGE_CURVE ( 'NONE', #5026, #28864, #49765, .T. ) ;
#44949 = PLANE ( 'NONE',  #46776 ) ;
#44950 = EDGE_CURVE ( 'NONE', #19018, #3156, #45681, .T. ) ;
#44951 = VECTOR ( 'NONE', #47581, 1000.000000000000000 ) ;
#44952 = ADVANCED_FACE ( 'NONE', ( #23121 ), #40460, .T. ) ;
#44953 = EDGE_CURVE ( 'NONE', #3827, #19026, #36295, .T. ) ;
#44954 = VECTOR ( 'NONE', #32056, 1000.000000000000000 ) ;
#44955 = CARTESIAN_POINT ( 'NONE',  ( 30.87089393895375267, -12.69923079256617093, -9.367992836599951190 ) ) ;
#44956 = CARTESIAN_POINT ( 'NONE',  ( 1.011271242968694084, -0.7347315653655782652, 3.333333333333333481 ) ) ;
#44957 =( BOUNDED_CURVE ( )  B_SPLINE_CURVE ( 3, ( #39364, #17765, #37299, #2121 ),
 .UNSPECIFIED., .F., .F. ) 
 B_SPLINE_CURVE_WITH_KNOTS ( ( 4, 4 ),
 ( 0.000000000000000000, 1.570796326794896558 ),
 .UNSPECIFIED. ) 
 CURVE ( )  GEOMETRIC_REPRESENTATION_ITEM ( )  RATIONAL_B_SPLINE_CURVE ( ( 1.000000000000000000, 0.8047378541243649375, 0.8047378541243649375, 1.000000000000000000 ) ) 
 REPRESENTATION_ITEM ( '' )  );
#44958 = CARTESIAN_POINT ( 'NONE',  ( 21.23829395927641883, 2.683863964738837371, 229.0000000000000000 ) ) ;
#44959 = VECTOR ( 'NONE', #28485, 1000.000000000000000 ) ;
#44960 = EDGE_CURVE ( 'NONE', #1207, #47828, #34438, .T. ) ;
#44961 = CARTESIAN_POINT ( 'NONE',  ( -5.670847180967843570, -1.750000000000022427, 1.843413822775074040 ) ) ;
#44962 = EDGE_CURVE ( 'NONE', #8293, #50401, #2847, .T. ) ;
#44963 = ORIENTED_EDGE ( 'NONE', *, *, #32628, .F. ) ;
#44964 = CIRCLE ( 'NONE', #3184, 2.000000000000001776 ) ;
#44965 = VERTEX_POINT ( 'NONE', #34188 ) ;
#44966 = FACE_OUTER_BOUND ( 'NONE', #14393, .T. ) ;
#44967 = CARTESIAN_POINT ( 'NONE',  ( 185.0000000000000000, -268.4999999999999432, -339.9999999999998863 ) ) ;
#44968 = VECTOR ( 'NONE', #14573, 1000.000000000000000 ) ;
#44969 = ORIENTED_EDGE ( 'NONE', *, *, #3434, .F. ) ;
#44970 = VERTEX_POINT ( 'NONE', #26730 ) ;
#44971 = DIRECTION ( 'NONE',  ( 1.000000000000000000, 0.000000000000000000, 0.000000000000000000 ) ) ;
#44972 = CARTESIAN_POINT ( 'NONE',  ( 183.0000000000000000, -268.4999999999999432, -349.9999999999999432 ) ) ;
#44973 = CARTESIAN_POINT ( 'NONE',  ( -204.9459734468148895, 1.025126265847089657, 79.06828755692797017 ) ) ;
#44974 = CARTESIAN_POINT ( 'NONE',  ( -5.000000000000000000, 0.000000000000000000, 0.000000000000000000 ) ) ;
#44975 =( REPRESENTATION_RELATIONSHIP ('NONE','NONE', #45699, #8742 ) REPRESENTATION_RELATIONSHIP_WITH_TRANSFORMATION ( #34133 )SHAPE_REPRESENTATION_RELATIONSHIP( ) );
#44976 = EDGE_LOOP ( 'NONE', ( #34561, #10683, #16215, #14397 ) ) ;
#44977 = VERTEX_POINT ( 'NONE', #46437 ) ;
#44978 = EDGE_CURVE ( 'NONE', #50236, #25157, #14665, .T. ) ;
#44979 = CARTESIAN_POINT ( 'NONE',  ( -128.4459734468149463, -1.025126265847082108, -37.43171244307203693 ) ) ;
#44980 = DIRECTION ( 'NONE',  ( -1.000000000000000000, -0.000000000000000000, -0.000000000000000000 ) ) ;
#44981 = EDGE_CURVE ( 'NONE', #8966, #22583, #22077, .T. ) ;
#44982 = EDGE_CURVE ( 'NONE', #42338, #16052, #11068, .T. ) ;
#44983 = VERTEX_POINT ( 'NONE', #7741 ) ;
#44984 = ORIENTED_EDGE ( 'NONE', *, *, #8618, .T. ) ;
#44985 = DIRECTION ( 'NONE',  ( -1.000000000000000000, 0.000000000000000000, -0.000000000000000000 ) ) ;
#44986 = LINE ( 'NONE', #18064, #1136 ) ;
#44987 = ORIENTED_EDGE ( 'NONE', *, *, #30744, .F. ) ;
#44988 = ORIENTED_EDGE ( 'NONE', *, *, #21454, .F. ) ;
#44989 = FACE_OUTER_BOUND ( 'NONE', #27467, .T. ) ;
#44991 = ORIENTED_EDGE ( 'NONE', *, *, #27165, .T. ) ;
#44990 = AXIS2_PLACEMENT_3D ( 'NONE', #27888, #4772, #49347 ) ;
#44992 = CARTESIAN_POINT ( 'NONE',  ( 7.576114424932982594, -50.00000000000000711, 7.906207997025717304 ) ) ;
#44993 = CARTESIAN_POINT ( 'NONE',  ( 35.05402655318504657, 2.143131898507882349E-16, -165.0000000000000000 ) ) ;
#44994 = CARTESIAN_POINT ( 'NONE',  ( 164.9999999999999716, 17.00000000000000000, -25.00000000000000711 ) ) ;
#44995 = CARTESIAN_POINT ( 'NONE',  ( -164.9999999999981526, 17.00000000000000000, 65.00000000000000000 ) ) ;
#44996 = VECTOR ( 'NONE', #46706, 1000.000000000000000 ) ;
#44997 = DIRECTION ( 'NONE',  ( 1.000000000000000000, 0.000000000000000000, 0.000000000000000000 ) ) ;
#44998 = ORIENTED_EDGE ( 'NONE', *, *, #18646, .T. ) ;
#44999 = VECTOR ( 'NONE', #27158, 1000.000000000000000 ) ;
#45000 = ADVANCED_FACE ( 'NONE', ( #3360 ), #26142, .T. ) ;
#45001 = VECTOR ( 'NONE', #46637, 1000.000000000000000 ) ;
#45002 = CARTESIAN_POINT ( 'NONE',  ( -166.6959734468149463, 0.000000000000000000, 165.0000000000000000 ) ) ;
#45003 = CARTESIAN_POINT ( 'NONE',  ( -37.27397286063865778, 4.111076158911805223, 7.697694107796192675 ) ) ;
#45004 = AXIS2_PLACEMENT_3D ( 'NONE', #27135, #34849, #42753 ) ;
#45005 = CARTESIAN_POINT ( 'NONE',  ( -1.320835335343009787, 0.01943189458965158267, 9.943883492372876276 ) ) ;
#45006 = DIRECTION ( 'NONE',  ( 0.9770330068457271366, 0.000000000000000000, 0.2130880182788258970 ) ) ;
#45007 = EDGE_CURVE ( 'NONE', #609, #27759, #45, .T. ) ;
#45008 = DIRECTION ( 'NONE',  ( 0.000000000000000000, 1.000000000000000000, 0.000000000000000000 ) ) ;
#45009 = LINE ( 'NONE', #17590, #40163 ) ;
#45010 = DIRECTION ( 'NONE',  ( -1.000000000000000000, 0.000000000000000000, -0.000000000000000000 ) ) ;
#45011 = ORIENTED_EDGE ( 'NONE', *, *, #19327, .T. ) ;
#45012 = CARTESIAN_POINT ( 'NONE',  ( 73.30402655318508209, -1.750000000000009992, -159.1817124430720298 ) ) ;
#45013 =( BOUNDED_CURVE ( )  B_SPLINE_CURVE ( 3, ( #36585, #9107, #12692, #24764 ),
 .UNSPECIFIED., .F., .F. ) 
 B_SPLINE_CURVE_WITH_KNOTS ( ( 4, 4 ),
 ( 0.000000000000000000, 1.570796326794889675 ),
 .UNSPECIFIED. ) 
 CURVE ( )  GEOMETRIC_REPRESENTATION_ITEM ( )  RATIONAL_B_SPLINE_CURVE ( ( 1.000000000000000000, 0.8047378541243667138, 0.8047378541243667138, 1.000000000000000000 ) ) 
 REPRESENTATION_ITEM ( '' )  );
#45014 = ADVANCED_FACE ( 'NONE', ( #8757 ), #4140, .F. ) ;
#45015 = EDGE_CURVE ( 'NONE', #34498, #38360, #5137, .T. ) ;
#45016 = CARTESIAN_POINT ( 'NONE',  ( 340.0000000000000568, 181.0000000000000853, 355.9999999999998295 ) ) ;
#45017 = FACE_OUTER_BOUND ( 'NONE', #39714, .T. ) ;
#45018 = FACE_OUTER_BOUND ( 'NONE', #13693, .T. ) ;
#45019 =( BOUNDED_CURVE ( )  B_SPLINE_CURVE ( 3, ( #3030, #18680, #14841, #27662 ),
 .UNSPECIFIED., .F., .F. ) 
 B_SPLINE_CURVE_WITH_KNOTS ( ( 4, 4 ),
 ( 3.140184917367548361E-16, 1.570796326794882791 ),
 .UNSPECIFIED. ) 
 CURVE ( )  GEOMETRIC_REPRESENTATION_ITEM ( )  RATIONAL_B_SPLINE_CURVE ( ( 1.000000000000000000, 0.8047378541243681571, 0.8047378541243681571, 1.000000000000000000 ) ) 
 REPRESENTATION_ITEM ( '' )  );
#45020 = ADVANCED_FACE ( 'NONE', ( #36213 ), #558, .F. ) ;
#45021 = VERTEX_POINT ( 'NONE', #39553 ) ;
#45022 = DIRECTION ( 'NONE',  ( -3.172065784643302499E-16, -1.000000000000000000, 2.537652627714642000E-15 ) ) ;
#45023 = ORIENTED_EDGE ( 'NONE', *, *, #45325, .F. ) ;
#45024 = VECTOR ( 'NONE', #12551, 1000.000000000000000 ) ;
#45025 = CARTESIAN_POINT ( 'NONE',  ( -17.23491422248386584, 0.5912720620001978844, 8.727788335465566760 ) ) ;
#45026 = ADVANCED_FACE ( 'NONE', ( #4390 ), #42120, .T. ) ;
#45027 = LINE ( 'NONE', #25816, #22996 ) ;
#45028 = CIRCLE ( 'NONE', #33566, 1.750000000000009992 ) ;
#45029 = EDGE_CURVE ( 'NONE', #8288, #18070, #32097, .T. ) ;
#45030 = VECTOR ( 'NONE', #8582, 1000.000000000000000 ) ;
#45031 = ORIENTED_EDGE ( 'NONE', *, *, #22507, .T. ) ;
#45032 = CARTESIAN_POINT ( 'NONE',  ( 7.499999999999948486, -194.9999999999999716, -240.0000000000000000 ) ) ;
#45033 = CARTESIAN_POINT ( 'NONE',  ( 35.05402655318504657, 1.025126265847089435, 2.568287556927986159 ) ) ;
#45034 = ORIENTED_EDGE ( 'NONE', *, *, #32619, .T. ) ;
#45035 = VERTEX_POINT ( 'NONE', #47196 ) ;
#45036 = AXIS2_PLACEMENT_3D ( 'NONE', #40838, #21085, #13640 ) ;
#45037 = ORIENTED_EDGE ( 'NONE', *, *, #39685, .F. ) ;
#45038 = EDGE_CURVE ( 'NONE', #35686, #17256, #1098, .T. ) ;
#45039 = CARTESIAN_POINT ( 'NONE',  ( -8.277096487746778308, 33.14818118907697198, 7.455576670931136185 ) ) ;
#45040 = CARTESIAN_POINT ( 'NONE',  ( 34.91952936320839740, -13.67027684621004546, -9.422646554964178023 ) ) ;
#45041 = LINE ( 'NONE', #21713, #17720 ) ;
#45042 = AXIS2_PLACEMENT_3D ( 'NONE', #29347, #6493, #2392 ) ;
#45043 = ORIENTED_EDGE ( 'NONE', *, *, #18298, .F. ) ;
#45044 = FACE_BOUND ( 'NONE', #35277, .T. ) ;
#45045 = CARTESIAN_POINT ( 'NONE',  ( 228.9999999999999716, -169.9999999999999716, 474.9999999999998863 ) ) ;
#45046 = FACE_OUTER_BOUND ( 'NONE', #13708, .T. ) ;
#45047 = EDGE_LOOP ( 'NONE', ( #48321, #18432, #11952, #30218 ) ) ;
#45048 = ORIENTED_EDGE ( 'NONE', *, *, #16201, .T. ) ;
#45049 = DIRECTION ( 'NONE',  ( -1.000000000000000000, -0.000000000000000000, -0.000000000000000000 ) ) ;
#45050 = FACE_OUTER_BOUND ( 'NONE', #47853, .T. ) ;
#45051 = FACE_OUTER_BOUND ( 'NONE', #50171, .T. ) ;
#45052 = ORIENTED_EDGE ( 'NONE', *, *, #49759, .F. ) ;
#45053 = DIRECTION ( 'NONE',  ( 0.000000000000000000, -0.000000000000000000, -1.000000000000000000 ) ) ;
#45054 = DIRECTION ( 'NONE',  ( 1.000000000000000000, 0.000000000000000000, 0.000000000000000000 ) ) ;
#45055 = CARTESIAN_POINT ( 'NONE',  ( -14.99999999999782041, 17.00000000000000000, 115.0000000000000142 ) ) ;
#45056 = CARTESIAN_POINT ( 'NONE',  ( -0.6803378293975504976, -1.026336841997344429, 9.975326647350891918 ) ) ;
#45057 = CARTESIAN_POINT ( 'NONE',  ( 36.76598589393955052, 7.383243274241862331, -8.192531242611266862 ) ) ;
#45058 = CARTESIAN_POINT ( 'NONE',  ( -48.44597344681492501, 0.000000000000000000, 162.5682875569279702 ) ) ;
#45059 = CARTESIAN_POINT ( 'NONE',  ( -86.69597344681494633, 1.750000000000010214, 40.81828755692798438 ) ) ;
#45060 = CARTESIAN_POINT ( 'NONE',  ( 0.9983599181300923942, 1.124146016603553733, 9.953784399990620813 ) ) ;
#45061 = DIRECTION ( 'NONE',  ( -1.000000000000000000, -0.000000000000000000, -0.000000000000000000 ) ) ;
#45062 = VECTOR ( 'NONE', #45268, 1000.000000000000000 ) ;
#45063 = CARTESIAN_POINT ( 'NONE',  ( -1.011271242968683426, -0.7347315653655928092, -3.333333333333333481 ) ) ;
#45064 = AXIS2_PLACEMENT_3D ( 'NONE', #10087, #26494, #45702 ) ;
#45065 = CARTESIAN_POINT ( 'NONE',  ( -5.000000000000000000, 165.2000000000000171, 340.1999999999997044 ) ) ;
#45066 = ORIENTED_EDGE ( 'NONE', *, *, #47160, .T. ) ;
#45067 = VECTOR ( 'NONE', #33353, 1000.000000000000000 ) ;
#45068 = FACE_OUTER_BOUND ( 'NONE', #34024, .T. ) ;
#45069 = MECHANICAL_DESIGN_GEOMETRIC_PRESENTATION_REPRESENTATION (  '', ( #16428 ), #43458 ) ;
#45070 = LINE ( 'NONE', #41503, #7837 ) ;
#45071 =( GEOMETRIC_REPRESENTATION_CONTEXT ( 3 ) GLOBAL_UNCERTAINTY_ASSIGNED_CONTEXT ( ( #40005 ) ) GLOBAL_UNIT_ASSIGNED_CONTEXT ( ( #7757, #31364, #43152 ) ) REPRESENTATION_CONTEXT ( 'NONE', 'WORKASPACE' ) );
#45072 = CARTESIAN_POINT ( 'NONE',  ( 164.9999999999999716, 17.00000000000000000, -90.00000000000002842 ) ) ;
#45073 = ORIENTED_EDGE ( 'NONE', *, *, #30594, .T. ) ;
#45074 = ADVANCED_FACE ( 'NONE', ( #16685 ), #27490, .T. ) ;
#45075 = EDGE_CURVE ( 'NONE', #50239, #38442, #39296, .T. ) ;
#45076 = CARTESIAN_POINT ( 'NONE',  ( 349.9999999999999432, -164.9999999999999432, 343.9999999999997726 ) ) ;
#45077 = ORIENTED_EDGE ( 'NONE', *, *, #1217, .T. ) ;
#45078 = LINE ( 'NONE', #9957, #33728 ) ;
#45079 = CARTESIAN_POINT ( 'NONE',  ( -166.6959734468149463, 1.750000000000010658, 80.81828755692798438 ) ) ;
#45080 = CYLINDRICAL_SURFACE ( 'NONE', #37964, 4.000000000000003553 ) ;
#45081 = FACE_OUTER_BOUND ( 'NONE', #1236, .T. ) ;
#45082 = ADVANCED_FACE ( 'NONE', ( #15944 ), #39806, .F. ) ;
#45083 = VERTEX_POINT ( 'NONE', #5638 ) ;
#45084 = PRESENTATION_STYLE_ASSIGNMENT (( #13795 ) ) ;
#45085 = ORIENTED_EDGE ( 'NONE', *, *, #8346, .F. ) ;
#45086 = ORIENTED_EDGE ( 'NONE', *, *, #7190, .F. ) ;
#45087 = EDGE_CURVE ( 'NONE', #45549, #47156, #9243, .T. ) ;
#45088 = CYLINDRICAL_SURFACE ( 'NONE', #4155, 1.750000000000015543 ) ;
#45089 = EDGE_CURVE ( 'NONE', #37129, #48972, #45372, .T. ) ;
#45090 = ORIENTED_EDGE ( 'NONE', *, *, #595, .F. ) ;
#45091 = CARTESIAN_POINT ( 'NONE',  ( 35.00000000000186162, 17.00000000000000000, 90.00000000000000000 ) ) ;
#45092 = DIRECTION ( 'NONE',  ( 0.000000000000000000, -1.000000000000000000, -0.000000000000000000 ) ) ;
#45093 = EDGE_LOOP ( 'NONE', ( #44368, #3357, #28216, #14258 ) ) ;
#45094 = DIRECTION ( 'NONE',  ( 0.9770330068457271366, -0.000000000000000000, 0.2130880182788259247 ) ) ;
#45095 = EDGE_CURVE ( 'NONE', #2812, #4778, #24026, .T. ) ;
#45096 = CARTESIAN_POINT ( 'NONE',  ( -6.695973446814940111, -1.750000000000024203, -79.18171244307201562 ) ) ;
#45097 = PLANE ( 'NONE',  #38267 ) ;
#45098 = ORIENTED_EDGE ( 'NONE', *, *, #17772, .T. ) ;
#45099 = CARTESIAN_POINT ( 'NONE',  ( -5.000000000000000000, 165.2000000000000171, -359.8000000000002387 ) ) ;
#45100 = CARTESIAN_POINT ( 'NONE',  ( -114.9999999999984652, 17.00000000000000000, 35.00000000000000000 ) ) ;
#45101 = VECTOR ( 'NONE', #45586, 1000.000000000000000 ) ;
#45102 = ORIENTED_EDGE ( 'NONE', *, *, #14505, .F. ) ;
#45103 = CARTESIAN_POINT ( 'NONE',  ( 181.0000000000000000, -174.9999999999999716, -356.0000000000001705 ) ) ;
#45104 = DIRECTION ( 'NONE',  ( 0.000000000000000000, 0.2223603367690619725, -0.9749645535258958384 ) ) ;
#45105 = ORIENTED_EDGE ( 'NONE', *, *, #35565, .T. ) ;
#45106 = ORIENTED_EDGE ( 'NONE', *, *, #8273, .T. ) ;
#45107 = ORIENTED_EDGE ( 'NONE', *, *, #2008, .F. ) ;
#45108 = CARTESIAN_POINT ( 'NONE',  ( 183.0000000000000000, -272.5000000000000000, -111.0000000000001563 ) ) ;
#45109 = FACE_OUTER_BOUND ( 'NONE', #18982, .T. ) ;
#45110 = VECTOR ( 'NONE', #39194, 1000.000000000000000 ) ;
#45111 = ORIENTED_EDGE ( 'NONE', *, *, #40246, .T. ) ;
#45112 = DIRECTION ( 'NONE',  ( -0.000000000000000000, -0.000000000000000000, -1.000000000000000000 ) ) ;
#45113 = CARTESIAN_POINT ( 'NONE',  ( -7.372990760266265653, 3.388353563403873350E-15, -22.00000000000000000 ) ) ;
#45114 = B_SPLINE_CURVE_WITH_KNOTS ( 'NONE', 3,
 ( #21910, #25756, #6498, #30364 ),
 .UNSPECIFIED., .F., .F.,
 ( 4, 4 ),
 ( 0.000000000000000000, 0.2545280377015988194 ),
 .UNSPECIFIED. ) ;
#45115 = CARTESIAN_POINT ( 'NONE',  ( 111.5540265531850537, 1.025126265847081886, 39.06828755692799149 ) ) ;
#45116 = ORIENTED_EDGE ( 'NONE', *, *, #34632, .F. ) ;
#45117 = CARTESIAN_POINT ( 'NONE',  ( -165.0000000000000284, 16.00000000000000000, 30.00000000000000000 ) ) ;
#45118 = LINE ( 'NONE', #20784, #34156 ) ;
#45119 = EDGE_CURVE ( 'NONE', #8942, #27159, #109, .T. ) ;
#45120 = FACE_OUTER_BOUND ( 'NONE', #26693, .T. ) ;
#45121 = EDGE_CURVE ( 'NONE', #1398, #48718, #1554, .T. ) ;
#45122 = EDGE_LOOP ( 'NONE', ( #27358, #43785, #1140, #5251 ) ) ;
#45123 = DIRECTION ( 'NONE',  ( 0.000000000000000000, 0.000000000000000000, 1.000000000000000000 ) ) ;
#45124 = CARTESIAN_POINT ( 'NONE',  ( -0.3910393408547386818, -3.877122853643371947, 9.741991644047244492 ) ) ;
#45125 = CARTESIAN_POINT ( 'NONE',  ( -0.3862712429686895876, 1.188820645368940720, 10.00000000000000000 ) ) ;
#45126 = CARTESIAN_POINT ( 'NONE',  ( -64.99999999999971578, 16.00000000000000000, -84.99999999999998579 ) ) ;
#45127 = ORIENTED_EDGE ( 'NONE', *, *, #26779, .F. ) ;
#45128 = CYLINDRICAL_SURFACE ( 'NONE', #44335, 1.750000000000015543 ) ;
#45129 = DIRECTION ( 'NONE',  ( 0.8637789008984335659, -0.000000000000000000, 0.5038710255240859137 ) ) ;
#45130 = CARTESIAN_POINT ( 'NONE',  ( -46.69597344681494633, 1.750000000000009992, -159.1817124430720298 ) ) ;
#45131 = CARTESIAN_POINT ( 'NONE',  ( 1.250000000000000222, 0.000000000000000000, 10.00000000000000000 ) ) ;
#45132 = DIRECTION ( 'NONE',  ( 0.000000000000000000, 0.000000000000000000, 1.000000000000000000 ) ) ;
#45133 = VECTOR ( 'NONE', #13395, 1000.000000000000000 ) ;
#45134 = ORIENTED_EDGE ( 'NONE', *, *, #12176, .F. ) ;
#45135 = CARTESIAN_POINT ( 'NONE',  ( 357.1715728752539576, 183.0000000000000284, 357.9999999999998295 ) ) ;
#45136 = EDGE_LOOP ( 'NONE', ( #12247, #38144, #14621, #44674 ) ) ;
#45137 = CARTESIAN_POINT ( 'NONE',  ( -5.670847180967843570, 1.750000000000022871, 159.7931612910808781 ) ) ;
#45138 = ORIENTED_EDGE ( 'NONE', *, *, #43669, .T. ) ;
#45139 = CARTESIAN_POINT ( 'NONE',  ( -85.67084718096784002, 1.750000000000010214, 119.7931612910808781 ) ) ;
#45140 = VECTOR ( 'NONE', #16582, 1000.000000000000000 ) ;
#45141 = AXIS2_PLACEMENT_3D ( 'NONE', #42509, #3253, #37939 ) ;
#45142 = CARTESIAN_POINT ( 'NONE',  ( 74.32915281903215998, 1.750000000000010214, 119.7931612910808781 ) ) ;
#45143 = EDGE_LOOP ( 'NONE', ( #6422, #32133 ) ) ;
#45144 = PLANE ( 'NONE',  #39268 ) ;
#45145 = VERTEX_POINT ( 'NONE', #21047 ) ;
#45146 = CARTESIAN_POINT ( 'NONE',  ( 75.05402655318509630, 2.143131898507880377E-16, -77.43171244307198720 ) ) ;
#45147 = DIRECTION ( 'NONE',  ( -0.000000000000000000, -0.000000000000000000, -1.000000000000000000 ) ) ;
#45148 = CARTESIAN_POINT ( 'NONE',  ( 114.3291528190321173, 1.749999999999996669, -158.1565861772249377 ) ) ;
#45149 = CARTESIAN_POINT ( 'NONE',  ( -127.7210997126620242, 1.749999999999996669, -118.1565861772249661 ) ) ;
#45150 = ADVANCED_FACE ( 'NONE', ( #45120 ), #28752, .F. ) ;
#45151 = FACE_OUTER_BOUND ( 'NONE', #8743, .T. ) ;
#45152 = ORIENTED_EDGE ( 'NONE', *, *, #47785, .T. ) ;
#45153 = ORIENTED_EDGE ( 'NONE', *, *, #5891, .T. ) ;
#45154 = FACE_OUTER_BOUND ( 'NONE', #49423, .T. ) ;
#45155 =( BOUNDED_CURVE ( )  B_SPLINE_CURVE ( 3, ( #36397, #47368, #12264, #27924 ),
 .UNSPECIFIED., .F., .F. ) 
 B_SPLINE_CURVE_WITH_KNOTS ( ( 4, 4 ),
 ( 4.712388980384689674, 6.283185307179586232 ),
 .UNSPECIFIED. ) 
 CURVE ( )  GEOMETRIC_REPRESENTATION_ITEM ( )  RATIONAL_B_SPLINE_CURVE ( ( 1.000000000000000000, 0.8047378541243649375, 0.8047378541243649375, 1.000000000000000000 ) ) 
 REPRESENTATION_ITEM ( '' )  );
#45156 = ORIENTED_EDGE ( 'NONE', *, *, #43382, .F. ) ;
#45157 = LINE ( 'NONE', #14131, #25923 ) ;
#45158 = CARTESIAN_POINT ( 'NONE',  ( 33.30402655318503946, 1.750000000000009992, -159.1817124430720298 ) ) ;
#45159 = EDGE_LOOP ( 'NONE', ( #18965, #5633, #25876, #33514, #2556, #11445 ) ) ;
#45160 = CARTESIAN_POINT ( 'NONE',  ( -114.9999999999994031, 17.00000000000000000, -54.99999999999999289 ) ) ;
#45161 =( BOUNDED_CURVE ( )  B_SPLINE_CURVE ( 3, ( #8119, #34825, #3225, #27108 ),
 .UNSPECIFIED., .F., .F. ) 
 B_SPLINE_CURVE_WITH_KNOTS ( ( 4, 4 ),
 ( 4.712388980384689674, 6.283185307179586232 ),
 .UNSPECIFIED. ) 
 CURVE ( )  GEOMETRIC_REPRESENTATION_ITEM ( )  RATIONAL_B_SPLINE_CURVE ( ( 1.000000000000000000, 0.8047378541243649375, 0.8047378541243649375, 1.000000000000000000 ) ) 
 REPRESENTATION_ITEM ( '' )  );
#45162 = AXIS2_PLACEMENT_3D ( 'NONE', #15560, #31223, #11706 ) ;
#45163 = CARTESIAN_POINT ( 'NONE',  ( 340.0000000000001137, 166.6568542494924259, 341.6568542494921417 ) ) ;
#45164 = ORIENTED_EDGE ( 'NONE', *, *, #3567, .T. ) ;
#45165 = CARTESIAN_POINT ( 'NONE',  ( 195.0540265531851105, 1.025126265847089879, -77.43171244307200141 ) ) ;
#45166 = CARTESIAN_POINT ( 'NONE',  ( 224.9999999999999432, 175.0000000000000000, 500.0000000000000000 ) ) ;
#45167 = CARTESIAN_POINT ( 'NONE',  ( -48.44597344681496054, -1.025126265847089435, -157.4317124430720582 ) ) ;
#45168 = DIRECTION ( 'NONE',  ( 1.000000000000000000, 0.000000000000000000, -0.000000000000000000 ) ) ;
#45169 = EDGE_LOOP ( 'NONE', ( #32321, #133, #32251, #5256 ) ) ;
#45170 = AXIS2_PLACEMENT_3D ( 'NONE', #49334, #2680, #18318 ) ;
#45171 = ORIENTED_EDGE ( 'NONE', *, *, #33473, .T. ) ;
#45172 = VERTEX_POINT ( 'NONE', #16955 ) ;
#45173 = DIRECTION ( 'NONE',  ( 1.000000000000000000, 0.000000000000000000, -7.793956916774525800E-48 ) ) ;
#45174 = CARTESIAN_POINT ( 'NONE',  ( 31.55402655318503236, 0.000000000000000000, 119.0682875569279702 ) ) ;
#45175 =( BOUNDED_CURVE ( )  B_SPLINE_CURVE ( 3, ( #46735, #34487, #50065, #11636 ),
 .UNSPECIFIED., .F., .F. ) 
 B_SPLINE_CURVE_WITH_KNOTS ( ( 4, 4 ),
 ( 0.000000000000000000, 1.570796326794896558 ),
 .UNSPECIFIED. ) 
 CURVE ( )  GEOMETRIC_REPRESENTATION_ITEM ( )  RATIONAL_B_SPLINE_CURVE ( ( 1.000000000000000000, 0.8047378541243649375, 0.8047378541243649375, 1.000000000000000000 ) ) 
 REPRESENTATION_ITEM ( '' )  );
#45176 = CARTESIAN_POINT ( 'NONE',  ( -1.249999999999999778, 0.000000000000000000, 10.00000000000000000 ) ) ;
#45177 = CIRCLE ( 'NONE', #36224, 4.000000000000003553 ) ;
#45178 = ORIENTED_EDGE ( 'NONE', *, *, #6149, .T. ) ;
#45179 = DIRECTION ( 'NONE',  ( 0.000000000000000000, -1.000000000000000000, 8.021842663476564905E-17 ) ) ;
#45180 = EDGE_CURVE ( 'NONE', #18068, #44090, #5389, .T. ) ;
#45181 = ORIENTED_EDGE ( 'NONE', *, *, #767, .T. ) ;
#45182 =( NAMED_UNIT ( * ) SI_UNIT ( $, .STERADIAN. ) SOLID_ANGLE_UNIT ( ) );
#45183 = CARTESIAN_POINT ( 'NONE',  ( -4.763548243873389154, 16.57409059453848599, 8.727788335465566760 ) ) ;
#45184 = CARTESIAN_POINT ( 'NONE',  ( 210.0000000000000568, 0.000000000000000000, 80.81828755692798438 ) ) ;
#45185 = CARTESIAN_POINT ( 'NONE',  ( -1.011271242968688533, 0.7347315653655859258, 10.00000000000000000 ) ) ;
#45186 = DIRECTION ( 'NONE',  ( 0.000000000000000000, -2.537652627714643577E-15, -1.000000000000000000 ) ) ;
#45187 = PLANE ( 'NONE',  #39740 ) ;
#45188 = CARTESIAN_POINT ( 'NONE',  ( -114.9999999999997158, 17.00000000000000000, -84.99999999999998579 ) ) ;
#45189 = EDGE_LOOP ( 'NONE', ( #17146, #32859, #34110, #5566, #29797 ) ) ;
#45190 = DIRECTION ( 'NONE',  ( 1.000000000000000000, -0.000000000000000000, -0.000000000000000000 ) ) ;
#45191 = CARTESIAN_POINT ( 'NONE',  ( -1.578643388466005160, 1.550786058692512182, 9.881002359080275355 ) ) ;
#45192 = DIRECTION ( 'NONE',  ( 1.000000000000000000, -5.326388832052271710E-25, 1.587271980518778491E-16 ) ) ;
#45193 = EDGE_LOOP ( 'NONE', ( #18226, #19652, #42394, #1825, #28862, #12095 ) ) ;
#45194 = FACE_OUTER_BOUND ( 'NONE', #40156, .T. ) ;
#45195 = EDGE_LOOP ( 'NONE', ( #7434, #41089, #42508 ) ) ;
#45196 = DIRECTION ( 'NONE',  ( 0.000000000000000000, -1.000000000000000000, -3.186989995019654210E-49 ) ) ;
#45197 = VECTOR ( 'NONE', #485, 1000.000000000000000 ) ;
#45198 = LINE ( 'NONE', #49031, #43016 ) ;
#45199 = CARTESIAN_POINT ( 'NONE',  ( -1.655785408455817675, -0.7536129375911022610, 9.903764339332079558 ) ) ;
#45200 = VECTOR ( 'NONE', #45953, 1000.000000000000000 ) ;
#45201 = AXIS2_PLACEMENT_3D ( 'NONE', #32704, #9352, #31957 ) ;
#45202 = CARTESIAN_POINT ( 'NONE',  ( 194.9999999999999716, 164.9999999999999716, 500.0000000000000000 ) ) ;
#45203 = ORIENTED_EDGE ( 'NONE', *, *, #25993, .F. ) ;
#45204 = CARTESIAN_POINT ( 'NONE',  ( -0.6215990105957072132, 1.608617984725374983, 9.928159647716134018 ) ) ;
#45205 = CARTESIAN_POINT ( 'NONE',  ( -14.99999999999906919, 17.00000000000000000, -24.99999999999999289 ) ) ;
#45206 = CARTESIAN_POINT ( 'NONE',  ( 3.695802964311526218, 9.324875653452767921, 9.390253821402620105 ) ) ;
#45207 = ADVANCED_FACE ( 'NONE', ( #48197 ), #50153, .F. ) ;
#45208 = ORIENTED_EDGE ( 'NONE', *, *, #35505, .F. ) ;
#45209 = ORIENTED_EDGE ( 'NONE', *, *, #6700, .F. ) ;
#45210 = FACE_OUTER_BOUND ( 'NONE', #36116, .T. ) ;
#45211 = EDGE_CURVE ( 'NONE', #26902, #39755, #35800, .T. ) ;
#45212 = CARTESIAN_POINT ( 'NONE',  ( 30.00000000000153833, 17.00000000000000000, 35.00000000000000000 ) ) ;
#45213 = ADVANCED_FACE ( 'NONE', ( #48696 ), #33619, .T. ) ;
#45214 = ORIENTED_EDGE ( 'NONE', *, *, #38656, .F. ) ;
#45215 = EDGE_LOOP ( 'NONE', ( #26116, #15121, #45854, #46986 ) ) ;
#45216 = DIRECTION ( 'NONE',  ( 0.000000000000000000, 0.000000000000000000, 1.000000000000000000 ) ) ;
#45217 = CARTESIAN_POINT ( 'NONE',  ( 3.245329132135053474, 7.282608432884214444, -6.098637220230962441E-16 ) ) ;
#45218 = CARTESIAN_POINT ( 'NONE',  ( -17.67745476136668614, -37.99701471135970365, 7.544061037322996377 ) ) ;
#45219 = CARTESIAN_POINT ( 'NONE',  ( 31.55402655318503236, 1.025126265847089213, 159.0682875569279418 ) ) ;
#45220 = ORIENTED_EDGE ( 'NONE', *, *, #8880, .T. ) ;
#45221 = CARTESIAN_POINT ( 'NONE',  ( 350.0000000000000000, 183.0000000000000284, -356.0000000000002274 ) ) ;
#45222 = ORIENTED_EDGE ( 'NONE', *, *, #1396, .T. ) ;
#45223 = EDGE_CURVE ( 'NONE', #16952, #22476, #29504, .T. ) ;
#45224 = ADVANCED_FACE ( 'NONE', ( #10001 ), #17924, .T. ) ;
#45225 = DIRECTION ( 'NONE',  ( 0.000000000000000000, -1.000000000000000000, 0.000000000000000000 ) ) ;
#45226 = EDGE_CURVE ( 'NONE', #46289, #2019, #5159, .T. ) ;
#45227 = PLANE ( 'NONE',  #33924 ) ;
#45228 = ORIENTED_EDGE ( 'NONE', *, *, #11770, .F. ) ;
#45229=STYLED_ITEM('',(#50747),#5610);
#45230 = ORIENTED_EDGE ( 'NONE', *, *, #13768, .F. ) ;
#45231 = CARTESIAN_POINT ( 'NONE',  ( -22.82242230425432439, 7.611558401714507482, 229.0000000000000000 ) ) ;
#45232 = VECTOR ( 'NONE', #33675, 1000.000000000000000 ) ;
#45233 = CARTESIAN_POINT ( 'NONE',  ( 191.5540265531851105, 0.000000000000000000, -0.9317124430720247208 ) ) ;
#45234 = ORIENTED_EDGE ( 'NONE', *, *, #13659, .T. ) ;
#45235 = DIRECTION ( 'NONE',  ( -0.000000000000000000, -1.000000000000000000, 2.537652627714643577E-15 ) ) ;
#45236 = EDGE_CURVE ( 'NONE', #47355, #16274, #25175, .T. ) ;
#45237 = EDGE_CURVE ( 'NONE', #50500, #12617, #43519, .T. ) ;
#45238 = ORIENTED_EDGE ( 'NONE', *, *, #14646, .T. ) ;
#45239 = AXIS2_PLACEMENT_3D ( 'NONE', #3642, #28006, #43156 ) ;
#45240 = FACE_OUTER_BOUND ( 'NONE', #46467, .T. ) ;
#45241 = ORIENTED_EDGE ( 'NONE', *, *, #31182, .F. ) ;
#45242 = CARTESIAN_POINT ( 'NONE',  ( -19.99999999999815969, 17.00000000000000000, 65.00000000000000000 ) ) ;
#45243 = ADVANCED_FACE ( 'NONE', ( #46624 ), #31033, .F. ) ;
#45244 = CARTESIAN_POINT ( 'NONE',  ( 3.566525152641073504, -1.569997364302916809, 9.741991644047246268 ) ) ;
#45245 = FACE_OUTER_BOUND ( 'NONE', #47939, .T. ) ;
#45246 = CARTESIAN_POINT ( 'NONE',  ( -204.9459734468149463, 2.143131898507880377E-16, -40.93171244307202983 ) ) ;
#45247 = ADVANCED_FACE ( 'NONE', ( #11529 ), #27178, .T. ) ;
#45248 = VECTOR ( 'NONE', #44589, 1000.000000000000000 ) ;
#45249 = LINE ( 'NONE', #42181, #42161 ) ;
#45250 = ORIENTED_EDGE ( 'NONE', *, *, #17778, .F. ) ;
#45251 = PLANE ( 'NONE',  #7858 ) ;
#45252 = EDGE_CURVE ( 'NONE', #42696, #34995, #14860, .T. ) ;
#45253 = CARTESIAN_POINT ( 'NONE',  ( 339.9999999999998863, -180.9999999999999716, 357.9999999999997726 ) ) ;
#45254 = B_SPLINE_SURFACE_WITH_KNOTS ( 'NONE', 3, 3, ( 
 ( #26253, #25234, #41891, #22386 ),
 ( #21633, #2871, #40883, #17536 ),
 ( #37321, #49787, #33209, #2146 ),
 ( #17791, #5728, #30352, #49032 ) ),
 .UNSPECIFIED., .F., .F., .F.,
 ( 4, 4 ),
 ( 4, 4 ),
 ( 0.000000000000000000, 1.000000000000000000 ),
 ( 0.000000000000000000, 1.000000000000000000 ),
 .UNSPECIFIED. ) ;
#45255 = CARTESIAN_POINT ( 'NONE',  ( 71.55402655318505367, 1.025126265847089435, -117.4317124430720156 ) ) ;
#45256 = CARTESIAN_POINT ( 'NONE',  ( -35.51958307830761896, 12.13749199045067684, -6.568693074176341185 ) ) ;
#45257 = CARTESIAN_POINT ( 'NONE',  ( 181.0000000000000284, -174.9999999999999716, -113.0000000000001563 ) ) ;
#45258 = CYLINDRICAL_SURFACE ( 'NONE', #13846, 1.750000000000001554 ) ;
#45259 = CARTESIAN_POINT ( 'NONE',  ( 32.27890028733795447, -1.750000000000010214, 121.8434138227750623 ) ) ;
#45260 = DIRECTION ( 'NONE',  ( -0.000000000000000000, -0.000000000000000000, -1.000000000000000000 ) ) ;
#45261 = VECTOR ( 'NONE', #19821, 1000.000000000000000 ) ;
#45262 = EDGE_CURVE ( 'NONE', #43085, #26536, #26668, .T. ) ;
#45263 = DIRECTION ( 'NONE',  ( -0.000000000000000000, -0.000000000000000000, -1.000000000000000000 ) ) ;
#45264 = ORIENTED_EDGE ( 'NONE', *, *, #45999, .T. ) ;
#45265 = CARTESIAN_POINT ( 'NONE',  ( -115.0000000000000284, 16.00000000000000000, -90.00000000000000000 ) ) ;
#45266 = EDGE_CURVE ( 'NONE', #36841, #40138, #3552, .T. ) ;
#45267 = EDGE_CURVE ( 'NONE', #47621, #29419, #37726, .T. ) ;
#45268 = DIRECTION ( 'NONE',  ( -0.000000000000000000, -0.000000000000000000, -1.000000000000000000 ) ) ;
#45269 = CARTESIAN_POINT ( 'NONE',  ( 0.4426377647354858835, 1.666766018367784596, 9.928159647716132241 ) ) ;
#45270 = CARTESIAN_POINT ( 'NONE',  ( 20.40054609052976531, -26.26366202847973597, -3.760136334089591248 ) ) ;
#45271 = DIRECTION ( 'NONE',  ( -0.000000000000000000, 1.000000000000000000, 0.000000000000000000 ) ) ;
#45272 = EDGE_CURVE ( 'NONE', #11294, #20141, #34130, .T. ) ;
#45273 = AXIS2_PLACEMENT_3D ( 'NONE', #16632, #8187, #11778 ) ;
#45274 = VERTEX_POINT ( 'NONE', #49711 ) ;
#45275 = ORIENTED_EDGE ( 'NONE', *, *, #45534, .T. ) ;
#45276 = CARTESIAN_POINT ( 'NONE',  ( 75.05402655318509630, 2.143131898507880377E-16, 42.56828755692799859 ) ) ;
#45277 = VECTOR ( 'NONE', #3500, 1000.000000000000000 ) ;
#45278 = ADVANCED_FACE ( 'NONE', ( #18695 ), #22459, .T. ) ;
#45279 = CARTESIAN_POINT ( 'NONE',  ( 74.32915281903215998, 1.750000000000009548, 39.79316129108089228 ) ) ;
#45280 = EDGE_LOOP ( 'NONE', ( #1224, #21841, #25663, #29038, #6611, #25041 ) ) ;
#45281 = CIRCLE ( 'NONE', #284, 0.5000000000000004441 ) ;
#45282 = CARTESIAN_POINT ( 'NONE',  ( 151.5540265531850537, 0.000000000000000000, 39.06828755692798438 ) ) ;
#45283 = CYLINDRICAL_SURFACE ( 'NONE', #14268, 2.000000000000001776 ) ;
#45284 = ORIENTED_EDGE ( 'NONE', *, *, #32022, .F. ) ;
#45285 = ORIENTED_EDGE ( 'NONE', *, *, #37262, .F. ) ;
#45286 = ORIENTED_EDGE ( 'NONE', *, *, #14596, .F. ) ;
#45287 = EDGE_CURVE ( 'NONE', #49568, #34456, #45869, .T. ) ;
#45288 = LINE ( 'NONE', #10170, #26620 ) ;
#45289 = CARTESIAN_POINT ( 'NONE',  ( 36.02002318912989409, -10.56068015588340181, -3.721387749823056090 ) ) ;
#45290 = FACE_OUTER_BOUND ( 'NONE', #14668, .T. ) ;
#45291 = ORIENTED_EDGE ( 'NONE', *, *, #19405, .F. ) ;
#45292 = CARTESIAN_POINT ( 'NONE',  ( 169.0000000000000000, 2.775557561562891351E-14, -111.0000000000001563 ) ) ;
#45293 = DIRECTION ( 'NONE',  ( -1.000000000000000000, 0.000000000000000000, 0.000000000000000000 ) ) ;
#45294 = ORIENTED_EDGE ( 'NONE', *, *, #44313, .F. ) ;
#45295 = EDGE_CURVE ( 'NONE', #41417, #21137, #34372, .T. ) ;
#45296 = ORIENTED_EDGE ( 'NONE', *, *, #15849, .F. ) ;
#45297 = LINE ( 'NONE', #30179, #2465 ) ;
#45298 = CARTESIAN_POINT ( 'NONE',  ( -46.76852358249002606, 17.86468378716741512, -9.367992836599954742 ) ) ;
#45299 = CARTESIAN_POINT ( 'NONE',  ( -206.6959734468149463, 1.750000000000009992, -159.1817124430720298 ) ) ;
#45300 = ORIENTED_EDGE ( 'NONE', *, *, #10891, .T. ) ;
#45301 = CARTESIAN_POINT ( 'NONE',  ( 1.782521105131670724, -0.3635605703593869920, 9.903764339332079558 ) ) ;
#45302 = CARTESIAN_POINT ( 'NONE',  ( 75.05402655318509630, 1.025126265847088991, 162.5682875569279133 ) ) ;
#45303 = EDGE_CURVE ( 'NONE', #16866, #35257, #18947, .T. ) ;
#45304 = LINE ( 'NONE', #37915, #28452 ) ;
#45305 = EDGE_CURVE ( 'NONE', #27903, #8207, #7432, .T. ) ;
#45306 = CARTESIAN_POINT ( 'NONE',  ( -14.99999999999970868, 16.00000000000000000, -60.00000000000000000 ) ) ;
#45307 = CARTESIAN_POINT ( 'NONE',  ( 185.0000000000000000, -272.4999999999999432, -355.9999999999999432 ) ) ;
#45308 = EDGE_CURVE ( 'NONE', #41530, #41472, #23837, .T. ) ;
#45309 = VECTOR ( 'NONE', #15325, 1000.000000000000000 ) ;
#45310 = LINE ( 'NONE', #2493, #27521 ) ;
#45311 = ADVANCED_FACE ( 'NONE', ( #7679 ), #16379, .F. ) ;
#45312 = DIRECTION ( 'NONE',  ( -1.000000000000000000, -0.000000000000000000, -0.000000000000000000 ) ) ;
#45313 = CARTESIAN_POINT ( 'NONE',  ( 1.250000000000000222, 0.000000000000000000, 10.00000000000000000 ) ) ;
#45314 = ADVANCED_FACE ( 'NONE', ( #992 ), #734, .F. ) ;
#45315 = CARTESIAN_POINT ( 'NONE',  ( 192.2789002873380184, 1.750000000000010436, 79.79316129108087807 ) ) ;
#45316 = AXIS2_PLACEMENT_3D ( 'NONE', #39892, #8829, #35803 ) ;
#45317 = FACE_OUTER_BOUND ( 'NONE', #33577, .T. ) ;
#45318 = ORIENTED_EDGE ( 'NONE', *, *, #30288, .T. ) ;
#45319 = FACE_OUTER_BOUND ( 'NONE', #18100, .T. ) ;
#45320 =( BOUNDED_CURVE ( )  B_SPLINE_CURVE ( 3, ( #49391, #14793, #34557, #42997 ),
 .UNSPECIFIED., .F., .F. ) 
 B_SPLINE_CURVE_WITH_KNOTS ( ( 4, 4 ),
 ( 1.570796326794896558, 3.141592653589793116 ),
 .UNSPECIFIED. ) 
 CURVE ( )  GEOMETRIC_REPRESENTATION_ITEM ( )  RATIONAL_B_SPLINE_CURVE ( ( 1.000000000000000000, 0.8047378541243649375, 0.8047378541243649375, 1.000000000000000000 ) ) 
 REPRESENTATION_ITEM ( '' )  );
#45321 = DIRECTION ( 'NONE',  ( -1.000000000000000000, -0.000000000000000000, -0.000000000000000000 ) ) ;
#45322 = LINE ( 'NONE', #7119, #9902 ) ;
#45323 = ORIENTED_EDGE ( 'NONE', *, *, #20553, .F. ) ;
#45324 = CARTESIAN_POINT ( 'NONE',  ( 31.55402655318503236, 1.025126265847089657, -80.93171244307201562 ) ) ;
#45325 = EDGE_CURVE ( 'NONE', #25314, #13960, #28102, .T. ) ;
#45326 = VERTEX_POINT ( 'NONE', #32047 ) ;
#45327 = DIRECTION ( 'NONE',  ( 0.000000000000000000, 0.000000000000000000, 1.000000000000000000 ) ) ;
#45328 = DIRECTION ( 'NONE',  ( -1.000000000000000000, 0.000000000000000000, 0.000000000000000000 ) ) ;
#45329 = CARTESIAN_POINT ( 'NONE',  ( -128.4459734468149179, 0.000000000000000000, -77.43171244307204404 ) ) ;
#45330 = LINE ( 'NONE', #41762, #25805 ) ;
#45331 = ORIENTED_EDGE ( 'NONE', *, *, #40644, .T. ) ;
#45332 = CARTESIAN_POINT ( 'NONE',  ( 31.55402655318503236, 0.000000000000000000, -117.4317124430720156 ) ) ;
#45333 = ORIENTED_EDGE ( 'NONE', *, *, #16790, .F. ) ;
#45334 = VERTEX_POINT ( 'NONE', #4817 ) ;
#45335 = CARTESIAN_POINT ( 'NONE',  ( 360.0000000000000568, 169.0000000000000284, 343.9999999999998863 ) ) ;
#45336 = ORIENTED_EDGE ( 'NONE', *, *, #34465, .T. ) ;
#45337 = CARTESIAN_POINT ( 'NONE',  ( 350.0000000000000000, -180.9999999999999716, -344.0000000000001705 ) ) ;
#45338 = FACE_OUTER_BOUND ( 'NONE', #17559, .T. ) ;
#45339 = VECTOR ( 'NONE', #21847, 1000.000000000000000 ) ;
#45340 = ORIENTED_EDGE ( 'NONE', *, *, #20861, .F. ) ;
#45341 = DIRECTION ( 'NONE',  ( 0.000000000000000000, 0.000000000000000000, -1.000000000000000000 ) ) ;
#45342 = VECTOR ( 'NONE', #40247, 1000.000000000000000 ) ;
#45343 = ADVANCED_FACE ( 'NONE', ( #39748 ), #35904, .F. ) ;
#45344 = DIRECTION ( 'NONE',  ( -1.000000000000000000, 0.000000000000000000, 0.000000000000000000 ) ) ;
#45345 = FACE_OUTER_BOUND ( 'NONE', #38316, .T. ) ;
#45346 = ORIENTED_EDGE ( 'NONE', *, *, #4500, .F. ) ;
#45347 = CARTESIAN_POINT ( 'NONE',  ( 14.49999999999999822, 12.98684210526315930, -19.37312575500899570 ) ) ;
#45348 = DIRECTION ( 'NONE',  ( 0.000000000000000000, 0.000000000000000000, -1.000000000000000000 ) ) ;
#45349 = AXIS2_PLACEMENT_3D ( 'NONE', #34895, #4081, #11276 ) ;
#45350 = CARTESIAN_POINT ( 'NONE',  ( -8.445973446814976526, 0.000000000000000000, 119.0682875569279418 ) ) ;
#45351 = VERTEX_POINT ( 'NONE', #47890 ) ;
#45352 = CARTESIAN_POINT ( 'NONE',  ( 75.05402655318509630, 2.143131898507880377E-16, -37.43171244307200141 ) ) ;
#45353 = CARTESIAN_POINT ( 'NONE',  ( -64.99999999999971578, 16.00000000000000000, -84.99999999999998579 ) ) ;
#45354 = ORIENTED_EDGE ( 'NONE', *, *, #16913, .T. ) ;
#45355 = VERTEX_POINT ( 'NONE', #38989 ) ;
#45356 = ORIENTED_EDGE ( 'NONE', *, *, #13886, .F. ) ;
#45357 = CARTESIAN_POINT ( 'NONE',  ( 135.0000000000019043, 16.00000000000000000, 90.00000000000000000 ) ) ;
#45358 = CARTESIAN_POINT ( 'NONE',  ( -19.99999999999971223, 17.00000000000000000, -84.99999999999998579 ) ) ;
#45359 = B_SPLINE_SURFACE_WITH_KNOTS ( 'NONE', 3, 3, ( 
 ( #45379, #5903, #2303, #29509 ),
 ( #10267, #36992, #9747, #18196 ),
 ( #44873, #44380, #49212, #14360 ),
 ( #5647, #13345, #21551, #2554 ) ),
 .UNSPECIFIED., .F., .F., .F.,
 ( 4, 4 ),
 ( 4, 4 ),
 ( 0.000000000000000000, 1.000000000000000000 ),
 ( 0.000000000000000000, 1.000000000000000000 ),
 .UNSPECIFIED. ) ;
#45360 = ORIENTED_EDGE ( 'NONE', *, *, #20861, .T. ) ;
#45361 = DIRECTION ( 'NONE',  ( 1.860490536778032451E-50, 0.000000000000000000, -1.000000000000000000 ) ) ;
#45362 = SURFACE_SIDE_STYLE ('',( #29748 ) ) ;
#45363 = FACE_BOUND ( 'NONE', #27332, .T. ) ;
#45364 = EDGE_CURVE ( 'NONE', #11132, #28586, #46913, .T. ) ;
#45365 = VECTOR ( 'NONE', #1249, 1000.000000000000000 ) ;
#45366 = CARTESIAN_POINT ( 'NONE',  ( -6.695973446814940111, 1.750000000000024203, 80.81828755692798438 ) ) ;
#45367 = ADVANCED_FACE ( 'NONE', ( #47637 ), #39242, .T. ) ;
#45368 = VERTEX_POINT ( 'NONE', #12275 ) ;
#45369 = CARTESIAN_POINT ( 'NONE',  ( 168.9999999999999716, -272.4999999999999432, -339.9999999999998863 ) ) ;
#45370 = CARTESIAN_POINT ( 'NONE',  ( 44.34968358615004291, 11.74141640735454928, -9.367992836599951190 ) ) ;
#45371 = EDGE_CURVE ( 'NONE', #23745, #9096, #45907, .T. ) ;
#45372 = LINE ( 'NONE', #29755, #13325 ) ;
#45373 = EDGE_LOOP ( 'NONE', ( #6471, #28106, #45086, #27658 ) ) ;
#45374 = EDGE_CURVE ( 'NONE', #11508, #37527, #4335, .T. ) ;
#45375 = EDGE_CURVE ( 'NONE', #50159, #43433, #28952, .T. ) ;
#45376 = CARTESIAN_POINT ( 'NONE',  ( 191.5540265531851105, 0.000000000000000000, -40.93171244307202983 ) ) ;
#45377 = CARTESIAN_POINT ( 'NONE',  ( 1.280882217648804167, -0.5301415400443709736, 9.960033073700794048 ) ) ;
#45378 = CIRCLE ( 'NONE', #12623, 2.000000000000001776 ) ;
#45379 = CARTESIAN_POINT ( 'NONE',  ( -36.08557433729205144, 35.58569447144795816, 7.455576670931136185 ) ) ;
#45380 = CARTESIAN_POINT ( 'NONE',  ( -126.6959734468149321, 1.749999999999997335, -119.1817124430720440 ) ) ;
#45381 = EDGE_LOOP ( 'NONE', ( #5250, #43472, #8563, #19361, #27695, #28901, #44852, #3664 ) ) ;
#45382 = DIRECTION ( 'NONE',  ( 0.000000000000000000, -1.000000000000000000, 0.000000000000000000 ) ) ;
#45383 = AXIS2_PLACEMENT_3D ( 'NONE', #45893, #14378, #10775 ) ;
#45384 = DIRECTION ( 'NONE',  ( 1.000000000000000000, -4.758098676964957447E-16, 2.958228394578795584E-31 ) ) ;
#45385 = EDGE_CURVE ( 'NONE', #38997, #23844, #44660, .T. ) ;
#45386 = DIRECTION ( 'NONE',  ( 0.000000000000000000, 0.000000000000000000, -1.000000000000000000 ) ) ;
#45387 = LINE ( 'NONE', #6661, #4494 ) ;
#45388 = VECTOR ( 'NONE', #28987, 1000.000000000000000 ) ;
#45389 = DIRECTION ( 'NONE',  ( 9.711650524620651178E-33, -1.223873602809432483E-48, 1.000000000000000000 ) ) ;
#45390 = VERTEX_POINT ( 'NONE', #42806 ) ;
#45391 = DIRECTION ( 'NONE',  ( 1.000000000000000000, 0.000000000000000000, 0.000000000000000000 ) ) ;
#45392 = EDGE_LOOP ( 'NONE', ( #9023, #6141, #47087, #33236, #48572, #45720 ) ) ;
#45393 = PLANE ( 'NONE',  #4869 ) ;
#45394 = EDGE_LOOP ( 'NONE', ( #22205, #160, #10946, #23428, #19077, #22232 ) ) ;
#45395 = CARTESIAN_POINT ( 'NONE',  ( 55.00000000000002132, -52.50000000000000711, -5.000000000000000000 ) ) ;
#45396 = FACE_OUTER_BOUND ( 'NONE', #46528, .T. ) ;
#45397 = FILL_AREA_STYLE ('',( #6181 ) ) ;
#45398 = ORIENTED_EDGE ( 'NONE', *, *, #27122, .T. ) ;
#45399 = VECTOR ( 'NONE', #46948, 1000.000000000000000 ) ;
#45400 = CARTESIAN_POINT ( 'NONE',  ( -1.540662627795934769, 1.371465786296043765, 9.894754715216725671 ) ) ;
#45401 = ORIENTED_EDGE ( 'NONE', *, *, #13089, .T. ) ;
#45402 = DIRECTION ( 'NONE',  ( 5.473822126268816076E-48, -1.000000000000000000, -1.654361225106055350E-24 ) ) ;
#45403 = CARTESIAN_POINT ( 'NONE',  ( -543.3973046169135159, 54.43801056904003133, -177.1374399499827916 ) ) ;
#45404 = CIRCLE ( 'NONE', #32453, 1.750000000000001554 ) ;
#45405 = LINE ( 'NONE', #49236, #20492 ) ;
#45406 = DIRECTION ( 'NONE',  ( -0.000000000000000000, -0.000000000000000000, -1.000000000000000000 ) ) ;
#45407 = CARTESIAN_POINT ( 'NONE',  ( 1.424123654779712922, 0.3625862473308184009, 9.958264684458541183 ) ) ;
#45408 = VERTEX_POINT ( 'NONE', #46881 ) ;
#45409 = VERTEX_POINT ( 'NONE', #27429 ) ;
#45410 = CARTESIAN_POINT ( 'NONE',  ( -50.11058929355266400, 7.578863168071933387, 7.455576670931136185 ) ) ;
#45411 = ADVANCED_FACE ( 'NONE', ( #19726 ), #35402, .T. ) ;
#45412 = ORIENTED_EDGE ( 'NONE', *, *, #2896, .F. ) ;
#45413 = VECTOR ( 'NONE', #15984, 1000.000000000000000 ) ;
#45414 = CARTESIAN_POINT ( 'NONE',  ( 357.9999999999999432, -181.0000000000000568, -356.0000000000002842 ) ) ;
#45415 = VERTEX_POINT ( 'NONE', #43315 ) ;
#45416 = CARTESIAN_POINT ( 'NONE',  ( -4.945973446814916130, -1.025126265847097207, 82.56828755692798438 ) ) ;
#45417 = ORIENTED_EDGE ( 'NONE', *, *, #47562, .T. ) ;
#45418 = VECTOR ( 'NONE', #4325, 1000.000000000000000 ) ;
#45419 = CARTESIAN_POINT ( 'NONE',  ( 6.619412807845094449, -7.495556955913033725, 9.646707543097347681 ) ) ;
#45420 = DIRECTION ( 'NONE',  ( -0.000000000000000000, -0.000000000000000000, -1.000000000000000000 ) ) ;
#45421 = CARTESIAN_POINT ( 'NONE',  ( 167.5000000000000000, 67.47808924524055385, -120.5992382549688955 ) ) ;
#45422 = CARTESIAN_POINT ( 'NONE',  ( 35.00000000000061107, 17.00000000000000000, -54.99999999999999289 ) ) ;
#45423 = VERTEX_POINT ( 'NONE', #36674 ) ;
#45424 = ORIENTED_EDGE ( 'NONE', *, *, #43790, .T. ) ;
#45425 = CARTESIAN_POINT ( 'NONE',  ( 181.0000000000000000, -81.49999999999995737, -115.0000000000001563 ) ) ;
#45426 = FACE_OUTER_BOUND ( 'NONE', #39093, .T. ) ;
#45427 = DIRECTION ( 'NONE',  ( -0.000000000000000000, -0.000000000000000000, -1.000000000000000000 ) ) ;
#45428 = DIRECTION ( 'NONE',  ( 1.000000000000000000, 1.156482317317870492E-16, 0.000000000000000000 ) ) ;
#45429 = VERTEX_POINT ( 'NONE', #44312 ) ;
#45430 = CARTESIAN_POINT ( 'NONE',  ( 112.2789002873379758, 1.749999999999996669, 41.84341382277508359 ) ) ;
#45431 = VERTEX_POINT ( 'NONE', #29441 ) ;
#45432 = ADVANCED_FACE ( 'NONE', ( #5335 ), #40496, .T. ) ;
#45433 =( NAMED_UNIT ( * ) PLANE_ANGLE_UNIT ( ) SI_UNIT ( $, .RADIAN. ) );
#45434 = EDGE_CURVE ( 'NONE', #47604, #7572, #16828, .T. ) ;
#45435 = DIRECTION ( 'NONE',  ( -0.000000000000000000, -0.000000000000000000, -1.000000000000000000 ) ) ;
#45436 = CYLINDRICAL_SURFACE ( 'NONE', #12930, 1.750000000000008438 ) ;
#45437 = CARTESIAN_POINT ( 'NONE',  ( 0.3370904143228959926, -0.2449105217885284291, 10.00000000000000000 ) ) ;
#45438 = VECTOR ( 'NONE', #40457, 1000.000000000000000 ) ;
#45439 = DIRECTION ( 'NONE',  ( 0.000000000000000000, 0.000000000000000000, 1.000000000000000000 ) ) ;
#45440 = FACE_OUTER_BOUND ( 'NONE', #49037, .T. ) ;
#45441 = CARTESIAN_POINT ( 'NONE',  ( 0.000000000000000000, 169.0000000000000000, 355.9999999999997726 ) ) ;
#45442 = ORIENTED_EDGE ( 'NONE', *, *, #42536, .F. ) ;
#45443 = EDGE_CURVE ( 'NONE', #16274, #11814, #39238, .T. ) ;
#45444 = DIRECTION ( 'NONE',  ( 0.000000000000000000, -1.000000000000000000, 0.000000000000000000 ) ) ;
#45445 = LINE ( 'NONE', #33691, #39220 ) ;
#45446 = CARTESIAN_POINT ( 'NONE',  ( 168.9999999999999716, 8.000000000000062172, -340.0000000000001137 ) ) ;
#45447 = CIRCLE ( 'NONE', #12736, 4.000000000000003553 ) ;
#45448 = CARTESIAN_POINT ( 'NONE',  ( -0.6108107228405769140, 1.056024183042602482, 9.963925895596188909 ) ) ;
#45449 = ORIENTED_EDGE ( 'NONE', *, *, #16272, .F. ) ;
#45450 = VECTOR ( 'NONE', #34350, 1000.000000000000000 ) ;
#45451 = LINE ( 'NONE', #49285, #12243 ) ;
#45452 = EDGE_LOOP ( 'NONE', ( #43977, #29335, #37702, #10355 ) ) ;
#45453 = CYLINDRICAL_SURFACE ( 'NONE', #43449, 1.750000000000001554 ) ;
#45454 = CARTESIAN_POINT ( 'NONE',  ( 114.3291528190321173, 1.749999999999996891, 121.8434138227750481 ) ) ;
#45455 =( GEOMETRIC_REPRESENTATION_CONTEXT ( 3 ) GLOBAL_UNCERTAINTY_ASSIGNED_CONTEXT ( ( #35517 ) ) GLOBAL_UNIT_ASSIGNED_CONTEXT ( ( #15432, #11329, #23124 ) ) REPRESENTATION_CONTEXT ( 'NONE', 'WORKASPACE' ) );
#45456 = FACE_OUTER_BOUND ( 'NONE', #47597, .T. ) ;
#45457 = ORIENTED_EDGE ( 'NONE', *, *, #10925, .F. ) ;
#45458 =( BOUNDED_CURVE ( )  B_SPLINE_CURVE ( 3, ( #32508, #4282, #47837, #28134 ),
 .UNSPECIFIED., .F., .F. ) 
 B_SPLINE_CURVE_WITH_KNOTS ( ( 4, 4 ),
 ( 4.712388980384684345, 6.058950556070484161 ),
 .UNSPECIFIED. ) 
 CURVE ( )  GEOMETRIC_REPRESENTATION_ITEM ( )  RATIONAL_B_SPLINE_CURVE ( ( 1.000000000000000000, 0.8545200852688803472, 0.8545200852688803472, 1.000000000000000000 ) ) 
 REPRESENTATION_ITEM ( '' )  );
#45459 = CARTESIAN_POINT ( 'NONE',  ( 15.39115647749017590, -6.484697992489784291, -9.458680755252684591 ) ) ;
#45460 = ORIENTED_EDGE ( 'NONE', *, *, #10307, .F. ) ;
#45461 = DIRECTION ( 'NONE',  ( -0.000000000000000000, -0.000000000000000000, -1.000000000000000000 ) ) ;
#45462 = DIRECTION ( 'NONE',  ( -0.000000000000000000, -0.000000000000000000, -1.000000000000000000 ) ) ;
#45463 = CARTESIAN_POINT ( 'NONE',  ( -4.945973446814903696, 2.143131898507912917E-16, 2.568287556928034121 ) ) ;
#45464 =( BOUNDED_CURVE ( )  B_SPLINE_CURVE ( 3, ( #44275, #5804, #48857, #9146 ),
 .UNSPECIFIED., .F., .F. ) 
 B_SPLINE_CURVE_WITH_KNOTS ( ( 4, 4 ),
 ( 1.570796326794896558, 3.141592653589793116 ),
 .UNSPECIFIED. ) 
 CURVE ( )  GEOMETRIC_REPRESENTATION_ITEM ( )  RATIONAL_B_SPLINE_CURVE ( ( 1.000000000000000000, 0.8047378541243649375, 0.8047378541243649375, 1.000000000000000000 ) ) 
 REPRESENTATION_ITEM ( '' )  );
#45465 = ORIENTED_EDGE ( 'NONE', *, *, #41016, .F. ) ;
#45466 = ORIENTED_EDGE ( 'NONE', *, *, #30867, .T. ) ;
#45467 = CARTESIAN_POINT ( 'NONE',  ( -5.930385588435886923, 41.38048276556310157, 8.846626183609801686 ) ) ;
#45468 = CARTESIAN_POINT ( 'NONE',  ( 16.02661358026014327, 4.530191650547718218, -9.683996418299976483 ) ) ;
#45469 = EDGE_CURVE ( 'NONE', #13512, #37466, #28686, .T. ) ;
#45470 = CIRCLE ( 'NONE', #30794, 1.750000000000015543 ) ;
#45471 = ORIENTED_EDGE ( 'NONE', *, *, #19909, .T. ) ;
#45472 = ORIENTED_EDGE ( 'NONE', *, *, #50675, .T. ) ;
#45473 = DIRECTION ( 'NONE',  ( 0.000000000000000000, 0.000000000000000000, 1.000000000000000000 ) ) ;
#45474 = CARTESIAN_POINT ( 'NONE',  ( -4.945973446814903696, 2.143131898507912917E-16, 165.0000000000000000 ) ) ;
#45475 = DIRECTION ( 'NONE',  ( 0.000000000000000000, 0.000000000000000000, 1.000000000000000000 ) ) ;
#45476 = VECTOR ( 'NONE', #43080, 1000.000000000000000 ) ;
#45477 = ORIENTED_EDGE ( 'NONE', *, *, #39052, .F. ) ;
#45478 = PLANE ( 'NONE',  #17767 ) ;
#45479 = EDGE_LOOP ( 'NONE', ( #1007, #47936, #15607, #11117 ) ) ;
#45480 = CIRCLE ( 'NONE', #20938, 1.750000000000001554 ) ;
#45481 =( BOUNDED_CURVE ( )  B_SPLINE_CURVE ( 3, ( #1368, #11900, #24465, #48007 ),
 .UNSPECIFIED., .F., .F. ) 
 B_SPLINE_CURVE_WITH_KNOTS ( ( 4, 4 ),
 ( 4.710277376051282359E-16, 1.570796326794896780 ),
 .UNSPECIFIED. ) 
 CURVE ( )  GEOMETRIC_REPRESENTATION_ITEM ( )  RATIONAL_B_SPLINE_CURVE ( ( 1.000000000000000000, 0.8047378541243650485, 0.8047378541243650485, 1.000000000000000000 ) ) 
 REPRESENTATION_ITEM ( '' )  );
#45482 = CARTESIAN_POINT ( 'NONE',  ( 164.9999999999999716, 15.00000000000000000, -114.9999999999999858 ) ) ;
#45484 = VECTOR ( 'NONE', #19142, 1000.000000000000000 ) ;
#45483 = CARTESIAN_POINT ( 'NONE',  ( 80.00000000000092371, 17.00000000000000000, -24.99999999999999289 ) ) ;
#45485 = B_SPLINE_CURVE_WITH_KNOTS ( 'NONE', 3,
 ( #32765, #47609, #24064, #36380 ),
 .UNSPECIFIED., .F., .F.,
 ( 4, 4 ),
 ( 0.0001535465953326492635, 0.0005837444810832899313 ),
 .UNSPECIFIED. ) ;
#45486 = AXIS2_PLACEMENT_3D ( 'NONE', #31923, #7813, #35026 ) ;
#45487 = ORIENTED_EDGE ( 'NONE', *, *, #2907, .T. ) ;
#45488 = VECTOR ( 'NONE', #15367, 1000.000000000000000 ) ;
#45489 = ORIENTED_EDGE ( 'NONE', *, *, #50257, .F. ) ;
#45490 = CARTESIAN_POINT ( 'NONE',  ( -1.104345476778524349, -0.6507740520594079703, 9.967237415621761798 ) ) ;
#45491 = DIRECTION ( 'NONE',  ( 1.000000000000000000, 0.000000000000000000, 0.000000000000000000 ) ) ;
#45492 = EDGE_LOOP ( 'NONE', ( #13452, #42855, #44136, #8861 ) ) ;
#45493 = CARTESIAN_POINT ( 'NONE',  ( 210.0000000000000568, 0.000000000000000000, 2.568287556927987048 ) ) ;
#45494 = ORIENTED_EDGE ( 'NONE', *, *, #28017, .F. ) ;
#45495 = AXIS2_PLACEMENT_3D ( 'NONE', #32799, #29199, #43821 ) ;
#45496 = CARTESIAN_POINT ( 'NONE',  ( 35.00000000000061107, 16.00000000000000000, -54.99999999999999289 ) ) ;
#45497 = FACE_OUTER_BOUND ( 'NONE', #48533, .T. ) ;
#45498 = ORIENTED_EDGE ( 'NONE', *, *, #2907, .F. ) ;
#45499 = CARTESIAN_POINT ( 'NONE',  ( -208.4459734468148611, 1.025126265847088991, 2.568287556927986159 ) ) ;
#45500 = DIRECTION ( 'NONE',  ( 0.000000000000000000, -0.000000000000000000, 1.000000000000000000 ) ) ;
#45501 = LINE ( 'NONE', #18073, #49735 ) ;
#45502 = CARTESIAN_POINT ( 'NONE',  ( -87.72109971266203843, 1.750000000000009548, -160.2068387089191219 ) ) ;
#45503 = CARTESIAN_POINT ( 'NONE',  ( -164.9459734468149463, -1.025126265847089657, -120.9317124430720440 ) ) ;
#45504 = EDGE_LOOP ( 'NONE', ( #20953, #22419 ) ) ;
#45505 = ADVANCED_FACE ( 'NONE', ( #9689 ), #13273, .T. ) ;
#45506 = DIRECTION ( 'NONE',  ( -0.000000000000000000, -0.000000000000000000, -1.000000000000000000 ) ) ;
#45507 = CARTESIAN_POINT ( 'NONE',  ( 113.3040265531850537, 0.000000000000000000, 165.0000000000000000 ) ) ;
#45508 = CARTESIAN_POINT ( 'NONE',  ( 73.30402655318508209, 0.000000000000000000, 165.0000000000000000 ) ) ;
#45509 = CARTESIAN_POINT ( 'NONE',  ( -15.45175104485246820, 6.222373774239106758, -2.870787844569587133 ) ) ;
#45510 = B_SPLINE_CURVE_WITH_KNOTS ( 'NONE', 3,
 ( #41229, #6084, #37415, #29684 ),
 .UNSPECIFIED., .F., .F.,
 ( 4, 4 ),
 ( 3.471140604459641645E-18, 8.326314924909149835E-06 ),
 .UNSPECIFIED. ) ;
#45511 = VECTOR ( 'NONE', #18484, 1000.000000000000000 ) ;
#45512 = DIRECTION ( 'NONE',  ( 1.000000000000000000, 0.000000000000000000, 0.000000000000000000 ) ) ;
#45513 = DIRECTION ( 'NONE',  ( -1.000000000000000000, -0.000000000000000000, -0.000000000000000000 ) ) ;
#45514 = VECTOR ( 'NONE', #27287, 1000.000000000000000 ) ;
#45515 = CARTESIAN_POINT ( 'NONE',  ( -0.5107275442771143092, -1.175643901748072873, 9.976582533991681601 ) ) ;
#45516 = CARTESIAN_POINT ( 'NONE',  ( 7.576114424932982594, -50.00000000000000711, 7.906207997025717304 ) ) ;
#45517 = EDGE_CURVE ( 'NONE', #19482, #6581, #688, .T. ) ;
#45518 = CARTESIAN_POINT ( 'NONE',  ( 39.35269538308637038, -42.31198943095992604, 742.8425600500171413 ) ) ;
#45519 = VECTOR ( 'NONE', #2134, 1000.000000000000000 ) ;
#45520 = LINE ( 'NONE', #10402, #31239 ) ;
#45521 = ADVANCED_FACE ( 'NONE', ( #9181 ), #44068, .T. ) ;
#45522 = ORIENTED_EDGE ( 'NONE', *, *, #45121, .F. ) ;
#45523 = VECTOR ( 'NONE', #43293, 1000.000000000000000 ) ;
#45524 = CARTESIAN_POINT ( 'NONE',  ( -14.29087950072019098, -9.652079258044555132, 8.727788335465566760 ) ) ;
#45525 = CARTESIAN_POINT ( 'NONE',  ( 151.5540265531850537, -1.025126265847089657, 42.56828755692799149 ) ) ;
#45526 = CARTESIAN_POINT ( 'NONE',  ( 13.59579750444771307, -10.60877755095900632, 8.727788335465566760 ) ) ;
#45527 = ORIENTED_EDGE ( 'NONE', *, *, #29276, .T. ) ;
#45528 = EDGE_CURVE ( 'NONE', #9801, #12079, #33312, .T. ) ;
#45530 = ORIENTED_EDGE ( 'NONE', *, *, #11868, .T. ) ;
#45529 = EDGE_CURVE ( 'NONE', #9207, #10844, #6092, .T. ) ;
#45531 = LINE ( 'NONE', #49362, #45532 ) ;
#45532 = VECTOR ( 'NONE', #14249, 1000.000000000000114 ) ;
#45533 = CARTESIAN_POINT ( 'NONE',  ( 181.0000000000000284, -272.5000000000000000, -96.99999999999988631 ) ) ;
#45534 = EDGE_CURVE ( 'NONE', #30766, #12663, #4294, .T. ) ;
#45535 = ORIENTED_EDGE ( 'NONE', *, *, #8693, .F. ) ;
#45536 = CARTESIAN_POINT ( 'NONE',  ( 7.576114424932982594, -33.14742743729794938, 7.906207997025717304 ) ) ;
#45537 = LINE ( 'NONE', #22468, #28208 ) ;
#45538 = VERTEX_POINT ( 'NONE', #9435 ) ;
#45539 = ORIENTED_EDGE ( 'NONE', *, *, #10236, .T. ) ;
#45540 = ORIENTED_EDGE ( 'NONE', *, *, #30901, .F. ) ;
#45541 = CARTESIAN_POINT ( 'NONE',  ( -206.6959734468149463, 1.750000000000010214, -39.18171244307202983 ) ) ;
#45542 = CARTESIAN_POINT ( 'NONE',  ( 50.11058929355270664, -7.578863168071591438, 7.455576670931136185 ) ) ;
#45543 = CARTESIAN_POINT ( 'NONE',  ( 22.69295089195473736, 45.31600496604706052, 7.455576670931136185 ) ) ;
#45544 = VECTOR ( 'NONE', #45723, 1000.000000000000000 ) ;
#45545 = EDGE_LOOP ( 'NONE', ( #10528, #40732, #9860, #3963 ) ) ;
#45546 = CARTESIAN_POINT ( 'NONE',  ( 4.672045878990125800, -50.00000000000000711, 1.847720168420772691 ) ) ;
#45547 = AXIS2_PLACEMENT_3D ( 'NONE', #1597, #40597, #37279 ) ;
#45548 = LINE ( 'NONE', #10427, #3394 ) ;
#45549 = VERTEX_POINT ( 'NONE', #24589 ) ;
#45550 = AXIS2_PLACEMENT_3D ( 'NONE', #8113, #42724, #35079 ) ;
#45551 = ORIENTED_EDGE ( 'NONE', *, *, #5098, .F. ) ;
#45552 = CARTESIAN_POINT ( 'NONE',  ( 84.99999999999997158, 17.00000000000000000, -114.9999999999999858 ) ) ;
#45553 = CARTESIAN_POINT ( 'NONE',  ( -15.62858259096117841, 5.755205073598721910, -9.683996418299976483 ) ) ;
#45554 = CARTESIAN_POINT ( 'NONE',  ( 341.9999999999999432, -180.9999999999999716, 355.9999999999998295 ) ) ;
#45555 = VERTEX_POINT ( 'NONE', #5070 ) ;
#45556 = ADVANCED_FACE ( 'NONE', ( #40748 ), #1745, .T. ) ;
#45557 = LINE ( 'NONE', #1984, #19214 ) ;
#45558 = LINE ( 'NONE', #22741, #48480 ) ;
#45559 = AXIS2_PLACEMENT_3D ( 'NONE', #32650, #48498, #5689 ) ;
#45560 = ADVANCED_FACE ( 'NONE', ( #16897 ), #33052, .T. ) ;
#45561 = DIRECTION ( 'NONE',  ( -0.000000000000000000, -1.000000000000000000, -0.000000000000000000 ) ) ;
#45562 = DIRECTION ( 'NONE',  ( 0.000000000000000000, 0.000000000000000000, 1.000000000000000000 ) ) ;
#45563 = ADVANCED_FACE ( 'NONE', ( #48638 ), #5842, .F. ) ;
#45564 = AXIS2_PLACEMENT_3D ( 'NONE', #27984, #28248, #8755 ) ;
#45565 = CARTESIAN_POINT ( 'NONE',  ( -206.6959734468149463, 1.750000000000010658, -79.18171244307201562 ) ) ;
#45566 = ORIENTED_EDGE ( 'NONE', *, *, #32054, .F. ) ;
#45567 = FILL_AREA_STYLE ('',( #18383 ) ) ;
#45568 = ADVANCED_FACE ( 'NONE', ( #1993 ), #3488, .T. ) ;
#45569 = DIRECTION ( 'NONE',  ( 1.000000000000000000, 0.000000000000000000, 0.000000000000000000 ) ) ;
#45570 = CARTESIAN_POINT ( 'NONE',  ( -14.99999999999970868, 17.00000000000000000, -84.99999999999998579 ) ) ;
#45571 = CARTESIAN_POINT ( 'NONE',  ( -164.9459734468149463, -1.025126265847089213, -160.9317124430720014 ) ) ;
#45572 = EDGE_CURVE ( 'NONE', #25937, #13970, #19145, .T. ) ;
#45573 = AXIS2_PLACEMENT_3D ( 'NONE', #44902, #25444, #17744 ) ;
#45574 = DIRECTION ( 'NONE',  ( 0.000000000000000000, 0.000000000000000000, -1.000000000000000000 ) ) ;
#45575 = CARTESIAN_POINT ( 'NONE',  ( -3.222683565149130569, -0.4845875505058497290, 9.799352050262461589 ) ) ;
#45576 = ORIENTED_EDGE ( 'NONE', *, *, #6529, .T. ) ;
#45577 = DIRECTION ( 'NONE',  ( 0.000000000000000000, -1.000000000000000000, 0.000000000000000000 ) ) ;
#45578 = CARTESIAN_POINT ( 'NONE',  ( -44.99506233596265048, -23.32283626942287569, 7.455576670931136185 ) ) ;
#45579 = CARTESIAN_POINT ( 'NONE',  ( 181.0000000000000568, 175.0000000000000284, 343.9999999999998863 ) ) ;
#45580 = ORIENTED_EDGE ( 'NONE', *, *, #23748, .F. ) ;
#45581 = DIRECTION ( 'NONE',  ( -1.000000000000000000, -0.000000000000000000, -0.000000000000000000 ) ) ;
#45582 = VECTOR ( 'NONE', #5621, 1000.000000000000000 ) ;
#45583 = CARTESIAN_POINT ( 'NONE',  ( 85.00000000000213163, 17.00000000000000000, 95.00000000000000000 ) ) ;
#45584 = EDGE_LOOP ( 'NONE', ( #41668, #15225, #24173, #26138, #39298, #12559 ) ) ;
#45585 = DIRECTION ( 'NONE',  ( 1.000000000000000000, 0.000000000000000000, -9.251858538542979716E-16 ) ) ;
#45586 = DIRECTION ( 'NONE',  ( 0.000000000000000000, 0.000000000000000000, 1.000000000000000000 ) ) ;
#45587 = CARTESIAN_POINT ( 'NONE',  ( 14.49999999999999822, 12.98684210526315930, -19.37312575500900280 ) ) ;
#45588 = CARTESIAN_POINT ( 'NONE',  ( 343.9999999999993747, 183.0000000000000568, 357.9999999999998295 ) ) ;
#45589 = ORIENTED_EDGE ( 'NONE', *, *, #7832, .F. ) ;
#45590 = LINE ( 'NONE', #41764, #16700 ) ;
#45591 = EDGE_CURVE ( 'NONE', #21384, #21938, #22752, .T. ) ;
#45593 = VERTEX_POINT ( 'NONE', #37665 ) ;
#45592 = EDGE_CURVE ( 'NONE', #38490, #8483, #6595, .T. ) ;
#45594 = VERTEX_POINT ( 'NONE', #46322 ) ;
#45595 = DIRECTION ( 'NONE',  ( 0.000000000000000000, 0.000000000000000000, 1.000000000000000000 ) ) ;
#45596 = EDGE_CURVE ( 'NONE', #40426, #31866, #50174, .T. ) ;
#45597 = EDGE_CURVE ( 'NONE', #16490, #12746, #18135, .T. ) ;
#45598 = VERTEX_POINT ( 'NONE', #46059 ) ;
#45599 = DIRECTION ( 'NONE',  ( 0.000000000000000000, 0.000000000000000000, 1.000000000000000000 ) ) ;
#45600 = CARTESIAN_POINT ( 'NONE',  ( 0.000000000000000000, 0.000000000000000000, 15.00000000000000000 ) ) ;
#45601 = CARTESIAN_POINT ( 'NONE',  ( 15.00099850811936264, 7.462898891544210933, 9.403735324607438884 ) ) ;
#45602 = EDGE_CURVE ( 'NONE', #4602, #46359, #33810, .T. ) ;
#45603 = PLANE ( 'NONE',  #9218 ) ;
#45604 = EDGE_CURVE ( 'NONE', #41095, #22082, #18883, .T. ) ;
#45605 = PLANE ( 'NONE',  #25980 ) ;
#45606 = VERTEX_POINT ( 'NONE', #3236 ) ;
#45607 = CARTESIAN_POINT ( 'NONE',  ( -1.011271242968677875, -0.7347315653656004697, 10.00000000000000000 ) ) ;
#45608 = CARTESIAN_POINT ( 'NONE',  ( -86.69597344681494633, 1.750000000000010658, 80.81828755692798438 ) ) ;
#45609 = DIRECTION ( 'NONE',  ( 0.000000000000000000, 0.000000000000000000, -1.000000000000000000 ) ) ;
#45610 = ORIENTED_EDGE ( 'NONE', *, *, #13294, .T. ) ;
#45611 = DIRECTION ( 'NONE',  ( 0.000000000000000000, -1.000000000000000000, 0.000000000000000000 ) ) ;
#45612 = CARTESIAN_POINT ( 'NONE',  ( -48.44597344681495343, 0.000000000000000000, 165.0000000000000000 ) ) ;
#45613 = VERTEX_POINT ( 'NONE', #49888 ) ;
#45614 = ORIENTED_EDGE ( 'NONE', *, *, #30059, .T. ) ;
#45615 = VERTEX_POINT ( 'NONE', #10951 ) ;
#45616 = PLANE ( 'NONE',  #9827 ) ;
#45617 = CARTESIAN_POINT ( 'NONE',  ( 341.9999999999999432, -181.0000000000001421, 356.0000000000000568 ) ) ;
#45618 = ORIENTED_EDGE ( 'NONE', *, *, #296, .F. ) ;
#45619 = ADVANCED_FACE ( 'NONE', ( #42250 ), #26606, .F. ) ;
#45620 = DIRECTION ( 'NONE',  ( -1.000000000000000000, -0.000000000000000000, -0.000000000000000000 ) ) ;
#45621 = CARTESIAN_POINT ( 'NONE',  ( -5.000000000000000000, -184.7999999999999545, -340.2000000000001592 ) ) ;
#45622 = EDGE_CURVE ( 'NONE', #18731, #302, #30719, .T. ) ;
#45623 = CARTESIAN_POINT ( 'NONE',  ( 193.3040265531851105, -1.750000000000009992, 0.8182875569279768335 ) ) ;
#45624 = AXIS2_PLACEMENT_3D ( 'NONE', #9996, #34123, #49202 ) ;
#45625 = EDGE_CURVE ( 'NONE', #42991, #27084, #26092, .T. ) ;
#45626 = ORIENTED_EDGE ( 'NONE', *, *, #31534, .T. ) ;
#45627 = CARTESIAN_POINT ( 'NONE',  ( 5.551115123125782702E-14, -180.9999999999999716, 355.9999999999997726 ) ) ;
#45628 =( BOUNDED_CURVE ( )  B_SPLINE_CURVE ( 3, ( #22658, #3406, #3665, #27018 ),
 .UNSPECIFIED., .F., .F. ) 
 B_SPLINE_CURVE_WITH_KNOTS ( ( 4, 4 ),
 ( 0.000000000000000000, 1.570796326794896558 ),
 .UNSPECIFIED. ) 
 CURVE ( )  GEOMETRIC_REPRESENTATION_ITEM ( )  RATIONAL_B_SPLINE_CURVE ( ( 1.000000000000000000, 0.8047378541243649375, 0.8047378541243649375, 1.000000000000000000 ) ) 
 REPRESENTATION_ITEM ( '' )  );
#45629 = CARTESIAN_POINT ( 'NONE',  ( -0.3896797354171960270, 1.262193838292709147, 9.943883492372847854 ) ) ;
#45630 = ORIENTED_EDGE ( 'NONE', *, *, #48967, .F. ) ;
#45631 = CARTESIAN_POINT ( 'NONE',  ( -205.6708471809678827, -1.750000000000009548, -40.20683870891912193 ) ) ;
#45632 = LINE ( 'NONE', #41306, #1320 ) ;
#45633 = CARTESIAN_POINT ( 'NONE',  ( -124.9459734468149321, -1.025126265847081664, 122.5682875569279702 ) ) ;
#45634 = CARTESIAN_POINT ( 'NONE',  ( 14.49999999999999822, -46.12433806312137108, -6.404467680894764925 ) ) ;
#45635 = VERTEX_POINT ( 'NONE', #37922 ) ;
#45636 = DIRECTION ( 'NONE',  ( -0.1671032855531317807, -0.5142910309547739089, 0.8411784753765542133 ) ) ;
#45637 = EDGE_CURVE ( 'NONE', #2900, #23819, #18385, .T. ) ;
#45638 = CARTESIAN_POINT ( 'NONE',  ( 5.888214538810389698, 16.20866436362417673, 8.727788335465566760 ) ) ;
#45639 = CARTESIAN_POINT ( 'NONE',  ( 0.3862712429686727678, 1.188820645368945605, 10.00000000000000000 ) ) ;
#45640 = CARTESIAN_POINT ( 'NONE',  ( -88.44597344681497475, 0.000000000000000000, 165.0000000000000000 ) ) ;
#45641 = FACE_OUTER_BOUND ( 'NONE', #47283, .T. ) ;
#45642 = EDGE_LOOP ( 'NONE', ( #42622, #30069, #20867, #50177, #36699, #15555 ) ) ;
#45643 = ORIENTED_EDGE ( 'NONE', *, *, #24583, .T. ) ;
#45644 = FACE_OUTER_BOUND ( 'NONE', #49984, .T. ) ;
#45645 = EDGE_CURVE ( 'NONE', #41652, #8390, #4693, .T. ) ;
#45646 = VERTEX_POINT ( 'NONE', #50147 ) ;
#45647 = CARTESIAN_POINT ( 'NONE',  ( 50.24128791297869867, -41.04536285977715693, 5.000000000000000000 ) ) ;
#45648 = VERTEX_POINT ( 'NONE', #6346 ) ;
#45649 = FACE_OUTER_BOUND ( 'NONE', #15226, .T. ) ;
#45650 = EDGE_LOOP ( 'NONE', ( #13279, #46206, #39910, #6357 ) ) ;
#45651 = EDGE_CURVE ( 'NONE', #15590, #16798, #30194, .T. ) ;
#45652 = LINE ( 'NONE', #29528, #48218 ) ;
#45653 = EDGE_CURVE ( 'NONE', #44283, #1426, #26356, .T. ) ;
#45654 = VERTEX_POINT ( 'NONE', #22498 ) ;
#45655 = DIRECTION ( 'NONE',  ( 1.000000000000000000, 0.000000000000000000, 1.586032872232979935E-16 ) ) ;
#45656 = CARTESIAN_POINT ( 'NONE',  ( 135.0000000000015632, 16.00000000000000000, 35.00000000000000000 ) ) ;
#45657 = FACE_OUTER_BOUND ( 'NONE', #17221, .T. ) ;
#45658 = CARTESIAN_POINT ( 'NONE',  ( -14.49999999999999822, -46.12433806312137108, 6.404467680894761372 ) ) ;
#45659 = CARTESIAN_POINT ( 'NONE',  ( -44.94597344681493922, 1.025126265847089435, 2.568287556927986159 ) ) ;
#45660 = B_SPLINE_CURVE_WITH_KNOTS ( 'NONE', 3,
 ( #40566, #40317, #21823, #21059 ),
 .UNSPECIFIED., .F., .F.,
 ( 4, 4 ),
 ( 1.084202172485504627E-18, 0.0002708531562908071634 ),
 .UNSPECIFIED. ) ;
#45661 = VERTEX_POINT ( 'NONE', #38175 ) ;
#45662 = EDGE_CURVE ( 'NONE', #38893, #24608, #2991, .T. ) ;
#45663 = VERTEX_POINT ( 'NONE', #31990 ) ;
#45664 = CYLINDRICAL_SURFACE ( 'NONE', #538, 1.750000000000015543 ) ;
#45665 = EDGE_CURVE ( 'NONE', #25205, #37687, #15962, .T. ) ;
#45666 = EDGE_CURVE ( 'NONE', #30495, #39140, #4017, .T. ) ;
#45667 = ORIENTED_EDGE ( 'NONE', *, *, #35889, .F. ) ;
#45668 = CARTESIAN_POINT ( 'NONE',  ( -0.8282505383454070724, -1.889063466747028297, 9.894754715216727448 ) ) ;
#45669 = CARTESIAN_POINT ( 'NONE',  ( 167.5000000000000000, -112.5000000000000000, -10.00000000000000000 ) ) ;
#45670 = VERTEX_POINT ( 'NONE', #19665 ) ;
#45671 = DIRECTION ( 'NONE',  ( -0.000000000000000000, -0.000000000000000000, -1.000000000000000000 ) ) ;
#45672 = ADVANCED_FACE ( 'NONE', ( #38934 ), #43765, .T. ) ;
#45673 = LINE ( 'NONE', #26210, #36618 ) ;
#45674 = B_SPLINE_SURFACE_WITH_KNOTS ( 'NONE', 3, 3, ( 
 ( #7068, #6312, #6805, #10407 ),
 ( #26058, #41706, #22209, #19368 ),
 ( #34793, #47032, #15279, #16284 ),
 ( #7838, #15766, #8087, #27325 ) ),
 .UNSPECIFIED., .F., .F., .F.,
 ( 4, 4 ),
 ( 4, 4 ),
 ( 0.000000000000000000, 1.000000000000000000 ),
 ( 0.000000000000000000, 1.000000000000000000 ),
 .UNSPECIFIED. ) ;
#45675 = ORIENTED_EDGE ( 'NONE', *, *, #44450, .T. ) ;
#45676 = DIRECTION ( 'NONE',  ( -1.000000000000000000, -0.000000000000000000, -0.000000000000000000 ) ) ;
#45677 = FACE_OUTER_BOUND ( 'NONE', #6999, .T. ) ;
#45678 = CARTESIAN_POINT ( 'NONE',  ( -8.813458710706198573, -4.724716452304520864, 0.000000000000000000 ) ) ;
#45679 = CARTESIAN_POINT ( 'NONE',  ( -204.9459734468149463, 2.143131898507880377E-16, 165.0000000000000000 ) ) ;
#45680 = EDGE_LOOP ( 'NONE', ( #16403, #38276, #30687, #6062 ) ) ;
#45681 = LINE ( 'NONE', #10559, #7588 ) ;
#45682 = ORIENTED_EDGE ( 'NONE', *, *, #1240, .T. ) ;
#45683 = ORIENTED_EDGE ( 'NONE', *, *, #50042, .T. ) ;
#45684 = CARTESIAN_POINT ( 'NONE',  ( 861.4995338189738732, 844.4032370507319456, 1685.986414963429525 ) ) ;
#45685 = CARTESIAN_POINT ( 'NONE',  ( 194.3291528190321742, -1.750000000000009548, -118.1565861772249519 ) ) ;
#45686 = CARTESIAN_POINT ( 'NONE',  ( -88.44597344681497475, 0.000000000000000000, 165.0000000000000000 ) ) ;
#45687 = CARTESIAN_POINT ( 'NONE',  ( 115.0540265531850395, 1.025126265847081886, 79.06828755692797017 ) ) ;
#45688 = AXIS2_PLACEMENT_3D ( 'NONE', #13899, #13666, #5962 ) ;
#45689 = CARTESIAN_POINT ( 'NONE',  ( 164.9999999999999716, 165.0000000000000000, -356.0000000000001705 ) ) ;
#45690 = CYLINDRICAL_SURFACE ( 'NONE', #14291, 1.750000000000015543 ) ;
#45691 = DIRECTION ( 'NONE',  ( -0.000000000000000000, -0.000000000000000000, -1.000000000000000000 ) ) ;
#45692 = ORIENTED_EDGE ( 'NONE', *, *, #42443, .T. ) ;
#45693 = CARTESIAN_POINT ( 'NONE',  ( 196.8526953830863420, 160.1880105690400455, 472.8425600500170844 ) ) ;
#45694 = LINE ( 'NONE', #25477, #10517 ) ;
#45695 = CARTESIAN_POINT ( 'NONE',  ( 42.99990394833793061, 47.95759300784327905, 5.000000000000000000 ) ) ;
#45696 = EDGE_CURVE ( 'NONE', #42074, #48180, #8384, .T. ) ;
#45697 = SURFACE_STYLE_FILL_AREA ( #3124 ) ;
#45698 = ORIENTED_EDGE ( 'NONE', *, *, #49060, .T. ) ;
#45699 = SHAPE_REPRESENTATION ( 'MAT-058', ( #10261, #41389, #24228, #27478, #29921, #31598, #47092, #30780, #17649, #26669, #16022, #16818, #19249, #5345, #1262, #8659, #44653 ), #45455 ) ;
#45700 = DIRECTION ( 'NONE',  ( 0.000000000000000000, -1.000000000000000000, -3.186989995019654210E-49 ) ) ;
#45701 = ORIENTED_EDGE ( 'NONE', *, *, #49158, .F. ) ;
#45702 = DIRECTION ( 'NONE',  ( 0.000000000000000000, -0.000000000000000000, -1.000000000000000000 ) ) ;
#45703 = DIRECTION ( 'NONE',  ( -0.000000000000000000, -0.000000000000000000, -1.000000000000000000 ) ) ;
#45704 = CARTESIAN_POINT ( 'NONE',  ( 168.9999999999999716, 10.00000000000006395, 339.9999999999998295 ) ) ;
#45705 = ORIENTED_EDGE ( 'NONE', *, *, #48476, .F. ) ;
#45706 = EDGE_CURVE ( 'NONE', #39770, #5307, #4768, .T. ) ;
#45707 = EDGE_CURVE ( 'NONE', #22662, #9652, #47072, .T. ) ;
#45708 = CARTESIAN_POINT ( 'NONE',  ( 181.0000000000000000, 6.000000000000060396, -340.0000000000001137 ) ) ;
#45709 = ORIENTED_EDGE ( 'NONE', *, *, #46157, .F. ) ;
#45710 = DIRECTION ( 'NONE',  ( -1.000000000000000000, -0.000000000000000000, -0.000000000000000000 ) ) ;
#45711 = FACE_OUTER_BOUND ( 'NONE', #7615, .T. ) ;
#45712 = DIRECTION ( 'NONE',  ( -0.000000000000000000, -0.000000000000000000, -1.000000000000000000 ) ) ;
#45713 = ORIENTED_EDGE ( 'NONE', *, *, #39100, .T. ) ;
#45714 = VERTEX_POINT ( 'NONE', #47330 ) ;
#45715 = CARTESIAN_POINT ( 'NONE',  ( -6.174150299305392053, 45.68101107938186800, 8.807470649214879543 ) ) ;
#45716 = CARTESIAN_POINT ( 'NONE',  ( -125.6708471809678542, 1.749999999999996669, -38.15658617722495194 ) ) ;
#45717 = EDGE_CURVE ( 'NONE', #13126, #16395, #7995, .T. ) ;
#45718 = ADVANCED_FACE ( 'NONE', ( #12466 ), #30978, .F. ) ;
#45719 = AXIS2_PLACEMENT_3D ( 'NONE', #33940, #48785, #17277 ) ;
#45720 = ORIENTED_EDGE ( 'NONE', *, *, #4498, .T. ) ;
#45721 = ORIENTED_EDGE ( 'NONE', *, *, #26476, .F. ) ;
#45722 = CARTESIAN_POINT ( 'NONE',  ( -84.94597344681494633, 2.143131898507880377E-16, -77.43171244307204404 ) ) ;
#45723 = DIRECTION ( 'NONE',  ( -0.000000000000000000, -1.000000000000000000, -0.000000000000000000 ) ) ;
#45724 = CARTESIAN_POINT ( 'NONE',  ( -165.0000000000000284, 17.00000000000000000, -90.00000000000000000 ) ) ;
#45725 = ORIENTED_EDGE ( 'NONE', *, *, #25355, .F. ) ;
#45726 = DIRECTION ( 'NONE',  ( 1.000000000000000000, 0.000000000000000000, 0.000000000000000000 ) ) ;
#45727 = EDGE_CURVE ( 'NONE', #10604, #45654, #22355, .T. ) ;
#45728 = ORIENTED_EDGE ( 'NONE', *, *, #39396, .F. ) ;
#45729 = CLOSED_SHELL ( 'NONE', ( #44240, #31802, #22064, #35000, #9328, #9934, #42420, #32460, #22620, #15668, #10745, #34633, #43427, #774, #22845, #11394, #41899, #32137, #41999, #235, #31906, #25404, #47925, #41187, #1986, #4861, #11327, #26242, #10228, #11127, #20619, #8879, #34027, #21534, #35699, #45619, #32134, #2156, #17349, #22808, #5832, #15596, #37283, #46428, #37333, #5089, #11296, #44328, #40328, #22395, #26483, #22182, #5969, #41919, #9535, #18753, #30010, #1386, #22302, #30530, #25031, #2934, #14509, #48088, #42479, #26201, #9384, #33771, #27440, #24331, #15136, #39449, #180, #28718, #17038, #3705, #20267, #15923, #7657, #42392, #40132, #37815, #19096, #12021, #36823, #44336, #34768, #25035, #50663, #31885, #31927, #42419, #49655, #5149, #29175, #11375, #26294, #46398, #7668, #41496, #2340, #26153, #9323, #30242, #21470, #44590, #13344, #31647, #49477, #41256, #40444, #35309, #941, #16912, #14365, #31328, #45311, #31487, #28442, #26852, #11979, #28282, #27126, #19826, #10935, #43257, #7655, #49051, #41978, #46867, #36481, #12444, #12142, #34776, #13367, #40627, #14197, #28080, #24930, #48955, #50692, #17296, #6184, #34997, #4053, #47509, #43140, #10576, #36049, #14592, #42614, #12022, #18967, #10007, #43728, #29354, #21243, #47081, #38833, #30926, #30854, #35838, #42311, #45150, #41976, #20958, #29057, #553, #21285, #18284, #43418, #41529, #32115, #29490, #47725, #22520, #28969, #29923, #46510, #21757, #10173, #1691, #37495, #8315, #47157, #4859, #48385, #42495, #49220, #30198, #8939, #24027, #11517, #20514, #8870, #45343, #42140, #33682, #29706, #12197, #35117, #44686, #11866, #17133, #16279, #31057, #32694, #1697, #18265, #41537, #4689, #10971, #34714, #2756, #12398, #45014, #34616, #7692, #34402, #4649, #22138, #465, #4798, #22872, #20028, #23356, #6900, #33148, #21544, #6039, #32139, #39747, #22274, #46832, #32171, #8339, #46550, #41101, #47059, #10403, #24950, #17773, #41787, #26475, #31567, #32270, #30871, #33071, #5125, #12685, #34335, #39240, #22811, #11010, #24111, #437, #3141, #17730, #32779, #20680, #36836 ) ) ;
#45730 = LINE ( 'NONE', #10611, #17670 ) ;
#45731 = LINE ( 'NONE', #15240, #34551 ) ;
#45732 = ORIENTED_EDGE ( 'NONE', *, *, #26524, .T. ) ;
#45733 = ORIENTED_EDGE ( 'NONE', *, *, #18732, .F. ) ;
#45734 = ORIENTED_EDGE ( 'NONE', *, *, #44325, .T. ) ;
#45735 = CARTESIAN_POINT ( 'NONE',  ( -4.999999999999997335, 204.9999999999999716, -230.2499999999999716 ) ) ;
#45736 = CARTESIAN_POINT ( 'NONE',  ( -0.3862712429686895876, 1.188820645368940720, 10.00000000000000000 ) ) ;
#45737 = EDGE_LOOP ( 'NONE', ( #9141, #31198, #34856, #6666 ) ) ;
#45738 = CARTESIAN_POINT ( 'NONE',  ( -14.99999999999906919, 16.00000000000000000, -24.99999999999999289 ) ) ;
#45739 = ORIENTED_EDGE ( 'NONE', *, *, #49313, .F. ) ;
#45740 = DIRECTION ( 'NONE',  ( -1.000000000000000000, 0.000000000000000000, -2.958228394578794270E-31 ) ) ;
#45741 = ORIENTED_EDGE ( 'NONE', *, *, #10217, .F. ) ;
#45742 = CARTESIAN_POINT ( 'NONE',  ( 31.55402655318503236, 0.000000000000000000, 159.0682875569279702 ) ) ;
#45743 = CARTESIAN_POINT ( 'NONE',  ( 1.540526284687965264, -1.371707213411490267, 9.886433018048071730 ) ) ;
#45744 = DIRECTION ( 'NONE',  ( -0.9510565162951500895, -0.3090169943749582759, 0.000000000000000000 ) ) ;
#45745 = CARTESIAN_POINT ( 'NONE',  ( -88.44597344681491791, 2.143131898507880377E-16, -160.9317124430720298 ) ) ;
#45746 = CARTESIAN_POINT ( 'NONE',  ( -5.000000000000000000, 184.8000000000000114, 359.7999999999997840 ) ) ;
#45747 = ORIENTED_EDGE ( 'NONE', *, *, #4090, .T. ) ;
#45748 = CARTESIAN_POINT ( 'NONE',  ( -5.000000000000000000, -175.0000000000000284, -350.0000000000002274 ) ) ;
#45749 = EDGE_CURVE ( 'NONE', #30761, #16247, #23776, .T. ) ;
#45750 = CYLINDRICAL_SURFACE ( 'NONE', #6808, 1.750000000000015543 ) ;
#45751 = DIRECTION ( 'NONE',  ( -1.000000000000000000, -0.000000000000000000, -0.000000000000000000 ) ) ;
#45752 = LINE ( 'NONE', #3702, #14413 ) ;
#45753 = ADVANCED_FACE ( 'NONE', ( #24291 ), #11463, .T. ) ;
#45754 = VECTOR ( 'NONE', #18315, 1000.000000000000000 ) ;
#45755 =( BOUNDED_CURVE ( )  B_SPLINE_CURVE ( 3, ( #49723, #30276, #45886, #39001 ),
 .UNSPECIFIED., .F., .F. ) 
 B_SPLINE_CURVE_WITH_KNOTS ( ( 4, 4 ),
 ( 1.570796326794896558, 3.141592653589793116 ),
 .UNSPECIFIED. ) 
 CURVE ( )  GEOMETRIC_REPRESENTATION_ITEM ( )  RATIONAL_B_SPLINE_CURVE ( ( 1.000000000000000000, 0.8047378541243649375, 0.8047378541243649375, 1.000000000000000000 ) ) 
 REPRESENTATION_ITEM ( '' )  );
#45756 = AXIS2_PLACEMENT_3D ( 'NONE', #18015, #25224, #21887 ) ;
#45757 = FACE_OUTER_BOUND ( 'NONE', #49574, .T. ) ;
#45758 = CARTESIAN_POINT ( 'NONE',  ( 181.0000000000000000, -9.999999999999953815, -340.0000000000001137 ) ) ;
#45759 = CARTESIAN_POINT ( 'NONE',  ( 151.5540265531850537, -1.025126265847089213, -0.9317124430720324924 ) ) ;
#45760 = CIRCLE ( 'NONE', #9750, 1.750000000000008438 ) ;
#45761 = VECTOR ( 'NONE', #11257, 1000.000000000000000 ) ;
#45762 = DIRECTION ( 'NONE',  ( 1.000000000000000000, -0.000000000000000000, -0.000000000000000000 ) ) ;
#45763 =( BOUNDED_CURVE ( )  B_SPLINE_CURVE ( 3, ( #32884, #37253, #17220, #5911 ),
 .UNSPECIFIED., .F., .F. ) 
 B_SPLINE_CURVE_WITH_KNOTS ( ( 4, 4 ),
 ( 3.141592653589793116, 4.712388980384689674 ),
 .UNSPECIFIED. ) 
 CURVE ( )  GEOMETRIC_REPRESENTATION_ITEM ( )  RATIONAL_B_SPLINE_CURVE ( ( 1.000000000000000000, 0.8047378541243649375, 0.8047378541243649375, 1.000000000000000000 ) ) 
 REPRESENTATION_ITEM ( '' )  );
#45764 = B_SPLINE_CURVE_WITH_KNOTS ( 'NONE', 3,
 ( #29834, #14940, #30593, #14679 ),
 .UNSPECIFIED., .F., .F.,
 ( 4, 4 ),
 ( 0.9890644561682323532, 1.000000000000000000 ),
 .UNSPECIFIED. ) ;
#45765 = DIRECTION ( 'NONE',  ( 0.1191452206184307472, 0.000000000000000000, -0.9928768384869219865 ) ) ;
#45766 = ORIENTED_EDGE ( 'NONE', *, *, #32264, .F. ) ;
#45767 = LINE ( 'NONE', #14753, #13366 ) ;
#45768 = VECTOR ( 'NONE', #22081, 1000.000000000000000 ) ;
#45769 = DIRECTION ( 'NONE',  ( 0.000000000000000000, 1.000000000000000000, -2.406552799042969348E-16 ) ) ;
#45770 = CARTESIAN_POINT ( 'NONE',  ( -0.3370904143228963812, 0.2449105217885287067, 10.00000000000000000 ) ) ;
#45771 = CARTESIAN_POINT ( 'NONE',  ( -206.6959734468149463, -1.750000000000009992, -159.1817124430720298 ) ) ;
#45772 = DIRECTION ( 'NONE',  ( 0.000000000000000000, 0.000000000000000000, 1.000000000000000000 ) ) ;
#45773 = ORIENTED_EDGE ( 'NONE', *, *, #2062, .F. ) ;
#45774 = B_SPLINE_SURFACE_WITH_KNOTS ( 'NONE', 3, 3, ( 
 ( #15085, #6370, #7140, #29984 ),
 ( #6623, #41769, #22278, #34592 ),
 ( #10981, #22017, #18164, #33844 ),
 ( #2767, #38209, #22779, #38699 ) ),
 .UNSPECIFIED., .F., .F., .F.,
 ( 4, 4 ),
 ( 4, 4 ),
 ( 0.000000000000000000, 1.000000000000000000 ),
 ( 0.000000000000000000, 1.000000000000000000 ),
 .UNSPECIFIED. ) ;
#45775 = EDGE_LOOP ( 'NONE', ( #10205, #23101, #15105, #4437, #31308, #48707, #4702, #49068, #13995, #6755, #37676, #29744, #23073, #40771, #41342, #47756, #36819, #20664, #4454, #7528, #30903, #48281, #45739, #6506, #10410, #16288, #33879, #23105 ) ) ;
#45776 = CARTESIAN_POINT ( 'NONE',  ( -0.7547693905867810527, -1.149888081716692545, 9.972175347158279024 ) ) ;
#45777 = DIRECTION ( 'NONE',  ( 0.000000000000000000, 0.000000000000000000, -1.000000000000000000 ) ) ;
#45778 = ORIENTED_EDGE ( 'NONE', *, *, #15005, .T. ) ;
#45779 = CARTESIAN_POINT ( 'NONE',  ( -45.67084718096785423, 1.750000000000009326, 161.8434138227750907 ) ) ;
#45780 = CARTESIAN_POINT ( 'NONE',  ( -207.7210997126620384, 1.750000000000009548, -118.1565861772249519 ) ) ;
#45781 = DIRECTION ( 'NONE',  ( 0.000000000000000000, 1.000000000000000000, 0.000000000000000000 ) ) ;
#45782 = ORIENTED_EDGE ( 'NONE', *, *, #37641, .F. ) ;
#45783 = ORIENTED_EDGE ( 'NONE', *, *, #23161, .T. ) ;
#45784 = ADVANCED_FACE ( 'NONE', ( #35093 ), #31743, .T. ) ;
#45785 = ORIENTED_EDGE ( 'NONE', *, *, #40037, .T. ) ;
#45786 = DIRECTION ( 'NONE',  ( 0.000000000000000000, 0.000000000000000000, -1.000000000000000000 ) ) ;
#45787 = CARTESIAN_POINT ( 'NONE',  ( 191.5540265531851105, 0.000000000000000000, -37.43171244307205825 ) ) ;
#45788 = VECTOR ( 'NONE', #42380, 1000.000000000000000 ) ;
#45789 = CARTESIAN_POINT ( 'NONE',  ( 210.0000000000000568, 0.000000000000000000, 122.5682875569279844 ) ) ;
#45790 = ORIENTED_EDGE ( 'NONE', *, *, #5525, .T. ) ;
#45791 = DIRECTION ( 'NONE',  ( 0.000000000000000000, 0.000000000000000000, 1.000000000000000000 ) ) ;
#45792 = CARTESIAN_POINT ( 'NONE',  ( 74.32915281903215998, -1.750000000000009548, 81.84341382277507648 ) ) ;
#45793 = DIRECTION ( 'NONE',  ( 0.000000000000000000, 0.000000000000000000, -1.000000000000000000 ) ) ;
#45794 = ORIENTED_EDGE ( 'NONE', *, *, #42894, .T. ) ;
#45795 = ORIENTED_EDGE ( 'NONE', *, *, #28462, .F. ) ;
#45796 = DIRECTION ( 'NONE',  ( 0.000000000000000000, 1.000000000000000000, 6.123233995736766036E-17 ) ) ;
#45797 = PRESENTATION_LAYER_ASSIGNMENT (  '', '', ( #12248 ) ) ;
#45798 = VECTOR ( 'NONE', #13280, 1000.000000000000000 ) ;
#45799 = CYLINDRICAL_SURFACE ( 'NONE', #21816, 1.750000000000001554 ) ;
#45800 = CARTESIAN_POINT ( 'NONE',  ( -205.6708471809678827, 1.750000000000009548, -160.2068387089191219 ) ) ;
#45801 = ORIENTED_EDGE ( 'NONE', *, *, #9505, .F. ) ;
#45802 = CARTESIAN_POINT ( 'NONE',  ( 0.000000000000000000, -72.49999999999998579, 0.000000000000000000 ) ) ;
#45803 = LINE ( 'NONE', #26350, #30918 ) ;
#45804 = CARTESIAN_POINT ( 'NONE',  ( -4.641001526964560142, -33.28196331604080171, -8.016098858316199838 ) ) ;
#45805 = ORIENTED_EDGE ( 'NONE', *, *, #40011, .T. ) ;
#45806 = CARTESIAN_POINT ( 'NONE',  ( 24.47767542868285062, -23.18653802921781448, 8.807470649214879543 ) ) ;
#45807 = LINE ( 'NONE', #38420, #25064 ) ;
#45808 = DIRECTION ( 'NONE',  ( 0.000000000000000000, 1.000000000000000000, 0.000000000000000000 ) ) ;
#45809 = DIRECTION ( 'NONE',  ( 0.000000000000000000, 0.000000000000000000, -1.000000000000000000 ) ) ;
#45810 = LINE ( 'NONE', #19418, #11600 ) ;
#45811 = CARTESIAN_POINT ( 'NONE',  ( -14.99999999999876366, 17.00000000000000000, 5.000000000000004441 ) ) ;
#45812 = ORIENTED_EDGE ( 'NONE', *, *, #10516, .T. ) ;
#45813 = CARTESIAN_POINT ( 'NONE',  ( 1.011271242968677653, 0.7347315653656002477, -3.333333333333333481 ) ) ;
#45814 = CARTESIAN_POINT ( 'NONE',  ( -45.64490844644706868, -21.32281559348764333, 8.807470649214879543 ) ) ;
#45815 = FACE_BOUND ( 'NONE', #47263, .T. ) ;
#45816 = AXIS2_PLACEMENT_3D ( 'NONE', #13788, #44827, #49161 ) ;
#45817 = ORIENTED_EDGE ( 'NONE', *, *, #36613, .F. ) ;
#45818 = DIRECTION ( 'NONE',  ( -1.000000000000000000, 0.000000000000000000, -7.793956916774525800E-48 ) ) ;
#45819 = VECTOR ( 'NONE', #32186, 1000.000000000000000 ) ;
#45820 = CARTESIAN_POINT ( 'NONE',  ( -46.69597344681494633, 1.750000000000009992, 160.8182875569279702 ) ) ;
#45821 = VERTEX_POINT ( 'NONE', #23250 ) ;
#45822 = LINE ( 'NONE', #10215, #12348 ) ;
#45823 = LINE ( 'NONE', #41516, #24036 ) ;
#45824 = AXIS2_PLACEMENT_3D ( 'NONE', #5186, #20836, #1353 ) ;
#45825 = DIRECTION ( 'NONE',  ( 0.000000000000000000, 0.000000000000000000, -1.000000000000000000 ) ) ;
#45826 = ORIENTED_EDGE ( 'NONE', *, *, #41633, .T. ) ;
#45827 = CARTESIAN_POINT ( 'NONE',  ( 185.0000000000000568, 165.0000000000000000, 343.9999999999998863 ) ) ;
#45828 = ORIENTED_EDGE ( 'NONE', *, *, #7966, .T. ) ;
#45829 = VERTEX_POINT ( 'NONE', #50665 ) ;
#45830 = DIRECTION ( 'NONE',  ( -0.000000000000000000, -1.000000000000000000, -0.000000000000000000 ) ) ;
#45831 = VECTOR ( 'NONE', #5673, 1000.000000000000000 ) ;
#45832 = EDGE_CURVE ( 'NONE', #25388, #31636, #46899, .T. ) ;
#45833 = ORIENTED_EDGE ( 'NONE', *, *, #29028, .F. ) ;
#45834 = CARTESIAN_POINT ( 'NONE',  ( 214.9999999999999432, -172.9999999999999716, 232.0000000000000284 ) ) ;
#45835 = CARTESIAN_POINT ( 'NONE',  ( 210.0000000000000568, 0.000000000000000000, -159.1817124430720298 ) ) ;
#45836 = EDGE_CURVE ( 'NONE', #34748, #3643, #23526, .T. ) ;
#45837 = CARTESIAN_POINT ( 'NONE',  ( 50.24128791297869867, 41.04536285977714982, 5.000000000000000000 ) ) ;
#45838 = DIRECTION ( 'NONE',  ( 0.000000000000000000, 1.000000000000000000, -1.604368532695312981E-16 ) ) ;
#45839 = ORIENTED_EDGE ( 'NONE', *, *, #13997, .T. ) ;
#45840 = EDGE_CURVE ( 'NONE', #40426, #38146, #47832, .T. ) ;
#45841 = DIRECTION ( 'NONE',  ( -0.000000000000000000, -0.000000000000000000, -1.000000000000000000 ) ) ;
#45842 = CARTESIAN_POINT ( 'NONE',  ( -208.4459734468149463, 0.000000000000000000, -80.93171244307201562 ) ) ;
#45843 = ADVANCED_FACE ( 'NONE', ( #37110 ), #30677, .T. ) ;
#45844 = CARTESIAN_POINT ( 'NONE',  ( 166.9999999999999716, 6.000000000000060396, -340.0000000000001137 ) ) ;
#45845 = ORIENTED_EDGE ( 'NONE', *, *, #94, .T. ) ;
#45846 = CARTESIAN_POINT ( 'NONE',  ( -7.721099712662037540, -1.750000000000023537, 79.79316129108087807 ) ) ;
#45847 = DIRECTION ( 'NONE',  ( 0.000000000000000000, 0.000000000000000000, 1.000000000000000000 ) ) ;
#45848 = ORIENTED_EDGE ( 'NONE', *, *, #16934, .T. ) ;
#45849 = ORIENTED_EDGE ( 'NONE', *, *, #28625, .T. ) ;
#45850 = VERTEX_POINT ( 'NONE', #25043 ) ;
#45851 = CARTESIAN_POINT ( 'NONE',  ( 210.0000000000000568, 0.000000000000000000, 82.56828755692799859 ) ) ;
#45852 = EDGE_CURVE ( 'NONE', #38055, #28373, #41175, .T. ) ;
#45853 = CARTESIAN_POINT ( 'NONE',  ( 18.67411147745603373, 27.51799019669827473, -3.760136334089591248 ) ) ;
#45854 = ORIENTED_EDGE ( 'NONE', *, *, #7628, .F. ) ;
#45855 = AXIS2_PLACEMENT_3D ( 'NONE', #43287, #47353, #42770 ) ;
#45856 = AXIS2_PLACEMENT_3D ( 'NONE', #9589, #32961, #48540 ) ;
#45857 = DIRECTION ( 'NONE',  ( -0.000000000000000000, -0.000000000000000000, -1.000000000000000000 ) ) ;
#45858 = DIRECTION ( 'NONE',  ( 0.4374820812098816902, 0.3178493372392748872, -0.8411784753765541023 ) ) ;
#45859 = EDGE_CURVE ( 'NONE', #22212, #47361, #1112, .T. ) ;
#45860 = CARTESIAN_POINT ( 'NONE',  ( 1.962539651752403413, -0.2571568065648505708, 9.897807938190497978 ) ) ;
#45861 = VECTOR ( 'NONE', #33393, 1000.000000000000000 ) ;
#45862 = DIRECTION ( 'NONE',  ( -0.000000000000000000, -0.000000000000000000, -1.000000000000000000 ) ) ;
#45863 = DIRECTION ( 'NONE',  ( 0.000000000000000000, 0.000000000000000000, 1.000000000000000000 ) ) ;
#45864 = VERTEX_POINT ( 'NONE', #5277 ) ;
#45865 = CARTESIAN_POINT ( 'NONE',  ( 135.0000000000003411, 17.00000000000000000, -84.99999999999998579 ) ) ;
#45866 = CARTESIAN_POINT ( 'NONE',  ( 6.204997580903516941, -7.388441598285492518, 225.0000000000000000 ) ) ;
#45867 = AXIS2_PLACEMENT_3D ( 'NONE', #21720, #17867, #44803 ) ;
#45868 = AXIS2_PLACEMENT_3D ( 'NONE', #34119, #23303, #18940 ) ;
#45869 = LINE ( 'NONE', #30263, #42007 ) ;
#45870 = EDGE_CURVE ( 'NONE', #17731, #34855, #23619, .T. ) ;
#45871 = ADVANCED_FACE ( 'NONE', ( #17079 ), #36615, .T. ) ;
#45872 = ORIENTED_EDGE ( 'NONE', *, *, #4704, .T. ) ;
#45873 = DIRECTION ( 'NONE',  ( 0.000000000000000000, 0.000000000000000000, -1.000000000000000000 ) ) ;
#45874 = CARTESIAN_POINT ( 'NONE',  ( 177.5000000000000000, 74.83106485270648989, -130.5992382549688955 ) ) ;
#45875 = ADVANCED_FACE ( 'NONE', ( #1687 ), #13477, .T. ) ;
#45876 = ADVANCED_FACE ( 'NONE', ( #36868 ), #36351, .T. ) ;
#45877 = CARTESIAN_POINT ( 'NONE',  ( 111.5540265531850679, 0.000000000000000000, 165.0000000000000000 ) ) ;
#45878 = DIRECTION ( 'NONE',  ( -0.000000000000000000, -0.000000000000000000, 1.000000000000000000 ) ) ;
#45879 = ORIENTED_EDGE ( 'NONE', *, *, #42841, .T. ) ;
#45880 = EDGE_CURVE ( 'NONE', #48770, #4014, #9634, .T. ) ;
#45881 = DIRECTION ( 'NONE',  ( 1.000000000000000000, 6.344131455081961406E-16, -4.759647537211363479E-16 ) ) ;
#45882 = DIRECTION ( 'NONE',  ( 1.000000000000000000, 0.000000000000000000, 0.000000000000000000 ) ) ;
#45883 = EDGE_CURVE ( 'NONE', #40029, #38840, #7665, .T. ) ;
#45884 = CARTESIAN_POINT ( 'NONE',  ( 30.87089393895375267, -12.69923079256617449, -9.367992836599954742 ) ) ;
#45885 = CARTESIAN_POINT ( 'NONE',  ( 1.377636575563020438, -0.6021164824561170414, 9.953784399990622589 ) ) ;
#45886 = CARTESIAN_POINT ( 'NONE',  ( -44.94597344681493922, 1.025126265847089879, -77.43171244307200141 ) ) ;
#45887 = EDGE_LOOP ( 'NONE', ( #471, #21217, #26977, #18979 ) ) ;
#45888 = CARTESIAN_POINT ( 'NONE',  ( -4.945973446814916130, 1.025126265847097429, 119.0682875569279133 ) ) ;
#45889 = VERTEX_POINT ( 'NONE', #5527 ) ;
#45890 = CARTESIAN_POINT ( 'NONE',  ( 73.30402655318508209, -1.750000000000010214, -39.18171244307202983 ) ) ;
#45891 = ORIENTED_EDGE ( 'NONE', *, *, #10726, .T. ) ;
#45892 = CARTESIAN_POINT ( 'NONE',  ( 181.0000000000000000, -95.49999999999997158, -115.0000000000001563 ) ) ;
#45893 = CARTESIAN_POINT ( 'NONE',  ( 15.00000000000000000, 13.48684210526315930, 20.00000000000000000 ) ) ;
#45894 = ORIENTED_EDGE ( 'NONE', *, *, #48338, .T. ) ;
#45895 = DIRECTION ( 'NONE',  ( -0.000000000000000000, -0.000000000000000000, -1.000000000000000000 ) ) ;
#45896 = ADVANCED_FACE ( 'NONE', ( #32499 ), #21175, .T. ) ;
#45897 = VERTEX_POINT ( 'NONE', #17330 ) ;
#45898 = AXIS2_PLACEMENT_3D ( 'NONE', #46972, #27528, #15971 ) ;
#45899 = VECTOR ( 'NONE', #9342, 1000.000000000000000 ) ;
#45900 = ADVANCED_FACE ( 'NONE', ( #48333 ), #29138, .T. ) ;
#45901 = EDGE_CURVE ( 'NONE', #47066, #26504, #26044, .T. ) ;
#45902 = ORIENTED_EDGE ( 'NONE', *, *, #33734, .T. ) ;
#45903 = CARTESIAN_POINT ( 'NONE',  ( 224.9999999999999716, -175.0000000000000000, 499.9999999999998863 ) ) ;
#45904 = CARTESIAN_POINT ( 'NONE',  ( -8.445973446814964092, 1.025126265847096985, 42.56828755692800570 ) ) ;
#45905 = ORIENTED_EDGE ( 'NONE', *, *, #3388, .T. ) ;
#45906 = CARTESIAN_POINT ( 'NONE',  ( -44.94597344681493922, -1.025126265847088991, 2.568287556927986159 ) ) ;
#45907 = B_SPLINE_CURVE_WITH_KNOTS ( 'NONE', 3,
 ( #4587, #23578, #27937, #31797, #12523, #27682 ),
 .UNSPECIFIED., .F., .F.,
 ( 4, 2, 4 ),
 ( 4.171459933175973117E-17, 0.009882509389272368938, 0.01976501877854469277 ),
 .UNSPECIFIED. ) ;
#45908 = LINE ( 'NONE', #30551, #36566 ) ;
#45909 = CARTESIAN_POINT ( 'NONE',  ( 0.5107275442771160856, 1.175643901748075537, 9.976582533991678048 ) ) ;
#45910 = AXIS2_PLACEMENT_3D ( 'NONE', #50258, #15170, #22351 ) ;
#45911 = ORIENTED_EDGE ( 'NONE', *, *, #6658, .F. ) ;
#45912 = EDGE_LOOP ( 'NONE', ( #44351, #16728, #1459, #22336, #29774, #12163 ) ) ;
#45913 = CARTESIAN_POINT ( 'NONE',  ( -17.23491422248386584, 0.5912720620001978844, 8.727788335465566760 ) ) ;
#45914 = EDGE_CURVE ( 'NONE', #5639, #8857, #28865, .T. ) ;
#45915 = ORIENTED_EDGE ( 'NONE', *, *, #44960, .F. ) ;
#45916 = CARTESIAN_POINT ( 'NONE',  ( 34.99999999999997868, 17.00000000000000000, -90.00000000000000000 ) ) ;
#45917 = CARTESIAN_POINT ( 'NONE',  ( -8.445973446814964092, 1.025126265847097429, -80.93171244307204404 ) ) ;
#45918 = ORIENTED_EDGE ( 'NONE', *, *, #16831, .F. ) ;
#45919 = CARTESIAN_POINT ( 'NONE',  ( 0.2778388845795309314, -1.251314014313100520, 9.976582533991681601 ) ) ;
#45920 =( BOUNDED_CURVE ( )  B_SPLINE_CURVE ( 3, ( #47990, #8290, #23930, #39594 ),
 .UNSPECIFIED., .F., .F. ) 
 B_SPLINE_CURVE_WITH_KNOTS ( ( 4, 4 ),
 ( 3.141592653589793116, 4.712388980384689674 ),
 .UNSPECIFIED. ) 
 CURVE ( )  GEOMETRIC_REPRESENTATION_ITEM ( )  RATIONAL_B_SPLINE_CURVE ( ( 1.000000000000000000, 0.8047378541243649375, 0.8047378541243649375, 1.000000000000000000 ) ) 
 REPRESENTATION_ITEM ( '' )  );
#45921 = ORIENTED_EDGE ( 'NONE', *, *, #28778, .T. ) ;
#45922 = ADVANCED_FACE ( 'NONE', ( #26802 ), #37863, .T. ) ;
#45923 = CARTESIAN_POINT ( 'NONE',  ( 35.05402655318504657, 2.143131898507880377E-16, -157.4317124430720014 ) ) ;
#45924 = CARTESIAN_POINT ( 'NONE',  ( 24.47767542868285062, -23.18653802921781448, 8.807470649214879543 ) ) ;
#45925 = LINE ( 'NONE', #10806, #15621 ) ;
#45926 = PLANE ( 'NONE',  #48449 ) ;
#45927 = VERTEX_POINT ( 'NONE', #18079 ) ;
#45928 = ADVANCED_FACE ( 'NONE', ( #42435 ), #49587, .F. ) ;
#45929 = ORIENTED_EDGE ( 'NONE', *, *, #6201, .T. ) ;
#45930 = CARTESIAN_POINT ( 'NONE',  ( 114.3291528190321173, 1.749999999999996669, 1.843413822775057609 ) ) ;
#45931 = CARTESIAN_POINT ( 'NONE',  ( -21.24469349090191983, 33.89193117067290473, 910.0000000000000000 ) ) ;
#45932 = EDGE_LOOP ( 'NONE', ( #11179, #28903, #24446, #32461 ) ) ;
#45934 = ORIENTED_EDGE ( 'NONE', *, *, #50162, .T. ) ;
#45933 = VECTOR ( 'NONE', #22925, 1000.000000000000000 ) ;
#45935 = DIRECTION ( 'NONE',  ( 0.000000000000000000, 0.000000000000000000, 1.000000000000000000 ) ) ;
#45936 = CARTESIAN_POINT ( 'NONE',  ( -5.000000000000000000, 165.2000000000000171, -340.2000000000001592 ) ) ;
#45937 = CARTESIAN_POINT ( 'NONE',  ( -1.780432407520014415, -1.041450996408466612, 9.894754715216725671 ) ) ;
#45938 = CARTESIAN_POINT ( 'NONE',  ( -84.94597344681494633, 2.143131898507873721E-16, -165.0000000000000000 ) ) ;
#45939 = EDGE_CURVE ( 'NONE', #5061, #19653, #2925, .T. ) ;
#45940 = EDGE_CURVE ( 'NONE', #39919, #19835, #3174, .T. ) ;
#45941 = CARTESIAN_POINT ( 'NONE',  ( -124.9459734468149463, 2.143131898507847836E-16, -157.4317124430720582 ) ) ;
#45942 = CARTESIAN_POINT ( 'NONE',  ( 0.4612311909458165493, -1.380801828344328186, 9.938560165450807560 ) ) ;
#45943 =( REPRESENTATION_RELATIONSHIP ('NONE','NONE', #45699, #8438 ) REPRESENTATION_RELATIONSHIP_WITH_TRANSFORMATION ( #36471 )SHAPE_REPRESENTATION_RELATIONSHIP( ) );
#45944 = CARTESIAN_POINT ( 'NONE',  ( 5.888214538810389698, 16.20866436362417673, 8.727788335465566760 ) ) ;
#45945 = ORIENTED_EDGE ( 'NONE', *, *, #29695, .T. ) ;
#45946 = FACE_OUTER_BOUND ( 'NONE', #4721, .T. ) ;
#45947 = VECTOR ( 'NONE', #12468, 1000.000000000000000 ) ;
#45948 = EDGE_CURVE ( 'NONE', #37949, #27161, #34128, .T. ) ;
#45950 = AXIS2_PLACEMENT_3D ( 'NONE', #19611, #43219, #131 ) ;
#45949 = CARTESIAN_POINT ( 'NONE',  ( 0.8433491450857230065, -0.9182416014173362395, 9.981352469109934233 ) ) ;
#45951 = DIRECTION ( 'NONE',  ( -0.000000000000000000, -0.000000000000000000, 1.000000000000000000 ) ) ;
#45952 = ADVANCED_FACE ( 'NONE', ( #18577 ), #45750, .T. ) ;
#45953 = DIRECTION ( 'NONE',  ( -1.000000000000000000, 0.000000000000000000, 0.000000000000000000 ) ) ;
#45954 = ORIENTED_EDGE ( 'NONE', *, *, #21433, .T. ) ;
#45955 = CARTESIAN_POINT ( 'NONE',  ( -0.6108107228405769140, 1.056024183042602482, 9.963925895596188909 ) ) ;
#45956 = ORIENTED_EDGE ( 'NONE', *, *, #459, .F. ) ;
#45957 = DIRECTION ( 'NONE',  ( -1.000000000000000000, 0.000000000000000000, 0.000000000000000000 ) ) ;
#45958 = DIRECTION ( 'NONE',  ( 1.000000000000000000, 0.000000000000000000, -1.860490536778032451E-50 ) ) ;
#45959 = LINE ( 'NONE', #48796, #32932 ) ;
#45960 = ORIENTED_EDGE ( 'NONE', *, *, #41485, .F. ) ;
#45961 = EDGE_CURVE ( 'NONE', #37083, #44030, #19030, .T. ) ;
#45962 = CARTESIAN_POINT ( 'NONE',  ( -1.193089574352124149, -0.2545860991493743564, 9.963925895596188909 ) ) ;
#45963 = VERTEX_POINT ( 'NONE', #2192 ) ;
#45964 = CARTESIAN_POINT ( 'NONE',  ( -165.6708471809677974, -1.750000000000009326, 1.843413822775066269 ) ) ;
#45965 = CARTESIAN_POINT ( 'NONE',  ( 344.0000000000000000, 165.0000000000000000, -92.00000000000019895 ) ) ;
#45966 = CARTESIAN_POINT ( 'NONE',  ( -87.72109971266203843, -1.750000000000010214, 121.8434138227750623 ) ) ;
#45967 = VECTOR ( 'NONE', #606, 1000.000000000000000 ) ;
#45968 = VERTEX_POINT ( 'NONE', #41943 ) ;
#45969 = EDGE_LOOP ( 'NONE', ( #38063, #39886, #45790, #4562, #7714 ) ) ;
#45970 = CARTESIAN_POINT ( 'NONE',  ( -206.6959734468149463, -1.750000000000009992, 160.8182875569279702 ) ) ;
#45971 = CARTESIAN_POINT ( 'NONE',  ( 167.0000000000000000, -174.9999999999999716, -99.00000000000014211 ) ) ;
#45972 = ORIENTED_EDGE ( 'NONE', *, *, #10025, .T. ) ;
#45973 = VERTEX_POINT ( 'NONE', #45253 ) ;
#45974 = LINE ( 'NONE', #18795, #29042 ) ;
#45975 = DIRECTION ( 'NONE',  ( -0.4055129968046615185, -0.4055129968046615185, -0.8192181753629523833 ) ) ;
#45976 = CARTESIAN_POINT ( 'NONE',  ( 102.1135063278031652, 164.9999999999999716, 690.8162120245517599 ) ) ;
#45977 = ORIENTED_EDGE ( 'NONE', *, *, #49753, .F. ) ;
#45978 = DIRECTION ( 'NONE',  ( 0.000000000000000000, -2.537652627714642000E-15, -1.000000000000000000 ) ) ;
#45979 = ORIENTED_EDGE ( 'NONE', *, *, #41861, .F. ) ;
#45980 = CARTESIAN_POINT ( 'NONE',  ( 0.000000000000000000, 17.00000000000000000, 0.000000000000000000 ) ) ;
#45981 = VECTOR ( 'NONE', #32444, 1000.000000000000000 ) ;
#45982 = CARTESIAN_POINT ( 'NONE',  ( 35.05402655318504657, 2.143131898507880377E-16, 165.0000000000000000 ) ) ;
#45983 = CARTESIAN_POINT ( 'NONE',  ( -2.538055338523177440, -33.28424297489108596, -9.367992836599954742 ) ) ;
#45984 = ORIENTED_EDGE ( 'NONE', *, *, #49889, .T. ) ;
#45985 = ORIENTED_EDGE ( 'NONE', *, *, #934, .F. ) ;
#45986 = ORIENTED_EDGE ( 'NONE', *, *, #23372, .T. ) ;
#45987 = CARTESIAN_POINT ( 'NONE',  ( -42.51732812238059722, -47.49695244670218131, 5.000000000000000000 ) ) ;
#45988 = CARTESIAN_POINT ( 'NONE',  ( -46.69597344681494633, 1.750000000000009992, 160.8182875569279702 ) ) ;
#45989 = ORIENTED_EDGE ( 'NONE', *, *, #38192, .T. ) ;
#45990 = CARTESIAN_POINT ( 'NONE',  ( -581.3085477938157055, 47.50000000000000000, -68.52876838486925237 ) ) ;
#45991 = ORIENTED_EDGE ( 'NONE', *, *, #16747, .F. ) ;
#45992 = CARTESIAN_POINT ( 'NONE',  ( 210.0000000000000568, 0.000000000000000000, 120.8182875569279702 ) ) ;
#45993 =( NAMED_UNIT ( * ) SI_UNIT ( $, .STERADIAN. ) SOLID_ANGLE_UNIT ( ) );
#45994 = ORIENTED_EDGE ( 'NONE', *, *, #33928, .F. ) ;
#45995 = FACE_BOUND ( 'NONE', #12620, .T. ) ;
#45996 = CARTESIAN_POINT ( 'NONE',  ( 2.216591765713427975, -1.436486588195951430, 9.847478953136990398 ) ) ;
#45997 = CARTESIAN_POINT ( 'NONE',  ( 1.011271242968694084, -0.7347315653655782652, 10.00000000000000000 ) ) ;
#45998 = CARTESIAN_POINT ( 'NONE',  ( 185.0000000000000000, 6.000000000000060396, -350.0000000000001705 ) ) ;
#45999 = EDGE_CURVE ( 'NONE', #49298, #22581, #35515, .T. ) ;
#46000 = EDGE_CURVE ( 'NONE', #1528, #16006, #33753, .T. ) ;
#46001 =( BOUNDED_CURVE ( )  B_SPLINE_CURVE ( 3, ( #24328, #32274, #46855, #4052 ),
 .UNSPECIFIED., .F., .F. ) 
 B_SPLINE_CURVE_WITH_KNOTS ( ( 4, 4 ),
 ( 3.141592653589793116, 4.712388980384689674 ),
 .UNSPECIFIED. ) 
 CURVE ( )  GEOMETRIC_REPRESENTATION_ITEM ( )  RATIONAL_B_SPLINE_CURVE ( ( 1.000000000000000000, 0.8047378541243649375, 0.8047378541243649375, 1.000000000000000000 ) ) 
 REPRESENTATION_ITEM ( '' )  );
#46002 = CARTESIAN_POINT ( 'NONE',  ( 71.55402655318505367, 1.025126265847089213, -0.9317124430720324924 ) ) ;
#46003 = ORIENTED_EDGE ( 'NONE', *, *, #50041, .T. ) ;
#46004 = DIRECTION ( 'NONE',  ( 1.000000000000000000, 0.000000000000000000, -0.000000000000000000 ) ) ;
#46005 = AXIS2_PLACEMENT_3D ( 'NONE', #48938, #13824, #29497 ) ;
#46006 = DIRECTION ( 'NONE',  ( -0.000000000000000000, -0.000000000000000000, -1.000000000000000000 ) ) ;
#46007 = EDGE_CURVE ( 'NONE', #50249, #34526, #28238, .T. ) ;
#46008 = FACE_OUTER_BOUND ( 'NONE', #36025, .T. ) ;
#46009 = FACE_OUTER_BOUND ( 'NONE', #5515, .T. ) ;
#46010 = ADVANCED_FACE ( 'NONE', ( #38363 ), #49335, .T. ) ;
#46011 = EDGE_CURVE ( 'NONE', #16170, #20298, #27630, .T. ) ;
#46012 = DIRECTION ( 'NONE',  ( 0.000000000000000000, -2.265761274745217480E-16, 1.000000000000000000 ) ) ;
#46013 = CARTESIAN_POINT ( 'NONE',  ( -8.760073316077686911, -197.4999999999999432, -228.6347188485896140 ) ) ;
#46014 = EDGE_CURVE ( 'NONE', #44030, #43044, #4958, .T. ) ;
#46015 = CARTESIAN_POINT ( 'NONE',  ( 169.0000000000000000, -174.9999999999999716, -99.00000000000014211 ) ) ;
#46016 = ORIENTED_EDGE ( 'NONE', *, *, #12928, .T. ) ;
#46017 = DIRECTION ( 'NONE',  ( 7.793956916774525800E-48, 0.000000000000000000, 1.000000000000000000 ) ) ;
#46018 = CARTESIAN_POINT ( 'NONE',  ( 10.70590866674922204, -12.76446523155706814, -3.546734833711462365 ) ) ;
#46019 = CARTESIAN_POINT ( 'NONE',  ( -12.78770032058971395, -31.68259716188267916, 7.455576670931136185 ) ) ;
#46020 = CARTESIAN_POINT ( 'NONE',  ( 210.0000000000000568, 2.143131898507881856E-16, 79.06828755692797017 ) ) ;
#46021 = EDGE_LOOP ( 'NONE', ( #16970, #49436, #23036, #644 ) ) ;
#46022 = EDGE_LOOP ( 'NONE', ( #10832, #36173, #10213, #19225, #36905, #27208, #3582, #1363 ) ) ;
#46023 = CARTESIAN_POINT ( 'NONE',  ( -165.0000000000000284, 16.00000000000000000, 115.0000000000000142 ) ) ;
#46024 = CARTESIAN_POINT ( 'NONE',  ( -8.277096487746778308, 50.00000000000000711, 7.455576670931136185 ) ) ;
#46025 = VERTEX_POINT ( 'NONE', #30399 ) ;
#46026 = CARTESIAN_POINT ( 'NONE',  ( -0.09523839817533703844, -1.466467394240187350, 9.958264684458541183 ) ) ;
#46027 = CARTESIAN_POINT ( 'NONE',  ( 0.4692401618441018885, 1.180027720800731039, 9.975314328424618182 ) ) ;
#46028 = DIRECTION ( 'NONE',  ( -0.000000000000000000, -0.000000000000000000, -1.000000000000000000 ) ) ;
#46029 = AXIS2_PLACEMENT_3D ( 'NONE', #14277, #27109, #6845 ) ;
#46030 = ORIENTED_EDGE ( 'NONE', *, *, #10135, .F. ) ;
#46031 = VERTEX_POINT ( 'NONE', #1315 ) ;
#46032 = AXIS2_PLACEMENT_3D ( 'NONE', #44061, #29875, #16625 ) ;
#46033 = EDGE_LOOP ( 'NONE', ( #40257, #31387, #15734, #27910 ) ) ;
#46034 = EDGE_CURVE ( 'NONE', #17107, #41447, #9921, .T. ) ;
#46035 = CARTESIAN_POINT ( 'NONE',  ( 73.30402655318508209, -1.750000000000010658, 120.8182875569279702 ) ) ;
#46036 = CARTESIAN_POINT ( 'NONE',  ( 210.0000000000000568, 2.143131898507881856E-16, -120.9317124430720582 ) ) ;
#46037 = CARTESIAN_POINT ( 'NONE',  ( -1.540662627795934769, 1.371465786296043765, 9.894754715216725671 ) ) ;
#46038 = VERTEX_POINT ( 'NONE', #20793 ) ;
#46039 = DIRECTION ( 'NONE',  ( 1.860490536778032451E-50, 0.000000000000000000, -1.000000000000000000 ) ) ;
#46040 = LINE ( 'NONE', #31208, #4472 ) ;
#46041 = DIRECTION ( 'NONE',  ( 1.000000000000000000, 0.000000000000000000, 0.000000000000000000 ) ) ;
#46042 = VERTEX_POINT ( 'NONE', #16692 ) ;
#46043 = ORIENTED_EDGE ( 'NONE', *, *, #16863, .T. ) ;
#46044 = DIRECTION ( 'NONE',  ( 0.000000000000000000, 0.000000000000000000, 1.000000000000000000 ) ) ;
#46045 = CARTESIAN_POINT ( 'NONE',  ( -208.4459734468149463, 0.000000000000000000, 162.5682875569279702 ) ) ;
#46046 = LINE ( 'NONE', #37655, #1291 ) ;
#46047 = VERTEX_POINT ( 'NONE', #1056 ) ;
#46048 = EDGE_LOOP ( 'NONE', ( #29357, #29128, #27982, #18955, #1821, #19587 ) ) ;
#46049 = CARTESIAN_POINT ( 'NONE',  ( 47.22310614333766665, 16.46562252335956344, -3.760136334089591248 ) ) ;
#46050 = CARTESIAN_POINT ( 'NONE',  ( 185.0000000000000284, -168.9999999999999432, -115.0000000000001705 ) ) ;
#46051 =( BOUNDED_CURVE ( )  B_SPLINE_CURVE ( 3, ( #37952, #17672, #37205, #44842 ),
 .UNSPECIFIED., .F., .F. ) 
 B_SPLINE_CURVE_WITH_KNOTS ( ( 4, 4 ),
 ( 1.570796326794903663, 3.141592653589793116 ),
 .UNSPECIFIED. ) 
 CURVE ( )  GEOMETRIC_REPRESENTATION_ITEM ( )  RATIONAL_B_SPLINE_CURVE ( ( 1.000000000000000000, 0.8047378541243667138, 0.8047378541243667138, 1.000000000000000000 ) ) 
 REPRESENTATION_ITEM ( '' )  );
#46052 = CYLINDRICAL_SURFACE ( 'NONE', #10450, 3.500000000000003109 ) ;
#46053 = PLANE ( 'NONE',  #27780 ) ;
#46054 = ORIENTED_EDGE ( 'NONE', *, *, #46643, .T. ) ;
#46055 = SURFACE_SIDE_STYLE ('',( #37663 ) ) ;
#46056 = CARTESIAN_POINT ( 'NONE',  ( -164.9459734468149463, 2.143131898507880377E-16, -37.43171244307205825 ) ) ;
#46057 =( BOUNDED_CURVE ( )  B_SPLINE_CURVE ( 3, ( #10593, #34467, #45964, #49792 ),
 .UNSPECIFIED., .F., .F. ) 
 B_SPLINE_CURVE_WITH_KNOTS ( ( 4, 4 ),
 ( 3.141592653589793116, 4.712388980384689674 ),
 .UNSPECIFIED. ) 
 CURVE ( )  GEOMETRIC_REPRESENTATION_ITEM ( )  RATIONAL_B_SPLINE_CURVE ( ( 1.000000000000000000, 0.8047378541243649375, 0.8047378541243649375, 1.000000000000000000 ) ) 
 REPRESENTATION_ITEM ( '' )  );
#46058 = AXIS2_PLACEMENT_3D ( 'NONE', #3347, #49749, #30562 ) ;
#46059 = CARTESIAN_POINT ( 'NONE',  ( 85.00000000000152056, 17.00000000000000000, 60.00000000000000000 ) ) ;
#46060 = CARTESIAN_POINT ( 'NONE',  ( 1.133908876584335257, 0.5183204401656757998, 9.981352469109932457 ) ) ;
#46061 = CARTESIAN_POINT ( 'NONE',  ( 32.43949840348898306, 7.871562655726503266, -9.367992836599951190 ) ) ;
#46062 = DIRECTION ( 'NONE',  ( 0.000000000000000000, 0.000000000000000000, 1.000000000000000000 ) ) ;
#46063 = AXIS2_PLACEMENT_3D ( 'NONE', #47462, #28002, #31624 ) ;
#46064 = ORIENTED_EDGE ( 'NONE', *, *, #18888, .T. ) ;
#46065 = EDGE_CURVE ( 'NONE', #34142, #913, #42875, .T. ) ;
#46066 = CARTESIAN_POINT ( 'NONE',  ( 2.462075149652696027, -16.57295996686994499, 9.403735324607438884 ) ) ;
#46067 = AXIS2_PLACEMENT_3D ( 'NONE', #34834, #29691, #30455 ) ;
#46068 = CARTESIAN_POINT ( 'NONE',  ( 2.945500763482279627, 16.64098165802040086, -9.008049429158100807 ) ) ;
#46069 = CARTESIAN_POINT ( 'NONE',  ( 0.2773062244624638351, -1.251557370488896481, 9.948547179989619238 ) ) ;
#46070 =( GEOMETRIC_REPRESENTATION_CONTEXT ( 3 ) GLOBAL_UNCERTAINTY_ASSIGNED_CONTEXT ( ( #7605 ) ) GLOBAL_UNIT_ASSIGNED_CONTEXT ( ( #22635, #38812, #50031 ) ) REPRESENTATION_CONTEXT ( 'NONE', 'WORKASPACE' ) );
#46071 = VERTEX_POINT ( 'NONE', #24417 ) ;
#46072 = DIRECTION ( 'NONE',  ( -0.000000000000000000, -0.000000000000000000, -1.000000000000000000 ) ) ;
#46073 = VECTOR ( 'NONE', #24224, 1000.000000000000000 ) ;
#46074 = CARTESIAN_POINT ( 'NONE',  ( 340.0000000000000000, 183.3431457505076878, 358.3431457505073467 ) ) ;
#46075 = ORIENTED_EDGE ( 'NONE', *, *, #17961, .T. ) ;
#46076 = DIRECTION ( 'NONE',  ( -1.000000000000000000, -0.000000000000000000, -0.000000000000000000 ) ) ;
#46077 = CARTESIAN_POINT ( 'NONE',  ( -8.445973446814962315, 1.025126265847096985, 159.0682875569279418 ) ) ;
#46078 = CARTESIAN_POINT ( 'NONE',  ( 340.0000000000000568, 181.0000000000000284, 349.9999999999998295 ) ) ;
#46079 = CARTESIAN_POINT ( 'NONE',  ( 355.9999999999999432, -183.0000000000001421, -358.0000000000003411 ) ) ;
#46080 = VERTEX_POINT ( 'NONE', #48207 ) ;
#46081 = B_SPLINE_SURFACE_WITH_KNOTS ( 'NONE', 3, 3, ( 
 ( #47078, #18894, #46068, #23782 ),
 ( #19152, #4284, #50671, #19918 ),
 ( #11468, #7373, #35604, #38941 ),
 ( #16082, #10959, #26614, #42259 ) ),
 .UNSPECIFIED., .F., .F., .F.,
 ( 4, 4 ),
 ( 4, 4 ),
 ( 0.000000000000000000, 1.000000000000000000 ),
 ( 0.000000000000000000, 1.000000000000000000 ),
 .UNSPECIFIED. ) ;
#46082 = VERTEX_POINT ( 'NONE', #32613 ) ;
#46083 = ORIENTED_EDGE ( 'NONE', *, *, #19485, .T. ) ;
#46084 = CARTESIAN_POINT ( 'NONE',  ( -5.647304616913629616, -62.56198943095990472, 22.84256005001721945 ) ) ;
#46085 = ORIENTED_EDGE ( 'NONE', *, *, #20229, .F. ) ;
#46086 = AXIS2_PLACEMENT_3D ( 'NONE', #39433, #11971, #27627 ) ;
#46087 = CARTESIAN_POINT ( 'NONE',  ( 0.000000000000000000, 184.8000000000000114, 340.1999999999997044 ) ) ;
#46088 = DIRECTION ( 'NONE',  ( -1.000000000000000000, -0.000000000000000000, -0.000000000000000000 ) ) ;
#46089 = DIRECTION ( 'NONE',  ( 1.000000000000000000, 0.000000000000000000, 0.000000000000000000 ) ) ;
#46090 = CARTESIAN_POINT ( 'NONE',  ( 0.3656201545664388708, -2.182515578491310393, 9.881002359080277131 ) ) ;
#46091 = ORIENTED_EDGE ( 'NONE', *, *, #38576, .T. ) ;
#46093 = EDGE_CURVE ( 'NONE', #46904, #17107, #39383, .T. ) ;
#46092 = LINE ( 'NONE', #18672, #44452 ) ;
#46094 = CARTESIAN_POINT ( 'NONE',  ( 185.0000000000000000, -268.4999999999993747, -114.9999999999999147 ) ) ;
#46095 = CYLINDRICAL_SURFACE ( 'NONE', #20131, 2.000000000000001776 ) ;
#46096 = DIRECTION ( 'NONE',  ( -1.000000000000000000, -0.000000000000000000, -0.000000000000000000 ) ) ;
#46097 = ORIENTED_EDGE ( 'NONE', *, *, #36689, .F. ) ;
#46098 = CARTESIAN_POINT ( 'NONE',  ( 74.32915281903215998, 1.750000000000009548, -38.15658617722494483 ) ) ;
#46099 = CARTESIAN_POINT ( 'NONE',  ( 185.0000000000000284, 2.775557561562891351E-14, -111.0000000000001563 ) ) ;
#46100 = VECTOR ( 'NONE', #10710, 1000.000000000000000 ) ;
#46101 = ORIENTED_EDGE ( 'NONE', *, *, #50578, .F. ) ;
#46102 = ORIENTED_EDGE ( 'NONE', *, *, #40644, .F. ) ;
#46103 = VERTEX_POINT ( 'NONE', #4888 ) ;
#46104 = DIRECTION ( 'NONE',  ( -1.000000000000000000, -0.000000000000000000, -0.000000000000000000 ) ) ;
#46105 = VECTOR ( 'NONE', #4276, 1000.000000000000227 ) ;
#46106 = CARTESIAN_POINT ( 'NONE',  ( 210.0000000000000568, 0.000000000000000000, -119.1817124430720440 ) ) ;
#46107 = ORIENTED_EDGE ( 'NONE', *, *, #25852, .T. ) ;
#46108 = AXIS2_PLACEMENT_3D ( 'NONE', #10962, #46072, #18147 ) ;
#46109 =( NAMED_UNIT ( * ) SI_UNIT ( $, .STERADIAN. ) SOLID_ANGLE_UNIT ( ) );
#46110 = FACE_BOUND ( 'NONE', #18334, .T. ) ;
#46111 = CARTESIAN_POINT ( 'NONE',  ( -6.174150299305392053, 33.14591993373988998, 8.807470649214879543 ) ) ;
#46112 = CARTESIAN_POINT ( 'NONE',  ( 339.9999999999999432, -166.6568542494925396, -341.6568542494925396 ) ) ;
#46113 = CIRCLE ( 'NONE', #28143, 2.000000000000001776 ) ;
#46114 = CARTESIAN_POINT ( 'NONE',  ( 151.5540265531850537, 0.000000000000000000, 82.56828755692798438 ) ) ;
#46115 = CARTESIAN_POINT ( 'NONE',  ( 18.69789054174343690, -27.49790346457731616, -2.408242355805840784 ) ) ;
#46116 = DIRECTION ( 'NONE',  ( -1.000000000000000000, 0.000000000000000000, 0.000000000000000000 ) ) ;
#46117 = VERTEX_POINT ( 'NONE', #50349 ) ;
#46118 = CARTESIAN_POINT ( 'NONE',  ( -204.9459734468149463, 2.143131898507880377E-16, -117.4317124430720725 ) ) ;
#46119 = CARTESIAN_POINT ( 'NONE',  ( -6.695973446814940111, -1.750000000000023759, -39.18171244307202983 ) ) ;
#46120 = CARTESIAN_POINT ( 'NONE',  ( -127.7210997126620242, -1.749999999999996891, -120.2068387089191219 ) ) ;
#46121 = CARTESIAN_POINT ( 'NONE',  ( -46.69597344681494633, -1.750000000000010214, 40.81828755692798438 ) ) ;
#46122 = ORIENTED_EDGE ( 'NONE', *, *, #4179, .T. ) ;
#46123 = CARTESIAN_POINT ( 'NONE',  ( 344.0000000000000000, 167.0000000000001990, -342.0000000000002842 ) ) ;
#46124 = EDGE_CURVE ( 'NONE', #15741, #44725, #13096, .T. ) ;
#46125 = CARTESIAN_POINT ( 'NONE',  ( 181.0000000000000000, -270.4999999999999432, -339.9999999999998863 ) ) ;
#46126 = DIRECTION ( 'NONE',  ( 1.000000000000000000, 0.000000000000000000, 0.000000000000000000 ) ) ;
#46127 = CARTESIAN_POINT ( 'NONE',  ( -4.763548243873389154, 16.57409059453848599, 8.727788335465566760 ) ) ;
#46128 = CARTESIAN_POINT ( 'NONE',  ( 73.30402655318508209, 1.750000000000009992, 0.8182875569279768335 ) ) ;
#46129 = ORIENTED_EDGE ( 'NONE', *, *, #887, .T. ) ;
#46130 = CYLINDRICAL_SURFACE ( 'NONE', #20699, 1.750000000000015543 ) ;
#46131 = ORIENTED_EDGE ( 'NONE', *, *, #5525, .F. ) ;
#46132 = CARTESIAN_POINT ( 'NONE',  ( -119.9999999999997158, 17.00000000000000000, -60.00000000000000000 ) ) ;
#46133 = ORIENTED_EDGE ( 'NONE', *, *, #25848, .F. ) ;
#46134 = AXIS2_PLACEMENT_3D ( 'NONE', #38737, #50476, #10756 ) ;
#46136 = EDGE_CURVE ( 'NONE', #48233, #4709, #20762, .T. ) ;
#46135 = DIRECTION ( 'NONE',  ( -1.000000000000000000, -0.000000000000000000, -0.000000000000000000 ) ) ;
#46137 = EDGE_CURVE ( 'NONE', #18735, #33080, #41234, .T. ) ;
#46138 = VERTEX_POINT ( 'NONE', #28757 ) ;
#46139 = DIRECTION ( 'NONE',  ( -0.000000000000000000, -0.000000000000000000, -1.000000000000000000 ) ) ;
#46140 = ORIENTED_EDGE ( 'NONE', *, *, #6691, .T. ) ;
#46141 = AXIS2_PLACEMENT_3D ( 'NONE', #42888, #29648, #10150 ) ;
#46142 = B_SPLINE_CURVE_WITH_KNOTS ( 'NONE', 3,
 ( #30425, #46027, #42218, #22718 ),
 .UNSPECIFIED., .F., .F.,
 ( 4, 4 ),
 ( 0.000000000000000000, 0.0001252128669263239205 ),
 .UNSPECIFIED. ) ;
#46143 = EDGE_CURVE ( 'NONE', #35861, #20525, #15263, .T. ) ;
#46144 = ORIENTED_EDGE ( 'NONE', *, *, #8929, .T. ) ;
#46145 = CYLINDRICAL_SURFACE ( 'NONE', #20478, 1.750000000000015543 ) ;
#46146 = LINE ( 'NONE', #2575, #24869 ) ;
#46147 = ORIENTED_EDGE ( 'NONE', *, *, #49113, .F. ) ;
#46148 = CARTESIAN_POINT ( 'NONE',  ( -85.67084718096784002, 1.750000000000010214, 121.8434138227750623 ) ) ;
#46149 = CARTESIAN_POINT ( 'NONE',  ( 195.0540265531851105, 1.025126265847089435, -40.93171244307204404 ) ) ;
#46150 = CARTESIAN_POINT ( 'NONE',  ( 5.551115123125782702E-14, -168.9999999999999432, 341.9999999999997726 ) ) ;
#46151 = ORIENTED_EDGE ( 'NONE', *, *, #33212, .T. ) ;
#46153 = ORIENTED_EDGE ( 'NONE', *, *, #19040, .T. ) ;
#46152 = EDGE_CURVE ( 'NONE', #16567, #593, #38618, .T. ) ;
#46154 = CARTESIAN_POINT ( 'NONE',  ( 1.173396789973004228, 0.3425192899591110729, 9.969517326150317160 ) ) ;
#46155 = EDGE_CURVE ( 'NONE', #829, #20412, #44558, .T. ) ;
#46156 = CARTESIAN_POINT ( 'NONE',  ( 151.5540265531850537, 0.000000000000000000, 2.568287556927978166 ) ) ;
#46157 = EDGE_CURVE ( 'NONE', #40145, #18872, #27050, .T. ) ;
#46158 = EDGE_CURVE ( 'NONE', #47386, #36841, #49785, .T. ) ;
#46159 = VECTOR ( 'NONE', #14273, 1000.000000000000000 ) ;
#46160 = VERTEX_POINT ( 'NONE', #15499 ) ;
#46161 = CARTESIAN_POINT ( 'NONE',  ( 41.53730588968647197, 19.98817461849979793, 8.807470649214879543 ) ) ;
#46162 = DIRECTION ( 'NONE',  ( 0.000000000000000000, -1.000000000000000000, -3.186989995019654210E-49 ) ) ;
#46163 = VERTEX_POINT ( 'NONE', #47700 ) ;
#46164 = CARTESIAN_POINT ( 'NONE',  ( -0.2827943264366573617, 6.852167361307234472, 9.753789706659947711 ) ) ;
#46165 = ADVANCED_FACE ( 'NONE', ( #24163 ), #39817, .F. ) ;
#46166 = CARTESIAN_POINT ( 'NONE',  ( -4.945973446814903696, 2.143131898507912917E-16, 82.56828755692801280 ) ) ;
#46167 = ORIENTED_EDGE ( 'NONE', *, *, #35294, .F. ) ;
#46168 = CARTESIAN_POINT ( 'NONE',  ( -164.9999999999987779, 16.00000000000000000, 5.000000000000004441 ) ) ;
#46169 = DIRECTION ( 'NONE',  ( 0.000000000000000000, 0.3790464617558786942, -0.9253776417389547593 ) ) ;
#46170 = CARTESIAN_POINT ( 'NONE',  ( 0.9390173899407876501, 1.130417317737878458, 9.958264684458711713 ) ) ;
#46171 = AXIS2_PLACEMENT_3D ( 'NONE', #12071, #31584, #16413 ) ;
#46172 = EDGE_LOOP ( 'NONE', ( #18471, #21785, #1288, #35239 ) ) ;
#46173 = VECTOR ( 'NONE', #19440, 1000.000000000000000 ) ;
#46174 = DIRECTION ( 'NONE',  ( -1.000000000000000000, 0.000000000000000000, 0.000000000000000000 ) ) ;
#46175 = CARTESIAN_POINT ( 'NONE',  ( -1.011271242968683426, -0.7347315653655928092, 10.00000000000000000 ) ) ;
#46176 = AXIS2_PLACEMENT_3D ( 'NONE', #47718, #23659, #27764 ) ;
#46177 = CARTESIAN_POINT ( 'NONE',  ( 0.000000000000000000, 169.0000000000000000, -344.0000000000001705 ) ) ;
#46178 = ORIENTED_EDGE ( 'NONE', *, *, #39172, .F. ) ;
#46179 = EDGE_CURVE ( 'NONE', #10514, #30357, #20550, .T. ) ;
#46180 = AXIS2_PLACEMENT_3D ( 'NONE', #41196, #1709, #44778 ) ;
#46181 = VERTEX_POINT ( 'NONE', #49467 ) ;
#46182 = DIRECTION ( 'NONE',  ( 0.9818567070645118910, -6.036837696399288689E-15, -0.1896243834332324019 ) ) ;
#46183 = CARTESIAN_POINT ( 'NONE',  ( 31.55402655318503236, -1.025126265847089435, 39.06828755692797728 ) ) ;
#46184 = DIRECTION ( 'NONE',  ( -1.000000000000000000, 0.000000000000000000, 0.000000000000000000 ) ) ;
#46185 = CARTESIAN_POINT ( 'NONE',  ( 325.0507910275983932, 325.0507910275983932, 321.8002831173224649 ) ) ;
#46186 = EDGE_CURVE ( 'NONE', #35077, #31351, #40414, .T. ) ;
#46187 = EDGE_CURVE ( 'NONE', #17726, #32522, #9498, .T. ) ;
#46188 =( NAMED_UNIT ( * ) SI_UNIT ( $, .STERADIAN. ) SOLID_ANGLE_UNIT ( ) );
#46189 = CARTESIAN_POINT ( 'NONE',  ( 210.0000000000000568, 0.000000000000000000, -37.43171244307202272 ) ) ;
#46190 = DIRECTION ( 'NONE',  ( 0.000000000000000000, -1.000000000000000000, 0.000000000000000000 ) ) ;
#46191 = ORIENTED_EDGE ( 'NONE', *, *, #34223, .T. ) ;
#46192 = DIRECTION ( 'NONE',  ( -0.000000000000000000, 1.000000000000000000, -2.406552799042969348E-16 ) ) ;
#46193 = EDGE_CURVE ( 'NONE', #26846, #36961, #19581, .T. ) ;
#46194 = B_SPLINE_SURFACE_WITH_KNOTS ( 'NONE', 3, 3, ( 
 ( #46237, #30898, #42410, #10865 ),
 ( #34489, #7028, #26526, #14975 ),
 ( #35014, #38852, #18557, #46484 ),
 ( #50580, #45983, #50066, #42922 ) ),
 .UNSPECIFIED., .F., .F., .F.,
 ( 4, 4 ),
 ( 4, 4 ),
 ( 0.000000000000000000, 1.000000000000000000 ),
 ( 0.000000000000000000, 1.000000000000000000 ),
 .UNSPECIFIED. ) ;
#46195 = CARTESIAN_POINT ( 'NONE',  ( 1.270843316669197254, -0.6654759734677784255, 9.950105812514292936 ) ) ;
#46196 = CARTESIAN_POINT ( 'NONE',  ( 376.8544389702901753, 0.000000000000000000, 219.8317560660024697 ) ) ;
#46197 = EDGE_CURVE ( 'NONE', #45172, #28471, #32876, .T. ) ;
#46198 =( BOUNDED_CURVE ( )  B_SPLINE_CURVE ( 3, ( #36307, #36052, #1145, #35543 ),
 .UNSPECIFIED., .F., .F. ) 
 B_SPLINE_CURVE_WITH_KNOTS ( ( 4, 4 ),
 ( 1.570796326794896558, 3.141592653589793116 ),
 .UNSPECIFIED. ) 
 CURVE ( )  GEOMETRIC_REPRESENTATION_ITEM ( )  RATIONAL_B_SPLINE_CURVE ( ( 1.000000000000000000, 0.8047378541243649375, 0.8047378541243649375, 1.000000000000000000 ) ) 
 REPRESENTATION_ITEM ( '' )  );
#46199 = VECTOR ( 'NONE', #19661, 1000.000000000000000 ) ;
#46200 = EDGE_LOOP ( 'NONE', ( #26249, #15283, #25965, #22424 ) ) ;
#46201 = DIRECTION ( 'NONE',  ( 1.000000000000000000, 0.000000000000000000, 0.000000000000000000 ) ) ;
#46202 = EDGE_LOOP ( 'NONE', ( #7480, #48752, #5355, #40538, #35731 ) ) ;
#46203 = DIRECTION ( 'NONE',  ( -0.000000000000000000, -0.000000000000000000, -1.000000000000000000 ) ) ;
#46204 = CARTESIAN_POINT ( 'NONE',  ( -164.9459734468149463, 2.143131898507880377E-16, -40.93171244307202983 ) ) ;
#46205 = CARTESIAN_POINT ( 'NONE',  ( -44.94597344681493922, 2.143131898507880377E-16, 159.0682875569279702 ) ) ;
#46206 = ORIENTED_EDGE ( 'NONE', *, *, #49039, .F. ) ;
#46207 = CYLINDRICAL_SURFACE ( 'NONE', #37625, 1.750000000000001554 ) ;
#46208 = CARTESIAN_POINT ( 'NONE',  ( -124.9459734468149321, 1.025126265847081219, 162.5682875569279133 ) ) ;
#46209 = ORIENTED_EDGE ( 'NONE', *, *, #8080, .T. ) ;
#46210 = CARTESIAN_POINT ( 'NONE',  ( -7.372990760266265653, 0.000000000000000000, -5.000000000000000000 ) ) ;
#46211 = VECTOR ( 'NONE', #9105, 1000.000000000000000 ) ;
#46212 = ADVANCED_FACE ( 'NONE', ( #29257 ), #45359, .T. ) ;
#46213 = DIRECTION ( 'NONE',  ( -1.000000000000000000, -0.000000000000000000, -0.000000000000000000 ) ) ;
#46214 = DIRECTION ( 'NONE',  ( -1.586032880504786307E-16, 1.654361225106055350E-24, -1.000000000000000000 ) ) ;
#46215 = VECTOR ( 'NONE', #5032, 1000.000000000000000 ) ;
#46216 =( BOUNDED_CURVE ( )  B_SPLINE_CURVE ( 3, ( #45617, #26395, #26141, #14849 ),
 .UNSPECIFIED., .F., .F. ) 
 B_SPLINE_CURVE_WITH_KNOTS ( ( 4, 4 ),
 ( 4.712388980384662140, 6.283185307179586232 ),
 .UNSPECIFIED. ) 
 CURVE ( )  GEOMETRIC_REPRESENTATION_ITEM ( )  RATIONAL_B_SPLINE_CURVE ( ( 1.000000000000000000, 0.8047378541243583872, 0.8047378541243583872, 1.000000000000000000 ) ) 
 REPRESENTATION_ITEM ( '' )  );
#46217 = EDGE_LOOP ( 'NONE', ( #32317, #38640, #38207, #43118 ) ) ;
#46218 = ORIENTED_EDGE ( 'NONE', *, *, #28383, .F. ) ;
#46219 = CARTESIAN_POINT ( 'NONE',  ( -164.9999999999994031, 16.00000000000000000, -54.99999999999999289 ) ) ;
#46220 = ADVANCED_FACE ( 'NONE', ( #48458 ), #49022, .T. ) ;
#46221 = AXIS2_PLACEMENT_3D ( 'NONE', #33663, #6450, #49757 ) ;
#46222 = DIRECTION ( 'NONE',  ( 0.000000000000000000, -1.000000000000000000, 0.000000000000000000 ) ) ;
#46223 = EDGE_CURVE ( 'NONE', #46923, #11032, #40557, .T. ) ;
#46224 = EDGE_CURVE ( 'NONE', #22583, #12326, #42836, .T. ) ;
#46225 = ORIENTED_EDGE ( 'NONE', *, *, #27807, .F. ) ;
#46226 = ORIENTED_EDGE ( 'NONE', *, *, #50404, .F. ) ;
#46227 = CARTESIAN_POINT ( 'NONE',  ( -127.7210997126620242, -1.749999999999996891, -118.1565861772249661 ) ) ;
#46228 = CARTESIAN_POINT ( 'NONE',  ( 191.5540265531850537, -1.025126265847089435, 39.06828755692797728 ) ) ;
#46229 = CARTESIAN_POINT ( 'NONE',  ( 339.9999999999999432, 167.0000000000000000, -344.0000000000001705 ) ) ;
#46230 = ORIENTED_EDGE ( 'NONE', *, *, #29770, .F. ) ;
#46231 = DIRECTION ( 'NONE',  ( -1.000000000000000000, 0.000000000000000000, 0.000000000000000000 ) ) ;
#46232 = EDGE_CURVE ( 'NONE', #46936, #27142, #14098, .T. ) ;
#46233 = ORIENTED_EDGE ( 'NONE', *, *, #23647, .T. ) ;
#46234 = EDGE_CURVE ( 'NONE', #17047, #1405, #6161, .T. ) ;
#46235 = CYLINDRICAL_SURFACE ( 'NONE', #23043, 1.750000000000015543 ) ;
#46236 = DIRECTION ( 'NONE',  ( 0.000000000000000000, -0.2223603367690619725, 0.9749645535258958384 ) ) ;
#46237 = CARTESIAN_POINT ( 'NONE',  ( 8.277096487746778308, -50.00000000000000711, 7.455576670931136185 ) ) ;
#46238 = VECTOR ( 'NONE', #44005, 1000.000000000000000 ) ;
#46239 = ORIENTED_EDGE ( 'NONE', *, *, #31152, .T. ) ;
#46240 = ORIENTED_EDGE ( 'NONE', *, *, #26331, .F. ) ;
#46241 = ORIENTED_EDGE ( 'NONE', *, *, #737, .F. ) ;
#46242 = VECTOR ( 'NONE', #29080, 1000.000000000000000 ) ;
#46243 = CARTESIAN_POINT ( 'NONE',  ( 0.000000000000000000, 169.0000000000000000, -360.0000000000002274 ) ) ;
#46244 = CARTESIAN_POINT ( 'NONE',  ( -44.99506233596265048, -23.32283626942287569, 7.455576670931136185 ) ) ;
#46245 = ORIENTED_EDGE ( 'NONE', *, *, #12659, .T. ) ;
#46246 = ORIENTED_EDGE ( 'NONE', *, *, #37452, .F. ) ;
#46247 = DIRECTION ( 'NONE',  ( -1.000000000000000000, 0.000000000000000000, 0.000000000000000000 ) ) ;
#46248 = EDGE_LOOP ( 'NONE', ( #37938, #16074, #34354, #50712 ) ) ;
#46249 = CARTESIAN_POINT ( 'NONE',  ( -11.73320209285699889, 11.96063479729179768, 9.403735324607438884 ) ) ;
#46250 = CARTESIAN_POINT ( 'NONE',  ( -168.4459734468149463, 0.000000000000000000, -40.93171244307202983 ) ) ;
#46251 = CARTESIAN_POINT ( 'NONE',  ( -50.11058929355266400, 7.578863168071933387, 7.455576670931136185 ) ) ;
#46252 = PLANE ( 'NONE',  #10548 ) ;
#46253 = ADVANCED_FACE ( 'NONE', ( #26164 ), #14608, .T. ) ;
#46254 = AXIS2_PLACEMENT_3D ( 'NONE', #6065, #40473, #17363 ) ;
#46255 = CARTESIAN_POINT ( 'NONE',  ( -206.6959734468149463, 1.750000000000010658, -79.18171244307201562 ) ) ;
#46256 = VERTEX_POINT ( 'NONE', #46391 ) ;
#46257 = CARTESIAN_POINT ( 'NONE',  ( -194.9999999999999432, -172.9999999999999716, 232.0000000000000284 ) ) ;
#46258 = CARTESIAN_POINT ( 'NONE',  ( -2.097937730060984052, 0.2450639578955122744, 9.884520316594375799 ) ) ;
#46259 = CARTESIAN_POINT ( 'NONE',  ( -49.46074318306826001, 9.578883844007169301, 8.807470649214879543 ) ) ;
#46260 = VECTOR ( 'NONE', #36142, 1000.000000000000000 ) ;
#46261 = CARTESIAN_POINT ( 'NONE',  ( -225.0000000000000568, 164.9999999999999716, 352.0000000000000000 ) ) ;
#46262 = CARTESIAN_POINT ( 'NONE',  ( -44.99506233596265048, -23.32283626942287569, 7.455576670931136185 ) ) ;
#46263 = EDGE_CURVE ( 'NONE', #29971, #17736, #38244, .T. ) ;
#46264 = CARTESIAN_POINT ( 'NONE',  ( 130.0000000000008811, 17.00000000000000000, 0.000000000000000000 ) ) ;
#46265 = CARTESIAN_POINT ( 'NONE',  ( 169.0000000000000000, -174.9999999999999716, -113.0000000000001563 ) ) ;
#46266 = EDGE_LOOP ( 'NONE', ( #39363, #21580, #49486, #46607, #41821 ) ) ;
#46267 = VECTOR ( 'NONE', #29217, 1000.000000000000000 ) ;
#46268 = DIRECTION ( 'NONE',  ( 0.000000000000000000, -2.406552799042969348E-16, -1.000000000000000000 ) ) ;
#46269 = EDGE_CURVE ( 'NONE', #9554, #33142, #18455, .T. ) ;
#46270 = VECTOR ( 'NONE', #24539, 1000.000000000000000 ) ;
#46271 = CARTESIAN_POINT ( 'NONE',  ( 35.00000000000028422, 16.00000000000000000, -84.99999999999998579 ) ) ;
#46272 = LINE ( 'NONE', #26563, #25046 ) ;
#46273 = AXIS2_PLACEMENT_3D ( 'NONE', #370, #47267, #35029 ) ;
#46274 = ORIENTED_EDGE ( 'NONE', *, *, #9661, .F. ) ;
#46275 = EDGE_LOOP ( 'NONE', ( #48505, #32068, #10338, #33343, #27697, #46225 ) ) ;
#46276 = FACE_OUTER_BOUND ( 'NONE', #34234, .T. ) ;
#46277 = CARTESIAN_POINT ( 'NONE',  ( 6.174150299305392053, -33.14591993373988998, 8.807470649214879543 ) ) ;
#46278 = AXIS2_PLACEMENT_3D ( 'NONE', #29569, #37797, #21361 ) ;
#46279 = EDGE_CURVE ( 'NONE', #36017, #27788, #15173, .T. ) ;
#46280 = EDGE_CURVE ( 'NONE', #25760, #31020, #7685, .T. ) ;
#46281 = ORIENTED_EDGE ( 'NONE', *, *, #33426, .F. ) ;
#46282 = EDGE_LOOP ( 'NONE', ( #42904, #18721, #18477, #13817 ) ) ;
#46283 = CARTESIAN_POINT ( 'NONE',  ( -119.9999999999981668, 17.00000000000000000, 90.00000000000000000 ) ) ;
#46284 = CARTESIAN_POINT ( 'NONE',  ( 355.9999999999999432, -174.9999999999999432, 359.9999999999998295 ) ) ;
#46285 = DIRECTION ( 'NONE',  ( -1.000000000000000000, -0.000000000000000000, -0.000000000000000000 ) ) ;
#46286 = CIRCLE ( 'NONE', #2092, 2.000000000000001776 ) ;
#46287 = ORIENTED_EDGE ( 'NONE', *, *, #33705, .F. ) ;
#46288 = ORIENTED_EDGE ( 'NONE', *, *, #28678, .F. ) ;
#46289 = VERTEX_POINT ( 'NONE', #22308 ) ;
#46290 = EDGE_CURVE ( 'NONE', #31511, #29900, #11279, .T. ) ;
#46291 =( GEOMETRIC_REPRESENTATION_CONTEXT ( 3 ) GLOBAL_UNCERTAINTY_ASSIGNED_CONTEXT ( ( #38831 ) ) GLOBAL_UNIT_ASSIGNED_CONTEXT ( ( #2367, #25724, #6715 ) ) REPRESENTATION_CONTEXT ( 'NONE', 'WORKASPACE' ) );
#46292 = AXIS2_PLACEMENT_3D ( 'NONE', #11146, #11388, #47007 ) ;
#46294 = EDGE_CURVE ( 'NONE', #50289, #3893, #3679, .T. ) ;
#46293 = LINE ( 'NONE', #18112, #4504 ) ;
#46295 = LINE ( 'NONE', #10922, #12766 ) ;
#46296 = EDGE_CURVE ( 'NONE', #10383, #48103, #20409, .T. ) ;
#46297 = CARTESIAN_POINT ( 'NONE',  ( 135.0000000000015632, 16.00000000000000000, 60.00000000000000000 ) ) ;
#46298 = ORIENTED_EDGE ( 'NONE', *, *, #30901, .T. ) ;
#46299 = DIRECTION ( 'NONE',  ( 1.000000000000000000, 0.000000000000000000, 0.000000000000000000 ) ) ;
#46300 = DIRECTION ( 'NONE',  ( -0.000000000000000000, -1.000000000000000000, -0.000000000000000000 ) ) ;
#46301 = CARTESIAN_POINT ( 'NONE',  ( -46.69597344681494633, -1.750000000000010658, -119.1817124430720440 ) ) ;
#46302 = EDGE_LOOP ( 'NONE', ( #4109, #12464, #12304, #24865 ) ) ;
#46303 =( BOUNDED_CURVE ( )  B_SPLINE_CURVE ( 3, ( #20897, #28096, #24257, #21393 ),
 .UNSPECIFIED., .F., .F. ) 
 B_SPLINE_CURVE_WITH_KNOTS ( ( 4, 4 ),
 ( 4.712388980384689674, 6.283185307179586232 ),
 .UNSPECIFIED. ) 
 CURVE ( )  GEOMETRIC_REPRESENTATION_ITEM ( )  RATIONAL_B_SPLINE_CURVE ( ( 1.000000000000000000, 0.8047378541243649375, 0.8047378541243649375, 1.000000000000000000 ) ) 
 REPRESENTATION_ITEM ( '' )  );
#46304 = VERTEX_POINT ( 'NONE', #42059 ) ;
#46305 = CARTESIAN_POINT ( 'NONE',  ( 185.0000000000000568, 175.0000000000000284, 343.9999999999998863 ) ) ;
#46306 = CARTESIAN_POINT ( 'NONE',  ( -46.69597344681494633, 1.750000000000009992, 160.8182875569279702 ) ) ;
#46307 = ADVANCED_FACE ( 'NONE', ( #6918 ), #23062, .T. ) ;
#46308 = FACE_OUTER_BOUND ( 'NONE', #33130, .T. ) ;
#46309 = B_SPLINE_CURVE_WITH_KNOTS ( 'NONE', 3,
 ( #11023, #29515, #18202, #49218 ),
 .UNSPECIFIED., .F., .F.,
 ( 4, 4 ),
 ( 0.01005345353272254355, 0.01006177981554775419 ),
 .UNSPECIFIED. ) ;
#46310 = ORIENTED_EDGE ( 'NONE', *, *, #44882, .F. ) ;
#46311 = ORIENTED_EDGE ( 'NONE', *, *, #34964, .T. ) ;
#46312 = PLANE ( 'NONE',  #1228 ) ;
#46313 = CARTESIAN_POINT ( 'NONE',  ( 5.551115123125782702E-14, -166.9999999999999432, 355.9999999999997726 ) ) ;
#46314 = VECTOR ( 'NONE', #590, 1000.000000000000000 ) ;
#46315 = DIRECTION ( 'NONE',  ( 3.172065784643303486E-16, 1.000000000000000000, 8.758115402030106693E-47 ) ) ;
#46316 = CARTESIAN_POINT ( 'NONE',  ( -208.4459734468148611, 1.025126265847089657, 79.06828755692797017 ) ) ;
#46317 = CARTESIAN_POINT ( 'NONE',  ( 6.174150299305392053, -33.14591993373988998, 8.807470649214879543 ) ) ;
#46318 = VECTOR ( 'NONE', #18556, 1000.000000000000000 ) ;
#46319 = ORIENTED_EDGE ( 'NONE', *, *, #42198, .F. ) ;
#46320 = LINE ( 'NONE', #18880, #25129 ) ;
#46321 = DIRECTION ( 'NONE',  ( -0.000000000000000000, -1.000000000000000000, -0.000000000000000000 ) ) ;
#46323 = AXIS2_PLACEMENT_3D ( 'NONE', #13225, #9637, #48082 ) ;
#46322 = CARTESIAN_POINT ( 'NONE',  ( 35.05402655318504657, 2.143131898507880377E-16, -120.9317124430720725 ) ) ;
#46324 = CARTESIAN_POINT ( 'NONE',  ( 339.9999999999999432, 181.0000000000000284, -344.0000000000001705 ) ) ;
#46325 = DIRECTION ( 'NONE',  ( -0.000000000000000000, -0.000000000000000000, -1.000000000000000000 ) ) ;
#46326 = AXIS2_PLACEMENT_3D ( 'NONE', #26131, #10483, #18173 ) ;
#46328 =( GEOMETRIC_REPRESENTATION_CONTEXT ( 3 ) GLOBAL_UNCERTAINTY_ASSIGNED_CONTEXT ( ( #12786 ) ) GLOBAL_UNIT_ASSIGNED_CONTEXT ( ( #47510, #35514, #12639 ) ) REPRESENTATION_CONTEXT ( 'NONE', 'WORKASPACE' ) );
#46327 = PLANE ( 'NONE',  #351 ) ;
#46329 = ORIENTED_EDGE ( 'NONE', *, *, #18952, .F. ) ;
#46330 = CARTESIAN_POINT ( 'NONE',  ( 185.0000000000000000, -164.9999999999999432, -356.0000000000001705 ) ) ;
#46331 = CARTESIAN_POINT ( 'NONE',  ( 31.55402655318503236, 0.000000000000000000, 79.06828755692797017 ) ) ;
#46332 = CARTESIAN_POINT ( 'NONE',  ( 1.011271242968688311, -0.7347315653655855927, 10.00000000000000000 ) ) ;
#46333 = CIRCLE ( 'NONE', #7039, 1.750000000000015543 ) ;
#46334 = CARTESIAN_POINT ( 'NONE',  ( -1.011271242968683426, -0.7347315653655928092, 10.00000000000000000 ) ) ;
#46335 = EDGE_CURVE ( 'NONE', #14478, #20370, #3056, .T. ) ;
#46336 = AXIS2_PLACEMENT_3D ( 'NONE', #38638, #42211, #22710 ) ;
#46337 = VERTEX_POINT ( 'NONE', #34378 ) ;
#46338 = FACE_OUTER_BOUND ( 'NONE', #20977, .T. ) ;
#46339 = LINE ( 'NONE', #27133, #31111 ) ;
#46340 = ORIENTED_EDGE ( 'NONE', *, *, #34364, .T. ) ;
#46341 = DIRECTION ( 'NONE',  ( 0.000000000000000000, 0.000000000000000000, -1.000000000000000000 ) ) ;
#46342 = CARTESIAN_POINT ( 'NONE',  ( 4.641001526964561918, 33.28196331604080171, -8.016098858316205167 ) ) ;
#46343 = CARTESIAN_POINT ( 'NONE',  ( -0.1265591857321690383, -1.213367045380180809, 9.963925895596192461 ) ) ;
#46344 = CARTESIAN_POINT ( 'NONE',  ( 25.08868538179583396, -27.91927157928032699, 6.057468652304065060 ) ) ;
#46345 = ORIENTED_EDGE ( 'NONE', *, *, #7650, .T. ) ;
#46346 = CARTESIAN_POINT ( 'NONE',  ( -30.22736451279196856, -39.84193304692609416, -2.408242355805840784 ) ) ;
#46347 = ORIENTED_EDGE ( 'NONE', *, *, #17207, .T. ) ;
#46348 = ORIENTED_EDGE ( 'NONE', *, *, #28784, .F. ) ;
#46349 = CARTESIAN_POINT ( 'NONE',  ( -214.9999999999999432, -173.0000000000000000, 352.0000000000000568 ) ) ;
#46350 = AXIS2_PLACEMENT_3D ( 'NONE', #38902, #27337, #3728 ) ;
#46351 = EDGE_CURVE ( 'NONE', #42713, #14002, #6333, .T. ) ;
#46352 = EDGE_CURVE ( 'NONE', #15209, #12301, #26674, .T. ) ;
#46353 = VECTOR ( 'NONE', #23166, 1000.000000000000000 ) ;
#46354 = ORIENTED_EDGE ( 'NONE', *, *, #18008, .T. ) ;
#46355 = CARTESIAN_POINT ( 'NONE',  ( 50.00000000000000000, -50.00000000000000000, 800.0000000000000000 ) ) ;
#46356 = DIRECTION ( 'NONE',  ( -1.000000000000000000, -0.000000000000000000, -0.000000000000000000 ) ) ;
#46357 = CARTESIAN_POINT ( 'NONE',  ( 7.241383964640743187, 3.469446951953614189E-15, 5.000000000000000000 ) ) ;
#46358 = PLANE ( 'NONE',  #6308 ) ;
#46359 = VERTEX_POINT ( 'NONE', #19468 ) ;
#46361 = EDGE_CURVE ( 'NONE', #2701, #36062, #25682, .T. ) ;
#46360 = CARTESIAN_POINT ( 'NONE',  ( -128.4459734468149463, -1.025126265847081664, -157.4317124430720582 ) ) ;
#46362 = DIRECTION ( 'NONE',  ( 1.612977847700450206E-50, 0.000000000000000000, -1.000000000000000000 ) ) ;
#46363 = EDGE_CURVE ( 'NONE', #16830, #27540, #30785, .T. ) ;
#46364 =( BOUNDED_CURVE ( )  B_SPLINE_CURVE ( 3, ( #5831, #44544, #33044, #20724 ),
 .UNSPECIFIED., .F., .F. ) 
 B_SPLINE_CURVE_WITH_KNOTS ( ( 4, 4 ),
 ( 1.570796326794896558, 3.141592653589793116 ),
 .UNSPECIFIED. ) 
 CURVE ( )  GEOMETRIC_REPRESENTATION_ITEM ( )  RATIONAL_B_SPLINE_CURVE ( ( 1.000000000000000000, 0.8047378541243649375, 0.8047378541243649375, 1.000000000000000000 ) ) 
 REPRESENTATION_ITEM ( '' )  );
#46365 = ORIENTED_EDGE ( 'NONE', *, *, #22040, .T. ) ;
#46366 = CARTESIAN_POINT ( 'NONE',  ( -8.569579719062554446, -5.179646911086122962, 3.092310436554649655 ) ) ;
#46367 = DIRECTION ( 'NONE',  ( 1.000000000000000000, 0.000000000000000000, -4.758098676964956461E-16 ) ) ;
#46368 = ORIENTED_EDGE ( 'NONE', *, *, #37620, .T. ) ;
#46369 = AXIS2_PLACEMENT_3D ( 'NONE', #17877, #21233, #36922 ) ;
#46370 = ORIENTED_EDGE ( 'NONE', *, *, #18029, .T. ) ;
#46371 = ORIENTED_EDGE ( 'NONE', *, *, #47630, .F. ) ;
#46372 = LINE ( 'NONE', #3534, #34457 ) ;
#46373 = EDGE_CURVE ( 'NONE', #29572, #13781, #6033, .T. ) ;
#46374 =( BOUNDED_CURVE ( )  B_SPLINE_CURVE ( 3, ( #50214, #26925, #26173, #38999 ),
 .UNSPECIFIED., .F., .F. ) 
 B_SPLINE_CURVE_WITH_KNOTS ( ( 4, 4 ),
 ( 0.000000000000000000, 1.570796326794896558 ),
 .UNSPECIFIED. ) 
 CURVE ( )  GEOMETRIC_REPRESENTATION_ITEM ( )  RATIONAL_B_SPLINE_CURVE ( ( 1.000000000000000000, 0.8047378541243649375, 0.8047378541243649375, 1.000000000000000000 ) ) 
 REPRESENTATION_ITEM ( '' )  );
#46375 = CARTESIAN_POINT ( 'NONE',  ( 344.0000000000000000, 175.0000000000000284, -92.00000000000019895 ) ) ;
#46376 = ORIENTED_EDGE ( 'NONE', *, *, #37207, .F. ) ;
#46377 = AXIS2_PLACEMENT_3D ( 'NONE', #30885, #22906, #39592 ) ;
#46378 = CARTESIAN_POINT ( 'NONE',  ( -0.4692401618441021660, -1.180027720800729041, 9.975314328424614629 ) ) ;
#46379 = CARTESIAN_POINT ( 'NONE',  ( -7.721099712662037540, 1.750000000000023981, -120.2068387089191219 ) ) ;
#46380 = FACE_BOUND ( 'NONE', #29735, .T. ) ;
#46381 = CARTESIAN_POINT ( 'NONE',  ( -1.249999999999999778, 0.000000000000000000, 10.00000000000000000 ) ) ;
#46382 = DIRECTION ( 'NONE',  ( 0.000000000000000000, 0.000000000000000000, 1.000000000000000000 ) ) ;
#46383 = CYLINDRICAL_SURFACE ( 'NONE', #29027, 1.750000000000036193 ) ;
#46384 = LINE ( 'NONE', #15114, #31700 ) ;
#46385 = CARTESIAN_POINT ( 'NONE',  ( 193.3040265531851105, 1.750000000000010214, -39.18171244307202983 ) ) ;
#46386 = CARTESIAN_POINT ( 'NONE',  ( -18.67411147745623978, -27.51799019669813973, -3.760136334089591248 ) ) ;
#46387 = VERTEX_POINT ( 'NONE', #31804 ) ;
#46388 = PLANE ( 'NONE',  #23254 ) ;
#46389 = CARTESIAN_POINT ( 'NONE',  ( -50.00000000000000000, 50.00000000000000000, 800.0000000000000000 ) ) ;
#46390 = B_SPLINE_CURVE_WITH_KNOTS ( 'NONE', 3,
 ( #49734, #41834, #21844, #45400 ),
 .UNSPECIFIED., .F., .F.,
 ( 4, 4 ),
 ( 0.0009679537044786268220, 0.001281751046851330568 ),
 .UNSPECIFIED. ) ;
#46391 = CARTESIAN_POINT ( 'NONE',  ( 339.9999999999998863, -166.9999999999999432, 355.9999999999997726 ) ) ;
#46392 = FACE_OUTER_BOUND ( 'NONE', #17075, .T. ) ;
#46393 = ORIENTED_EDGE ( 'NONE', *, *, #7114, .T. ) ;
#46394 = CARTESIAN_POINT ( 'NONE',  ( 1.184758822850214388, -0.8459872530593102180, 9.938560165450805783 ) ) ;
#46395 = FACE_OUTER_BOUND ( 'NONE', #26880, .T. ) ;
#46396 = CARTESIAN_POINT ( 'NONE',  ( -1.377636575563021992, 0.6021164824561227036, 9.953784399990620813 ) ) ;
#46397 = DIRECTION ( 'NONE',  ( -1.000000000000000000, -0.000000000000000000, -0.000000000000000000 ) ) ;
#46398 = ADVANCED_FACE ( 'NONE', ( #47641 ), #4594, .F. ) ;
#46399 = VERTEX_POINT ( 'NONE', #43319 ) ;
#46400 =( NAMED_UNIT ( * ) PLANE_ANGLE_UNIT ( ) SI_UNIT ( $, .RADIAN. ) );
#46401 = ORIENTED_EDGE ( 'NONE', *, *, #5298, .F. ) ;
#46402 = CARTESIAN_POINT ( 'NONE',  ( -0.3862712429686729343, -1.188820645368946050, 10.00000000000000000 ) ) ;
#46403 = ORIENTED_EDGE ( 'NONE', *, *, #14200, .F. ) ;
#46404 = CARTESIAN_POINT ( 'NONE',  ( 344.0000000000000000, 174.9999999999996874, -342.0000000000002842 ) ) ;
#46405 = CARTESIAN_POINT ( 'NONE',  ( -114.9999999999984652, 16.00000000000000000, 35.00000000000000000 ) ) ;
#46406 = B_SPLINE_CURVE_WITH_KNOTS ( 'NONE', 3,
 ( #45003, #29634, #37112, #20933, #45256, #9131 ),
 .UNSPECIFIED., .F., .F.,
 ( 4, 2, 4 ),
 ( 4.943961906533900219E-17, 0.009882509389272372408, 0.01976501877854469624 ),
 .UNSPECIFIED. ) ;
#46407 = EDGE_LOOP ( 'NONE', ( #40975, #30957, #10811, #32854, #5057, #19999 ) ) ;
#46408 = SURFACE_STYLE_USAGE ( .BOTH. , #31055 ) ;
#46409 = VERTEX_POINT ( 'NONE', #43577 ) ;
#46410 = AXIS2_PLACEMENT_3D ( 'NONE', #25766, #14970, #46231 ) ;
#46411 = VERTEX_POINT ( 'NONE', #12280 ) ;
#46412 = CARTESIAN_POINT ( 'NONE',  ( -86.69597344681494633, 1.750000000000010214, -39.18171244307202983 ) ) ;
#46413 = CARTESIAN_POINT ( 'NONE',  ( 359.9999999999999432, -181.0000000000001421, -356.0000000000003411 ) ) ;
#46414 = ORIENTED_EDGE ( 'NONE', *, *, #32192, .F. ) ;
#46415 = CARTESIAN_POINT ( 'NONE',  ( -1.011271242968683426, -0.7347315653655928092, -10.00000000000000000 ) ) ;
#46416 = CARTESIAN_POINT ( 'NONE',  ( 33.30402655318503946, -1.750000000000009992, 0.8182875569279768335 ) ) ;
#46417 = CARTESIAN_POINT ( 'NONE',  ( -48.44597344681495343, 0.000000000000000000, -80.93171244307204404 ) ) ;
#46418 = ORIENTED_EDGE ( 'NONE', *, *, #26488, .F. ) ;
#46419 = EDGE_LOOP ( 'NONE', ( #40482, #35769, #30793, #10119 ) ) ;
#46420 = DIRECTION ( 'NONE',  ( 0.000000000000000000, -1.000000000000000000, 0.000000000000000000 ) ) ;
#46421 = PLANE ( 'NONE',  #30518 ) ;
#46422 = VERTEX_POINT ( 'NONE', #32305 ) ;
#46423 = VECTOR ( 'NONE', #41550, 1000.000000000000000 ) ;
#46424 = DIRECTION ( 'NONE',  ( -1.000000000000000000, -0.000000000000000000, 0.000000000000000000 ) ) ;
#46425 = CARTESIAN_POINT ( 'NONE',  ( 339.9999999999999432, 174.9999999999996589, -344.0000000000002842 ) ) ;
#46426 = ORIENTED_EDGE ( 'NONE', *, *, #5254, .F. ) ;
#46427 = FACE_OUTER_BOUND ( 'NONE', #37763, .T. ) ;
#46428 = ADVANCED_FACE ( 'NONE', ( #43074 ), #16383, .F. ) ;
#46429 = ORIENTED_EDGE ( 'NONE', *, *, #19317, .T. ) ;
#46430 = CARTESIAN_POINT ( 'NONE',  ( 33.30402655318503946, -1.750000000000009992, -159.1817124430720298 ) ) ;
#46431 = CARTESIAN_POINT ( 'NONE',  ( -8.445973446814976526, 0.000000000000000000, -77.43171244307198720 ) ) ;
#46432 = DIRECTION ( 'NONE',  ( 6.203854594147707562E-25, -2.067951531382569187E-25, 1.000000000000000000 ) ) ;
#46433 = CARTESIAN_POINT ( 'NONE',  ( 2.500000000000002665, 204.9999999999999716, -230.2499999999999716 ) ) ;
#46434 = VERTEX_POINT ( 'NONE', #7945 ) ;
#46435 = CARTESIAN_POINT ( 'NONE',  ( 34.08355720199905647, -2.371364769369109116, 7.455576670931136185 ) ) ;
#46436 = CARTESIAN_POINT ( 'NONE',  ( -24.47767542868268364, 23.18653802921800278, 8.807470649214879543 ) ) ;
#46437 = CARTESIAN_POINT ( 'NONE',  ( -215.0000000000000568, -173.0000000000000000, 372.0000000000000000 ) ) ;
#46438 = ORIENTED_EDGE ( 'NONE', *, *, #16412, .F. ) ;
#46439 = ORIENTED_EDGE ( 'NONE', *, *, #35548, .T. ) ;
#46440 = DIRECTION ( 'NONE',  ( 0.3789361732451775877, -1.425365463543235410E-14, -0.9254228096423284811 ) ) ;
#46441 = CARTESIAN_POINT ( 'NONE',  ( 32.27890028733795447, -1.750000000000009548, 39.79316129108089228 ) ) ;
#46442 = CARTESIAN_POINT ( 'NONE',  ( 0.000000000000000000, 17.00000000000000000, 0.000000000000000000 ) ) ;
#46443 = DIRECTION ( 'NONE',  ( 1.000000000000000000, 0.000000000000000000, 0.000000000000000000 ) ) ;
#46444 = PLANE ( 'NONE',  #1204 ) ;
#46445 = CARTESIAN_POINT ( 'NONE',  ( 7.359817328027030925, 15.16751262232805431, 2.590526750877053086 ) ) ;
#46446 = ORIENTED_EDGE ( 'NONE', *, *, #7650, .F. ) ;
#46447 = LINE ( 'NONE', #22632, #177 ) ;
#46448 = CYLINDRICAL_SURFACE ( 'NONE', #44166, 1.750000000000001554 ) ;
#46449 = CARTESIAN_POINT ( 'NONE',  ( -164.9459734468149463, 2.143131898507890731E-16, -165.0000000000000000 ) ) ;
#46450 = CARTESIAN_POINT ( 'NONE',  ( -166.6959734468149463, 1.750000000000010658, 80.81828755692798438 ) ) ;
#46452 = ORIENTED_EDGE ( 'NONE', *, *, #30355, .T. ) ;
#46451 = CIRCLE ( 'NONE', #23574, 4.000000000000003553 ) ;
#46453 = CARTESIAN_POINT ( 'NONE',  ( 344.0000000000000000, 165.0000000000001990, -340.0000000000002842 ) ) ;
#46454 = CARTESIAN_POINT ( 'NONE',  ( 339.9999999999999432, 181.0000000000000284, -342.0000000000001705 ) ) ;
#46455 = ORIENTED_EDGE ( 'NONE', *, *, #47222, .T. ) ;
#46456 = CARTESIAN_POINT ( 'NONE',  ( -7.749480817862350435, -14.85497772329513211, 9.403735324607438884 ) ) ;
#46457 = CARTESIAN_POINT ( 'NONE',  ( -64.99999999999846523, 16.00000000000000000, 60.00000000000000000 ) ) ;
#46458 = CARTESIAN_POINT ( 'NONE',  ( 168.9999999999999716, -164.9999999999999432, -342.0000000000001137 ) ) ;
#46459 = ORIENTED_EDGE ( 'NONE', *, *, #458, .T. ) ;
#46460 = CARTESIAN_POINT ( 'NONE',  ( 181.0000000000000000, -180.9999999999999716, -350.0000000000001705 ) ) ;
#46461 = CARTESIAN_POINT ( 'NONE',  ( 153.3040265531850537, 1.750000000000009992, 0.8182875569279768335 ) ) ;
#46462 = ORIENTED_EDGE ( 'NONE', *, *, #22248, .T. ) ;
#46463 = DIRECTION ( 'NONE',  ( 1.000000000000000000, 0.000000000000000000, 0.000000000000000000 ) ) ;
#46464 = UNCERTAINTY_MEASURE_WITH_UNIT (LENGTH_MEASURE( 1.000000000000000082E-05 ), #48263, 'distance_accuracy_value', 'NONE');
#46465 = DIRECTION ( 'NONE',  ( 0.000000000000000000, 0.000000000000000000, 1.000000000000000000 ) ) ;
#46466 = ORIENTED_EDGE ( 'NONE', *, *, #37276, .T. ) ;
#46467 = EDGE_LOOP ( 'NONE', ( #2884, #20331, #15421, #4970 ) ) ;
#46468 = DIRECTION ( 'NONE',  ( -0.000000000000000000, -1.000000000000000000, -0.000000000000000000 ) ) ;
#46469 = DIRECTION ( 'NONE',  ( -0.000000000000000000, -1.000000000000000000, -0.000000000000000000 ) ) ;
#46470 = ORIENTED_EDGE ( 'NONE', *, *, #47785, .F. ) ;
#46471 = EDGE_CURVE ( 'NONE', #32541, #20108, #24596, .T. ) ;
#46472 = VERTEX_POINT ( 'NONE', #27941 ) ;
#46473 = CARTESIAN_POINT ( 'NONE',  ( -44.94597344681493922, -1.025126265847089435, -77.43171244307200141 ) ) ;
#46474 = CARTESIAN_POINT ( 'NONE',  ( 356.0000000000006253, 167.0000000000000000, -342.0000000000001137 ) ) ;
#46475 = CARTESIAN_POINT ( 'NONE',  ( 168.9999999999999716, 165.0000000000000000, -344.0000000000001137 ) ) ;
#46476 = VERTEX_POINT ( 'NONE', #20485 ) ;
#46477 = DIRECTION ( 'NONE',  ( 0.000000000000000000, -1.000000000000000000, 0.000000000000000000 ) ) ;
#46478 = ADVANCED_FACE ( 'NONE', ( #31554 ), #39753, .T. ) ;
#46479 = ORIENTED_EDGE ( 'NONE', *, *, #31186, .T. ) ;
#46480 = CARTESIAN_POINT ( 'NONE',  ( 0.3862712429686894766, -1.188820645368940276, -10.00000000000000000 ) ) ;
#46481 = ADVANCED_FACE ( 'NONE', ( #23842 ), #12044, .T. ) ;
#46482 = DIRECTION ( 'NONE',  ( -0.000000000000000000, -1.000000000000000000, -0.000000000000000000 ) ) ;
#46483 = EDGE_CURVE ( 'NONE', #3284, #25760, #4820, .T. ) ;
#46484 = CARTESIAN_POINT ( 'NONE',  ( 1.249999999999999778, -0.000000000000000000, -3.333333333333333481 ) ) ;
#46485 = ORIENTED_EDGE ( 'NONE', *, *, #33145, .F. ) ;
#46486 = AXIS2_PLACEMENT_3D ( 'NONE', #46752, #10628, #26291 ) ;
#46487 = ORIENTED_EDGE ( 'NONE', *, *, #43537, .F. ) ;
#46488 = ORIENTED_EDGE ( 'NONE', *, *, #11133, .T. ) ;
#46489 = CARTESIAN_POINT ( 'NONE',  ( -206.6959734468149463, 1.750000000000010658, 120.8182875569279702 ) ) ;
#46490 = SURFACE_SIDE_STYLE ('',( #11137 ) ) ;
#46491 = DIRECTION ( 'NONE',  ( -1.000000000000000000, -0.000000000000000000, -0.000000000000000000 ) ) ;
#46492 = ORIENTED_EDGE ( 'NONE', *, *, #13614, .T. ) ;
#46493 = DIRECTION ( 'NONE',  ( 1.000000000000000000, 0.000000000000000000, 0.000000000000000000 ) ) ;
#46494 = EDGE_LOOP ( 'NONE', ( #33302, #29968, #32926 ) ) ;
#46495 = DIRECTION ( 'NONE',  ( -0.000000000000000000, -0.000000000000000000, -1.000000000000000000 ) ) ;
#46496 = ORIENTED_EDGE ( 'NONE', *, *, #29451, .F. ) ;
#46497 =( BOUNDED_CURVE ( )  B_SPLINE_CURVE ( 3, ( #36542, #872, #37048, #17013 ),
 .UNSPECIFIED., .F., .F. ) 
 B_SPLINE_CURVE_WITH_KNOTS ( ( 4, 4 ),
 ( 3.141592653589793116, 4.712388980384689674 ),
 .UNSPECIFIED. ) 
 CURVE ( )  GEOMETRIC_REPRESENTATION_ITEM ( )  RATIONAL_B_SPLINE_CURVE ( ( 1.000000000000000000, 0.8047378541243649375, 0.8047378541243649375, 1.000000000000000000 ) ) 
 REPRESENTATION_ITEM ( '' )  );
#46498 = LINE ( 'NONE', #19592, #36732 ) ;
#46499 = CARTESIAN_POINT ( 'NONE',  ( -0.3862712429686809279, -1.188820645368943163, -10.00000000000000000 ) ) ;
#46500 = PLANE ( 'NONE',  #50366 ) ;
#46501 = DIRECTION ( 'NONE',  ( 0.000000000000000000, -1.000000000000000000, 0.000000000000000000 ) ) ;
#46502 = ORIENTED_EDGE ( 'NONE', *, *, #49974, .T. ) ;
#46503 = ORIENTED_EDGE ( 'NONE', *, *, #49346, .F. ) ;
#46504 = PLANE ( 'NONE',  #17368 ) ;
#46505 =( BOUNDED_CURVE ( )  B_SPLINE_CURVE ( 3, ( #22730, #19390, #6833, #30435 ),
 .UNSPECIFIED., .F., .F. ) 
 B_SPLINE_CURVE_WITH_KNOTS ( ( 4, 4 ),
 ( 1.570796326794896558, 3.141592653589793116 ),
 .UNSPECIFIED. ) 
 CURVE ( )  GEOMETRIC_REPRESENTATION_ITEM ( )  RATIONAL_B_SPLINE_CURVE ( ( 1.000000000000000000, 0.8047378541243649375, 0.8047378541243649375, 1.000000000000000000 ) ) 
 REPRESENTATION_ITEM ( '' )  );
#46506 = CARTESIAN_POINT ( 'NONE',  ( -2.188678504086925880, 0.3267089737526900350, 9.881002359080270026 ) ) ;
#46507 = B_SPLINE_SURFACE_WITH_KNOTS ( 'NONE', 3, 3, ( 
 ( #23874, #36193, #23615, #15662 ),
 ( #19498, #46922, #35186, #542 ),
 ( #35441, #12563, #43864, #4631 ),
 ( #31331, #43116, #11825, #4121 ) ),
 .UNSPECIFIED., .F., .F., .F.,
 ( 4, 4 ),
 ( 4, 4 ),
 ( 0.000000000000000000, 1.000000000000000000 ),
 ( 0.000000000000000000, 1.000000000000000000 ),
 .UNSPECIFIED. ) ;
#46508 = CARTESIAN_POINT ( 'NONE',  ( -168.4459734468149747, -1.025126265847089213, 162.5682875569279133 ) ) ;
#46509 = CARTESIAN_POINT ( 'NONE',  ( -15.98719783915689163, 4.501063718205989161, 3.266473740018926541 ) ) ;
#46510 = ADVANCED_FACE ( 'NONE', ( #12789 ), #15886, .F. ) ;
#46511 = EDGE_CURVE ( 'NONE', #16197, #3985, #11583, .T. ) ;
#46512 = EDGE_CURVE ( 'NONE', #20771, #38870, #41267, .T. ) ;
#46513 = EDGE_CURVE ( 'NONE', #21378, #21529, #32051, .T. ) ;
#46514 = LINE ( 'NONE', #3957, #33897 ) ;
#46515 = PLANE ( 'NONE',  #22093 ) ;
#46516 = EDGE_CURVE ( 'NONE', #16307, #32346, #8514, .T. ) ;
#46517 = ORIENTED_EDGE ( 'NONE', *, *, #18007, .T. ) ;
#46518 = DIRECTION ( 'NONE',  ( -0.000000000000000000, -0.000000000000000000, -1.000000000000000000 ) ) ;
#46519 = EDGE_CURVE ( 'NONE', #22924, #42094, #23581, .T. ) ;
#46520 =( BOUNDED_CURVE ( )  B_SPLINE_CURVE ( 3, ( #3618, #11324, #39051, #34692 ),
 .UNSPECIFIED., .F., .F. ) 
 B_SPLINE_CURVE_WITH_KNOTS ( ( 4, 4 ),
 ( 1.570796326794896558, 3.141592653589793116 ),
 .UNSPECIFIED. ) 
 CURVE ( )  GEOMETRIC_REPRESENTATION_ITEM ( )  RATIONAL_B_SPLINE_CURVE ( ( 1.000000000000000000, 0.8047378541243649375, 0.8047378541243649375, 1.000000000000000000 ) ) 
 REPRESENTATION_ITEM ( '' )  );
#46521 = CARTESIAN_POINT ( 'NONE',  ( 168.9999999999999716, 175.0000000000000284, -356.0000000000001705 ) ) ;
#46522 = ORIENTED_EDGE ( 'NONE', *, *, #49008, .T. ) ;
#46523 = VECTOR ( 'NONE', #17517, 999.9999999999998863 ) ;
#46524 = CARTESIAN_POINT ( 'NONE',  ( 29.99999999999997158, 16.00000000000000000, -114.9999999999999858 ) ) ;
#46525 = CARTESIAN_POINT ( 'NONE',  ( 0.000000000000000000, -165.1999999999999602, 359.7999999999997840 ) ) ;
#46526 = DIRECTION ( 'NONE',  ( -0.000000000000000000, -0.000000000000000000, -1.000000000000000000 ) ) ;
#46527 = EDGE_LOOP ( 'NONE', ( #23085, #32285, #10914, #1286, #17760, #34281 ) ) ;
#46528 = EDGE_LOOP ( 'NONE', ( #48011, #2382, #31762, #19475, #36333, #31130 ) ) ;
#46529 = EDGE_CURVE ( 'NONE', #21982, #2527, #8707, .T. ) ;
#46530 = CARTESIAN_POINT ( 'NONE',  ( 4.395207584381303434, 3.942437227415936718, 9.586754400234161366 ) ) ;
#46531 = CARTESIAN_POINT ( 'NONE',  ( 3.229232847726260403, -16.57333684275945629, 9.178419661560148768 ) ) ;
#46532 = EDGE_CURVE ( 'NONE', #1662, #40121, #36398, .T. ) ;
#46533 = ORIENTED_EDGE ( 'NONE', *, *, #29761, .F. ) ;
#46534 = ADVANCED_FACE ( 'NONE', ( #16903 ), #17524, .T. ) ;
#46535 = ORIENTED_EDGE ( 'NONE', *, *, #2659, .T. ) ;
#46536 = CARTESIAN_POINT ( 'NONE',  ( 0.1287570809895660084, -0.3962735484563127408, 10.00000000000000000 ) ) ;
#46537 = CARTESIAN_POINT ( 'NONE',  ( 34.38425513258721367, -36.82177522737821107, 8.807470649214879543 ) ) ;
#46538 = DIRECTION ( 'NONE',  ( 1.000000000000000000, 0.000000000000000000, 0.000000000000000000 ) ) ;
#46539 = ORIENTED_EDGE ( 'NONE', *, *, #13609, .T. ) ;
#46540 = ORIENTED_EDGE ( 'NONE', *, *, #25353, .T. ) ;
#46541 = VERTEX_POINT ( 'NONE', #41243 ) ;
#46542 = PLANE ( 'NONE',  #35729 ) ;
#46543 = CARTESIAN_POINT ( 'NONE',  ( -48.44597344681496054, -1.025126265847089213, -160.9317124430720014 ) ) ;
#46544 = VERTEX_POINT ( 'NONE', #48894 ) ;
#46545 = DIRECTION ( 'NONE',  ( 1.000000000000000000, 0.000000000000000000, 7.793956916774525800E-48 ) ) ;
#46546 = CARTESIAN_POINT ( 'NONE',  ( 22.51959565330788493, 30.03043964857266346, -6.568693074176341185 ) ) ;
#46547 = ORIENTED_EDGE ( 'NONE', *, *, #11238, .F. ) ;
#46548 = ORIENTED_EDGE ( 'NONE', *, *, #24041, .T. ) ;
#46549 = CARTESIAN_POINT ( 'NONE',  ( 35.05402655318504657, 2.143131898507880377E-16, -37.43171244307200141 ) ) ;
#46550 = ADVANCED_FACE ( 'NONE', ( #45317 ), #48396, .F. ) ;
#46551 = LINE ( 'NONE', #23512, #35805 ) ;
#46552 = LINE ( 'NONE', #31730, #32263 ) ;
#46553 = UNCERTAINTY_MEASURE_WITH_UNIT (LENGTH_MEASURE( 1.000000000000000082E-05 ), #52, 'distance_accuracy_value', 'NONE');
#46554 = EDGE_LOOP ( 'NONE', ( #42374, #16778, #39482, #26190 ) ) ;
#46555 = ORIENTED_EDGE ( 'NONE', *, *, #47830, .F. ) ;
#46556 = CARTESIAN_POINT ( 'NONE',  ( -208.4459734468149463, 0.000000000000000000, -77.43171244307204404 ) ) ;
#46557 =( NAMED_UNIT ( * ) SI_UNIT ( $, .STERADIAN. ) SOLID_ANGLE_UNIT ( ) );
#46558 = VECTOR ( 'NONE', #4765, 1000.000000000000000 ) ;
#46559 = CARTESIAN_POINT ( 'NONE',  ( 168.9999999999999716, -81.49999999999995737, -115.0000000000001563 ) ) ;
#46560 = CARTESIAN_POINT ( 'NONE',  ( 210.0000000000000568, 0.000000000000000000, 120.8182875569279702 ) ) ;
#46561 = CARTESIAN_POINT ( 'NONE',  ( -206.6959734468149463, 1.750000000000010658, 80.81828755692798438 ) ) ;
#46562 = AXIS2_PLACEMENT_3D ( 'NONE', #939, #36098, #43766 ) ;
#46563 = EDGE_CURVE ( 'NONE', #34063, #16264, #43031, .T. ) ;
#46564 = CARTESIAN_POINT ( 'NONE',  ( 9.260964247899973856, -13.84230907185609460, -9.683996418299976483 ) ) ;
#46565 = ORIENTED_EDGE ( 'NONE', *, *, #9010, .T. ) ;
#46566 = CARTESIAN_POINT ( 'NONE',  ( 34.08406891383362591, -15.63733501198463038, -8.192531242611266862 ) ) ;
#46567 = CARTESIAN_POINT ( 'NONE',  ( 10.00000000000000000, 249.9999999999999716, 225.0000000000000000 ) ) ;
#46568 = CARTESIAN_POINT ( 'NONE',  ( -10.50000000000003730, 13.48684210526314331, -19.99999999999999645 ) ) ;
#46569 = CLOSED_SHELL ( 'NONE', ( #20072, #42845, #6878, #22801 ) ) ;
#46570 = CARTESIAN_POINT ( 'NONE',  ( -87.72109971266203843, 1.750000000000009548, -78.15658617722490931 ) ) ;
#46571 = EDGE_CURVE ( 'NONE', #23363, #30968, #48144, .T. ) ;
#46572 = EDGE_CURVE ( 'NONE', #50186, #9851, #24915, .T. ) ;
#46573 = ORIENTED_EDGE ( 'NONE', *, *, #28499, .F. ) ;
#46574 = CARTESIAN_POINT ( 'NONE',  ( 1.011271242968677653, 0.7347315653656002477, 3.333333333333333481 ) ) ;
#46575 = EDGE_CURVE ( 'NONE', #22827, #39841, #13277, .T. ) ;
#46576 = DIRECTION ( 'NONE',  ( -1.000000000000000000, 0.000000000000000000, -1.586032872232979935E-16 ) ) ;
#46577 = CARTESIAN_POINT ( 'NONE',  ( 9.999999999999996447, -34.54492135858216528, 5.000000000000000000 ) ) ;
#46578 = EDGE_CURVE ( 'NONE', #22476, #14628, #36932, .T. ) ;
#46579 = ORIENTED_EDGE ( 'NONE', *, *, #21532, .F. ) ;
#46580 = LINE ( 'NONE', #4030, #7378 ) ;
#46581 = EDGE_LOOP ( 'NONE', ( #43596, #31684, #7593, #15130 ) ) ;
#46582 = CARTESIAN_POINT ( 'NONE',  ( 343.9999999999999432, -183.0000000000001421, 358.0000000000001137 ) ) ;
#46583 = CARTESIAN_POINT ( 'NONE',  ( 71.55402655318505367, 0.000000000000000000, 39.06828755692795596 ) ) ;
#46584 = DIRECTION ( 'NONE',  ( 1.000000000000000000, 0.000000000000000000, 0.000000000000000000 ) ) ;
#46585 = CARTESIAN_POINT ( 'NONE',  ( -0.9942667885118393611, 0.7728247605419426014, 9.974012008644018934 ) ) ;
#46586 = EDGE_CURVE ( 'NONE', #33796, #12365, #29697, .T. ) ;
#46587 = ORIENTED_EDGE ( 'NONE', *, *, #28702, .F. ) ;
#46588 = CARTESIAN_POINT ( 'NONE',  ( 210.0000000000000568, 2.143131898507881856E-16, -120.9317124430720582 ) ) ;
#46589 = ORIENTED_EDGE ( 'NONE', *, *, #50436, .F. ) ;
#46590 = VERTEX_POINT ( 'NONE', #1751 ) ;
#46591 = CARTESIAN_POINT ( 'NONE',  ( -0.2778388845795317086, 1.251314014313103851, 9.976582533991678048 ) ) ;
#46592 = VECTOR ( 'NONE', #6032, 1000.000000000000000 ) ;
#46593 = VECTOR ( 'NONE', #28262, 1000.000000000000000 ) ;
#46594 = ORIENTED_EDGE ( 'NONE', *, *, #50000, .F. ) ;
#46595 = EDGE_CURVE ( 'NONE', #42421, #50239, #9528, .T. ) ;
#46596 = LINE ( 'NONE', #23025, #26239 ) ;
#46597 = LINE ( 'NONE', #31768, #15086 ) ;
#46598 =( BOUNDED_CURVE ( )  B_SPLINE_CURVE ( 3, ( #29818, #13153, #29062, #49005 ),
 .UNSPECIFIED., .F., .F. ) 
 B_SPLINE_CURVE_WITH_KNOTS ( ( 4, 4 ),
 ( 1.570796326794896558, 3.141592653589793116 ),
 .UNSPECIFIED. ) 
 CURVE ( )  GEOMETRIC_REPRESENTATION_ITEM ( )  RATIONAL_B_SPLINE_CURVE ( ( 1.000000000000000000, 0.8047378541243649375, 0.8047378541243649375, 1.000000000000000000 ) ) 
 REPRESENTATION_ITEM ( '' )  );
#46599 = VECTOR ( 'NONE', #38303, 1000.000000000000000 ) ;
#46600 = AXIS2_PLACEMENT_3D ( 'NONE', #17181, #10241, #9475 ) ;
#46601 = AXIS2_PLACEMENT_3D ( 'NONE', #41062, #5905, #25930 ) ;
#46602 = CARTESIAN_POINT ( 'NONE',  ( 31.55402655318503236, 0.000000000000000000, 165.0000000000000000 ) ) ;
#46603 = ORIENTED_EDGE ( 'NONE', *, *, #38493, .T. ) ;
#46604 = CARTESIAN_POINT ( 'NONE',  ( 31.55402655318503236, 1.025126265847089213, 162.5682875569279133 ) ) ;
#46605 = DIRECTION ( 'NONE',  ( 0.5407575913134976542, 0.000000000000000000, -0.8411784753765542133 ) ) ;
#46606 = AXIS2_PLACEMENT_3D ( 'NONE', #49682, #8352, #26886 ) ;
#46607 = ORIENTED_EDGE ( 'NONE', *, *, #41238, .F. ) ;
#46608 = CARTESIAN_POINT ( 'NONE',  ( -9.907356528110963012, 1.358045148327947427, 0.000000000000000000 ) ) ;
#46609 = LINE ( 'NONE', #3031, #13839 ) ;
#46610 = ORIENTED_EDGE ( 'NONE', *, *, #32558, .T. ) ;
#46611 = VERTEX_POINT ( 'NONE', #44317 ) ;
#46612 = ORIENTED_EDGE ( 'NONE', *, *, #29011, .T. ) ;
#46613 = CARTESIAN_POINT ( 'NONE',  ( 0.000000000000000000, 169.0000000000000000, 357.9999999999997726 ) ) ;
#46614 = LINE ( 'NONE', #42789, #38143 ) ;
#46615 = EDGE_LOOP ( 'NONE', ( #1982, #41112, #44393, #49718 ) ) ;
#46616 = LINE ( 'NONE', #26903, #39760 ) ;
#46617 = CARTESIAN_POINT ( 'NONE',  ( -34.38425513258694366, 36.82177522737846687, 8.807470649214879543 ) ) ;
#46618 = PLANE ( 'NONE',  #164 ) ;
#46619 = CARTESIAN_POINT ( 'NONE',  ( 0.3334286742302847717, 1.332255019526881412, 9.946805383069621698 ) ) ;
#46620 = CARTESIAN_POINT ( 'NONE',  ( 214.9999999999999432, -173.0000000000000000, 372.0000000000000000 ) ) ;
#46621 = CARTESIAN_POINT ( 'NONE',  ( 9.998889670239195837, 0.1490146381531976816, 9.282506307616472441 ) ) ;
#46622 = CARTESIAN_POINT ( 'NONE',  ( -165.0000000000000284, 15.00000000000000000, 115.0000000000000142 ) ) ;
#46623 = CARTESIAN_POINT ( 'NONE',  ( -6.695973446814940111, 1.750000000000023315, 0.8182875569279768335 ) ) ;
#46624 = FACE_OUTER_BOUND ( 'NONE', #13943, .T. ) ;
#46625 = EDGE_LOOP ( 'NONE', ( #1520, #30122, #45346, #46738 ) ) ;
#46626 = VECTOR ( 'NONE', #27197, 1000.000000000000000 ) ;
#46627 = CARTESIAN_POINT ( 'NONE',  ( -206.6959734468149463, -1.750000000000010658, -119.1817124430720440 ) ) ;
#46628 = DIRECTION ( 'NONE',  ( -1.000000000000000000, 0.000000000000000000, -7.793956916774525800E-48 ) ) ;
#46629 = ADVANCED_FACE ( 'NONE', ( #24848, #14034 ), #13780, .T. ) ;
#46630 = VECTOR ( 'NONE', #35290, 1000.000000000000000 ) ;
#46631 = EDGE_CURVE ( 'NONE', #34498, #37542, #9693, .T. ) ;
#46632 = DIRECTION ( 'NONE',  ( 0.000000000000000000, 0.000000000000000000, -1.000000000000000000 ) ) ;
#46633 = CARTESIAN_POINT ( 'NONE',  ( 33.30402655318503946, 0.000000000000000000, 165.0000000000000000 ) ) ;
#46634 = ORIENTED_EDGE ( 'NONE', *, *, #42492, .T. ) ;
#46635 = CARTESIAN_POINT ( 'NONE',  ( 30.00000000000062172, 16.00000000000000000, -54.99999999999999289 ) ) ;
#46636 = VECTOR ( 'NONE', #50512, 1000.000000000000000 ) ;
#46637 = DIRECTION ( 'NONE',  ( 0.8090169943749465631, 0.5877852522924742473, 0.000000000000000000 ) ) ;
#46638 = EDGE_CURVE ( 'NONE', #40480, #7451, #5847, .T. ) ;
#46639 = FACE_OUTER_BOUND ( 'NONE', #19494, .T. ) ;
#46640 = CARTESIAN_POINT ( 'NONE',  ( -87.72109971266203843, 1.750000000000009326, 1.843413822775066269 ) ) ;
#46641 = DIRECTION ( 'NONE',  ( 0.000000000000000000, -1.000000000000000000, 0.000000000000000000 ) ) ;
#46642 = EDGE_CURVE ( 'NONE', #50507, #21498, #47792, .T. ) ;
#46643 = EDGE_CURVE ( 'NONE', #16943, #14950, #23000, .T. ) ;
#46644 = AXIS2_PLACEMENT_3D ( 'NONE', #32752, #25552, #8888 ) ;
#46645 = EDGE_LOOP ( 'NONE', ( #8860, #1485, #36165, #44573, #12008, #10096 ) ) ;
#46646 = DIRECTION ( 'NONE',  ( -0.000000000000000000, -1.000000000000000000, -0.000000000000000000 ) ) ;
#46647 = VERTEX_POINT ( 'NONE', #10956 ) ;
#46648 = LINE ( 'NONE', #11548, #19638 ) ;
#46649 = ORIENTED_EDGE ( 'NONE', *, *, #3966, .F. ) ;
#46650 = EDGE_CURVE ( 'NONE', #35217, #1861, #30459, .T. ) ;
#46651 = LINE ( 'NONE', #34912, #20521 ) ;
#46652 = CARTESIAN_POINT ( 'NONE',  ( -126.6959734468149321, 1.749999999999997335, -79.18171244307201562 ) ) ;
#46653 = EDGE_CURVE ( 'NONE', #9039, #48199, #13218, .T. ) ;
#46654 = VERTEX_POINT ( 'NONE', #49893 ) ;
#46655 = CARTESIAN_POINT ( 'NONE',  ( 154.3291528190321458, 1.750000000000009548, 159.7931612910809065 ) ) ;
#46656 = ORIENTED_EDGE ( 'NONE', *, *, #18029, .F. ) ;
#46657 =( BOUNDED_CURVE ( )  B_SPLINE_CURVE ( 3, ( #5821, #21215, #44534, #12764 ),
 .UNSPECIFIED., .F., .F. ) 
 B_SPLINE_CURVE_WITH_KNOTS ( ( 4, 4 ),
 ( 1.570796326794896558, 3.141592653589793116 ),
 .UNSPECIFIED. ) 
 CURVE ( )  GEOMETRIC_REPRESENTATION_ITEM ( )  RATIONAL_B_SPLINE_CURVE ( ( 1.000000000000000000, 0.8047378541243649375, 0.8047378541243649375, 1.000000000000000000 ) ) 
 REPRESENTATION_ITEM ( '' )  );
#46658 = VERTEX_POINT ( 'NONE', #50150 ) ;
#46659 = CARTESIAN_POINT ( 'NONE',  ( 191.5540265531851105, 0.000000000000000000, 82.56828755692798438 ) ) ;
#46660 = FACE_OUTER_BOUND ( 'NONE', #4596, .T. ) ;
#46661 = ORIENTED_EDGE ( 'NONE', *, *, #12070, .T. ) ;
#46662 = CARTESIAN_POINT ( 'NONE',  ( -36.08557433729205144, 35.58569447144795816, 7.455576670931136185 ) ) ;
#46663 = CARTESIAN_POINT ( 'NONE',  ( -1.424123654778022274, -0.3625862473323341328, 9.958264684458713489 ) ) ;
#46664 = CARTESIAN_POINT ( 'NONE',  ( 177.5000000000000284, 102.5000000000000142, -10.00000000000000000 ) ) ;
#46665 =( BOUNDED_CURVE ( )  B_SPLINE_CURVE ( 3, ( #1383, #8576, #24229, #20361 ),
 .UNSPECIFIED., .F., .F. ) 
 B_SPLINE_CURVE_WITH_KNOTS ( ( 4, 4 ),
 ( 0.000000000000000000, 1.570796326794896558 ),
 .UNSPECIFIED. ) 
 CURVE ( )  GEOMETRIC_REPRESENTATION_ITEM ( )  RATIONAL_B_SPLINE_CURVE ( ( 1.000000000000000000, 0.8047378541243649375, 0.8047378541243649375, 1.000000000000000000 ) ) 
 REPRESENTATION_ITEM ( '' )  );
#46666 = ORIENTED_EDGE ( 'NONE', *, *, #44738, .F. ) ;
#46667 = CARTESIAN_POINT ( 'NONE',  ( 165.0000000000000000, -81.49999999999995737, -115.0000000000001563 ) ) ;
#46668 = VECTOR ( 'NONE', #18916, 1000.000000000000000 ) ;
#46669 = LINE ( 'NONE', #39277, #33792 ) ;
#46670 = VECTOR ( 'NONE', #15709, 1000.000000000000000 ) ;
#46671 = VECTOR ( 'NONE', #16029, 1000.000000000000000 ) ;
#46672 = ORIENTED_EDGE ( 'NONE', *, *, #38813, .F. ) ;
#46673 = DIRECTION ( 'NONE',  ( 0.000000000000000000, -0.000000000000000000, 1.000000000000000000 ) ) ;
#46674 = LINE ( 'NONE', #27220, #47706 ) ;
#46675 = ORIENTED_EDGE ( 'NONE', *, *, #49014, .F. ) ;
#46676 = DIRECTION ( 'NONE',  ( 0.000000000000000000, 0.000000000000000000, 1.000000000000000000 ) ) ;
#46677 = VECTOR ( 'NONE', #32286, 1000.000000000000000 ) ;
#46678 = VECTOR ( 'NONE', #39799, 1000.000000000000000 ) ;
#46679 = CARTESIAN_POINT ( 'NONE',  ( -87.72109971266203843, 1.750000000000010436, 119.7931612910808781 ) ) ;
#46680 = VERTEX_POINT ( 'NONE', #45811 ) ;
#46681 = ADVANCED_FACE ( 'NONE', ( #3242 ), #49657, .F. ) ;
#46682 = CARTESIAN_POINT ( 'NONE',  ( 355.9999999999999432, -183.0000000000001421, -349.9999999999998863 ) ) ;
#46683 = CARTESIAN_POINT ( 'NONE',  ( 357.9999999999999432, -181.0000000000001421, -356.0000000000003979 ) ) ;
#46684 = CARTESIAN_POINT ( 'NONE',  ( 30.00000000000029132, 17.00000000000000000, -84.99999999999998579 ) ) ;
#46685 = AXIS2_PLACEMENT_3D ( 'NONE', #27963, #36707, #43601 ) ;
#46686 = CARTESIAN_POINT ( 'NONE',  ( -128.4459734468149179, 0.000000000000000000, -0.9317124430719969652 ) ) ;
#46687 = ORIENTED_EDGE ( 'NONE', *, *, #47287, .T. ) ;
#46688 = CARTESIAN_POINT ( 'NONE',  ( -6.508636631827791064, -15.75743548351446854, 8.953103998512858652 ) ) ;
#46689 = FACE_OUTER_BOUND ( 'NONE', #2401, .T. ) ;
#46690 = CARTESIAN_POINT ( 'NONE',  ( 344.0000000000000000, 165.0000000000000000, -92.00000000000019895 ) ) ;
#46691 = ORIENTED_EDGE ( 'NONE', *, *, #24340, .T. ) ;
#46692 = ORIENTED_EDGE ( 'NONE', *, *, #25798, .T. ) ;
#46693 = CARTESIAN_POINT ( 'NONE',  ( -207.2473046169136808, -154.8119894309599260, 472.5992458228020610 ) ) ;
#46694 = CARTESIAN_POINT ( 'NONE',  ( -206.6959734468149463, -1.750000000000009992, -159.1817124430720298 ) ) ;
#46695 = CARTESIAN_POINT ( 'NONE',  ( -48.44597344681495343, 0.000000000000000000, 165.0000000000000000 ) ) ;
#46696 = VERTEX_POINT ( 'NONE', #10451 ) ;
#46697 = DIRECTION ( 'NONE',  ( 0.000000000000000000, -1.000000000000000000, 0.000000000000000000 ) ) ;
#46698 = FACE_OUTER_BOUND ( 'NONE', #27654, .T. ) ;
#46699 = CARTESIAN_POINT ( 'NONE',  ( 34.66007756064423972, -14.33302383662588930, -9.011255500499645521 ) ) ;
#46700 = FILL_AREA_STYLE ('',( #36227 ) ) ;
#46701 = VECTOR ( 'NONE', #1771, 1000.000000000000000 ) ;
#46702 = EDGE_LOOP ( 'NONE', ( #4463, #15474, #48460, #10501, #14082 ) ) ;
#46703 =( LENGTH_UNIT ( ) NAMED_UNIT ( * ) SI_UNIT ( .MILLI., .METRE. ) );
#46704 = ORIENTED_EDGE ( 'NONE', *, *, #45665, .T. ) ;
#46705 = CARTESIAN_POINT ( 'NONE',  ( 183.0000000000000000, -168.9999999999999432, -350.0000000000001705 ) ) ;
#46706 = DIRECTION ( 'NONE',  ( 0.000000000000000000, 0.9749645535258953943, -0.2223603367690637489 ) ) ;
#46707 = EDGE_LOOP ( 'NONE', ( #39429, #4367, #12697, #15091, #19450, #27853 ) ) ;
#46708 = ADVANCED_FACE ( 'NONE', ( #18391 ), #22500, .T. ) ;
#46709 = VECTOR ( 'NONE', #28112, 1000.000000000000000 ) ;
#46710 = PLANE ( 'NONE',  #27895 ) ;
#46711 = CARTESIAN_POINT ( 'NONE',  ( 25.60949810002064098, 43.19700938445193827, 1.847720168420772691 ) ) ;
#46712 = VECTOR ( 'NONE', #30317, 1000.000000000000000 ) ;
#46713 = CIRCLE ( 'NONE', #42639, 4.000000000000003553 ) ;
#46714 = CARTESIAN_POINT ( 'NONE',  ( 30.00000000000187228, 17.00000000000000000, 90.00000000000000000 ) ) ;
#46715 = ORIENTED_EDGE ( 'NONE', *, *, #489, .T. ) ;
#46716 = LINE ( 'NONE', #23147, #6462 ) ;
#46717 = CARTESIAN_POINT ( 'NONE',  ( 152.2789002873379900, 1.750000000000009548, -0.2068387089191121020 ) ) ;
#46718 = VERTEX_POINT ( 'NONE', #18140 ) ;
#46719 = DIRECTION ( 'NONE',  ( -4.625929269271584521E-16, 0.000000000000000000, -1.000000000000000000 ) ) ;
#46720 = DIRECTION ( 'NONE',  ( -0.000000000000000000, -1.000000000000000000, -0.000000000000000000 ) ) ;
#46721 = CARTESIAN_POINT ( 'NONE',  ( -114.9999999999997158, 17.00000000000000000, -60.00000000000000000 ) ) ;
#46722 = FACE_OUTER_BOUND ( 'NONE', #34162, .T. ) ;
#46723 = ORIENTED_EDGE ( 'NONE', *, *, #15141, .T. ) ;
#46724 = ORIENTED_EDGE ( 'NONE', *, *, #21238, .F. ) ;
#46725 = DIRECTION ( 'NONE',  ( 0.000000000000000000, 0.000000000000000000, 1.000000000000000000 ) ) ;
#46726 = LINE ( 'NONE', #7526, #24708 ) ;
#46727 = ORIENTED_EDGE ( 'NONE', *, *, #24747, .T. ) ;
#46728 = CARTESIAN_POINT ( 'NONE',  ( -204.9459734468149463, 2.143131898507880377E-16, 165.0000000000000000 ) ) ;
#46729 = LINE ( 'NONE', #46229, #13311 ) ;
#46730 = ORIENTED_EDGE ( 'NONE', *, *, #1764, .T. ) ;
#46731 = CARTESIAN_POINT ( 'NONE',  ( -0.03371980368972005843, -1.221991649883341413, 9.987567862361071747 ) ) ;
#46732 = ORIENTED_EDGE ( 'NONE', *, *, #16792, .T. ) ;
#46733 = DIRECTION ( 'NONE',  ( 1.000000000000000000, 0.000000000000000000, 0.000000000000000000 ) ) ;
#46734 = ADVANCED_FACE ( 'NONE', ( #29960 ), #33814, .T. ) ;
#46735 = CARTESIAN_POINT ( 'NONE',  ( -128.4459734468149179, 0.000000000000000000, -40.93171244307202983 ) ) ;
#46736 = CARTESIAN_POINT ( 'NONE',  ( 85.00000000000056843, 17.00000000000000000, -54.99999999999999289 ) ) ;
#46737 = VECTOR ( 'NONE', #5351, 1000.000000000000000 ) ;
#46738 = ORIENTED_EDGE ( 'NONE', *, *, #48845, .T. ) ;
#46739 = ORIENTED_EDGE ( 'NONE', *, *, #7664, .F. ) ;
#46740 = ORIENTED_EDGE ( 'NONE', *, *, #4887, .T. ) ;
#46741 = FACE_BOUND ( 'NONE', #29290, .T. ) ;
#46742 = CARTESIAN_POINT ( 'NONE',  ( -36.76598589393961447, -7.383243274241610088, -8.192531242611266862 ) ) ;
#46743 = CARTESIAN_POINT ( 'NONE',  ( 33.30402655318503946, -1.750000000000010658, -79.18171244307201562 ) ) ;
#46744 = EDGE_LOOP ( 'NONE', ( #9870, #37536, #20997, #47993 ) ) ;
#46745 = DIRECTION ( 'NONE',  ( 1.000000000000000000, 0.000000000000000000, -0.000000000000000000 ) ) ;
#46746 = AXIS2_PLACEMENT_3D ( 'NONE', #31178, #16030, #11927 ) ;
#46747 = ORIENTED_EDGE ( 'NONE', *, *, #25519, .F. ) ;
#46748 = CARTESIAN_POINT ( 'NONE',  ( 168.9999999999999716, -5.999999999999950262, -340.0000000000001137 ) ) ;
#46749 = ORIENTED_EDGE ( 'NONE', *, *, #22860, .F. ) ;
#46750 =( LENGTH_UNIT ( ) NAMED_UNIT ( * ) SI_UNIT ( .MILLI., .METRE. ) );
#46751 = DIRECTION ( 'NONE',  ( -1.000000000000000000, 0.000000000000000000, -7.793956916774525800E-48 ) ) ;
#46752 = CARTESIAN_POINT ( 'NONE',  ( -115.0000000000000284, 17.00000000000000000, -114.9999999999999858 ) ) ;
#46753 = FACE_OUTER_BOUND ( 'NONE', #19060, .T. ) ;
#46754 = CARTESIAN_POINT ( 'NONE',  ( 1.249999999999999778, 0.000000000000000000, 10.00000000000000000 ) ) ;
#46755 = ORIENTED_EDGE ( 'NONE', *, *, #30470, .T. ) ;
#46756 = ORIENTED_EDGE ( 'NONE', *, *, #48675, .F. ) ;
#46757 = DIRECTION ( 'NONE',  ( 0.000000000000000000, 0.000000000000000000, 1.000000000000000000 ) ) ;
#46758 = CARTESIAN_POINT ( 'NONE',  ( 191.5540265531850537, -1.025126265847089657, 42.56828755692799149 ) ) ;
#46759 = CARTESIAN_POINT ( 'NONE',  ( -0.3862712429686895876, 1.188820645368940720, -10.00000000000000000 ) ) ;
#46760 = CARTESIAN_POINT ( 'NONE',  ( 167.0000000000000000, -9.999999999999953815, -111.0000000000001563 ) ) ;
#46761 = CARTESIAN_POINT ( 'NONE',  ( 44.25629667545848633, 43.33333333333339255, 790.0000000000000000 ) ) ;
#46762 = VERTEX_POINT ( 'NONE', #14292 ) ;
#46763 = EDGE_CURVE ( 'NONE', #37083, #4452, #42203, .T. ) ;
#46764 = CARTESIAN_POINT ( 'NONE',  ( -164.9459734468149463, 2.143131898507880377E-16, -0.9317124430720247208 ) ) ;
#46765 = DIRECTION ( 'NONE',  ( 0.000000000000000000, -1.000000000000000000, 0.000000000000000000 ) ) ;
#46766 = ADVANCED_FACE ( 'NONE', ( #42256, #42004 ), #46327, .T. ) ;
#46767 = VECTOR ( 'NONE', #4703, 1000.000000000000000 ) ;
#46768 = EDGE_LOOP ( 'NONE', ( #50569, #4614, #24829, #6197, #46666, #40519, #39110, #7786 ) ) ;
#46769 = CYLINDRICAL_SURFACE ( 'NONE', #17227, 1.750000000000001554 ) ;
#46770 = CARTESIAN_POINT ( 'NONE',  ( 154.3291528190321458, -1.750000000000009548, 121.8434138227750623 ) ) ;
#46771 = PLANE ( 'NONE',  #29903 ) ;
#46772 = AXIS2_PLACEMENT_3D ( 'NONE', #11717, #50149, #34836 ) ;
#46773 = EDGE_CURVE ( 'NONE', #21399, #46031, #25668, .T. ) ;
#46774 = ADVANCED_FACE ( 'NONE', ( #26861 ), #42499, .T. ) ;
#46775 = ORIENTED_EDGE ( 'NONE', *, *, #44313, .T. ) ;
#46776 = AXIS2_PLACEMENT_3D ( 'NONE', #33455, #13919, #29587 ) ;
#46777 = VERTEX_POINT ( 'NONE', #25512 ) ;
#46778 = FACE_OUTER_BOUND ( 'NONE', #49099, .T. ) ;
#46779 = CARTESIAN_POINT ( 'NONE',  ( -1.066995270233474624, 50.00000000000000711, -3.760136334089591248 ) ) ;
#46780 = ADVANCED_FACE ( 'NONE', ( #41667 ), #2411, .T. ) ;
#46781 = ORIENTED_EDGE ( 'NONE', *, *, #32509, .F. ) ;
#46782 = VERTEX_POINT ( 'NONE', #48566 ) ;
#46783 = CARTESIAN_POINT ( 'NONE',  ( 357.9999999999999432, -180.9999999999999716, 355.9999999999998295 ) ) ;
#46784 = CARTESIAN_POINT ( 'NONE',  ( -7.576114424932982594, 50.00000000000000711, 7.906207997025717304 ) ) ;
#46785 = CARTESIAN_POINT ( 'NONE',  ( -8.277096487746778308, 33.14818118907697198, 7.455576670931136185 ) ) ;
#46786 = DIRECTION ( 'NONE',  ( 0.000000000000000000, 0.000000000000000000, -1.000000000000000000 ) ) ;
#46787 = EDGE_LOOP ( 'NONE', ( #27502, #4701, #20066, #15786, #22299 ) ) ;
#46788 = ORIENTED_EDGE ( 'NONE', *, *, #7072, .T. ) ;
#46789 = ORIENTED_EDGE ( 'NONE', *, *, #38254, .T. ) ;
#46790 = EDGE_CURVE ( 'NONE', #32189, #19150, #21921, .T. ) ;
#46791 = EDGE_CURVE ( 'NONE', #41868, #31669, #6511, .T. ) ;
#46792 = CARTESIAN_POINT ( 'NONE',  ( 192.2789002873380184, -1.750000000000009548, -38.15658617722494483 ) ) ;
#46793 = CARTESIAN_POINT ( 'NONE',  ( -33.89193117067290473, -21.24469349090191983, 910.0000000000000000 ) ) ;
#46794 =( BOUNDED_CURVE ( )  B_SPLINE_CURVE ( 3, ( #19816, #4428, #35495, #50307 ),
 .UNSPECIFIED., .F., .F. ) 
 B_SPLINE_CURVE_WITH_KNOTS ( ( 4, 4 ),
 ( 0.000000000000000000, 1.570796326794896558 ),
 .UNSPECIFIED. ) 
 CURVE ( )  GEOMETRIC_REPRESENTATION_ITEM ( )  RATIONAL_B_SPLINE_CURVE ( ( 1.000000000000000000, 0.8047378541243649375, 0.8047378541243649375, 1.000000000000000000 ) ) 
 REPRESENTATION_ITEM ( '' )  );
#46795 = ADVANCED_FACE ( 'NONE', ( #22168, #37589 ), #45227, .T. ) ;
#46796 = EDGE_LOOP ( 'NONE', ( #45872, #20777, #959, #31732 ) ) ;
#46797 = EDGE_CURVE ( 'NONE', #50400, #21827, #9858, .T. ) ;
#46798 = CARTESIAN_POINT ( 'NONE',  ( 1.170973275723889095, 0.8656725377797501730, 9.938543673150057600 ) ) ;
#46799 = DIRECTION ( 'NONE',  ( 1.000000000000000000, 0.000000000000000000, 0.000000000000000000 ) ) ;
#46800 = CARTESIAN_POINT ( 'NONE',  ( -1.184758822850544568, 0.8459872530594374496, 9.938560165450795125 ) ) ;
#46801 = VERTEX_POINT ( 'NONE', #1668 ) ;
#46802 = ORIENTED_EDGE ( 'NONE', *, *, #11109, .T. ) ;
#46803 = LINE ( 'NONE', #47058, #23793 ) ;
#46805 = CARTESIAN_POINT ( 'NONE',  ( 1.780619886013945052, 1.041246721325614466, 9.886433018048068178 ) ) ;
#46804 =( BOUNDED_CURVE ( )  B_SPLINE_CURVE ( 3, ( #21227, #36915, #4576, #47628 ),
 .UNSPECIFIED., .F., .F. ) 
 B_SPLINE_CURVE_WITH_KNOTS ( ( 4, 4 ),
 ( 3.141592653589793116, 4.712388980384689674 ),
 .UNSPECIFIED. ) 
 CURVE ( )  GEOMETRIC_REPRESENTATION_ITEM ( )  RATIONAL_B_SPLINE_CURVE ( ( 1.000000000000000000, 0.8047378541243649375, 0.8047378541243649375, 1.000000000000000000 ) ) 
 REPRESENTATION_ITEM ( '' )  );
#46806 = VECTOR ( 'NONE', #36995, 1000.000000000000000 ) ;
#46807 = ADVANCED_FACE ( 'NONE', ( #49066 ), #2657, .T. ) ;
#46808 = LINE ( 'NONE', #15553, #27345 ) ;
#46809 = ORIENTED_EDGE ( 'NONE', *, *, #44153, .F. ) ;
#46810 = ORIENTED_EDGE ( 'NONE', *, *, #11158, .F. ) ;
#46811 = CARTESIAN_POINT ( 'NONE',  ( 73.30402655318508209, 1.750000000000009992, -159.1817124430720298 ) ) ;
#46812 = EDGE_LOOP ( 'NONE', ( #26224, #16364, #49731, #27407, #38584, #20423 ) ) ;
#46813 = CARTESIAN_POINT ( 'NONE',  ( 0.000000000000000000, -317.3964497041420145, 132.2485207100591253 ) ) ;
#46814 = PLANE ( 'NONE',  #1457 ) ;
#46815 = FACE_OUTER_BOUND ( 'NONE', #49966, .T. ) ;
#46816 = CARTESIAN_POINT ( 'NONE',  ( -86.69597344681494633, -1.750000000000010658, 120.8182875569279702 ) ) ;
#46817 = ORIENTED_EDGE ( 'NONE', *, *, #7062, .F. ) ;
#46818 = CARTESIAN_POINT ( 'NONE',  ( 168.9999999999999716, -164.9999999999999432, -115.0000000000001847 ) ) ;
#46819 = DIRECTION ( 'NONE',  ( -1.000000000000000000, -0.000000000000000000, -0.000000000000000000 ) ) ;
#46820 =( BOUNDED_CURVE ( )  B_SPLINE_CURVE ( 3, ( #3539, #24082, #35647, #27166 ),
 .UNSPECIFIED., .F., .F. ) 
 B_SPLINE_CURVE_WITH_KNOTS ( ( 4, 4 ),
 ( 3.141592653589793116, 4.712388980384689674 ),
 .UNSPECIFIED. ) 
 CURVE ( )  GEOMETRIC_REPRESENTATION_ITEM ( )  RATIONAL_B_SPLINE_CURVE ( ( 1.000000000000000000, 0.8047378541243649375, 0.8047378541243649375, 1.000000000000000000 ) ) 
 REPRESENTATION_ITEM ( '' )  );
#46821 = CARTESIAN_POINT ( 'NONE',  ( 111.5540265531850679, 0.000000000000000000, 119.0682875569279844 ) ) ;
#46822 = ADVANCED_FACE ( 'NONE', ( #32715, #14201 ), #5506, .F. ) ;
#46823 = CARTESIAN_POINT ( 'NONE',  ( 16.16402646813543242, -4.033894069732437693, -3.546734833711462365 ) ) ;
#46824 = EDGE_CURVE ( 'NONE', #13712, #11195, #21658, .T. ) ;
#46825 = B_SPLINE_CURVE_WITH_KNOTS ( 'NONE', 3,
 ( #29990, #15850, #43033, #23030 ),
 .UNSPECIFIED., .F., .F.,
 ( 4, 4 ),
 ( 8.824766327896537836E-19, 0.002040833422559265500 ),
 .UNSPECIFIED. ) ;
#46826 = EDGE_CURVE ( 'NONE', #9263, #12877, #13456, .T. ) ;
#46827 = ORIENTED_EDGE ( 'NONE', *, *, #49247, .T. ) ;
#46828 = CARTESIAN_POINT ( 'NONE',  ( 232.4999999999999716, -169.9999999999999716, 474.9999999999998863 ) ) ;
#46829 = ADVANCED_FACE ( 'NONE', ( #26026 ), #37348, .F. ) ;
#46830 = CARTESIAN_POINT ( 'NONE',  ( 181.0000000000000000, -95.49999999999998579, -340.0000000000001137 ) ) ;
#46831 = CARTESIAN_POINT ( 'NONE',  ( -164.4973046169135955, -97.72914955339486198, -17.31629813440246579 ) ) ;
#46832 = ADVANCED_FACE ( 'NONE', ( #10375 ), #13202, .F. ) ;
#46833 = VERTEX_POINT ( 'NONE', #44483 ) ;
#46834 = DIRECTION ( 'NONE',  ( 0.000000000000000000, 0.000000000000000000, -1.000000000000000000 ) ) ;
#46835 = CARTESIAN_POINT ( 'NONE',  ( 71.55402655318505367, 0.000000000000000000, -0.9317124430720524764 ) ) ;
#46836 = ORIENTED_EDGE ( 'NONE', *, *, #8255, .F. ) ;
#46837 = LINE ( 'NONE', #8397, #11452 ) ;
#46838 = CARTESIAN_POINT ( 'NONE',  ( 183.0000000000000000, 175.0000000000000284, -344.0000000000001137 ) ) ;
#46839 = CARTESIAN_POINT ( 'NONE',  ( 210.0000000000000568, 0.000000000000000000, 80.81828755692798438 ) ) ;
#46840 = CARTESIAN_POINT ( 'NONE',  ( 166.9999999999999716, -164.9999999999999432, -356.0000000000001705 ) ) ;
#46841 = AXIS2_PLACEMENT_3D ( 'NONE', #29054, #41358, #16999 ) ;
#46842 = ORIENTED_EDGE ( 'NONE', *, *, #1700, .F. ) ;
#46843 = CARTESIAN_POINT ( 'NONE',  ( -166.6959734468149463, -1.750000000000010658, -119.1817124430720440 ) ) ;
#46844 = ORIENTED_EDGE ( 'NONE', *, *, #49025, .T. ) ;
#46845 = ORIENTED_EDGE ( 'NONE', *, *, #6379, .T. ) ;
#46846 = DIRECTION ( 'NONE',  ( -0.000000000000000000, -1.000000000000000000, -0.000000000000000000 ) ) ;
#46847 = EDGE_CURVE ( 'NONE', #4637, #40403, #22054, .T. ) ;
#46848 = ORIENTED_EDGE ( 'NONE', *, *, #13316, .F. ) ;
#46849 = AXIS2_PLACEMENT_3D ( 'NONE', #540, #31838, #12824 ) ;
#46850 = CARTESIAN_POINT ( 'NONE',  ( -15.00000000000000000, 12.98684210526315930, 19.37312575500900280 ) ) ;
#46851 = CARTESIAN_POINT ( 'NONE',  ( -126.6959734468149321, 0.000000000000000000, 165.0000000000000000 ) ) ;
#46852 = EDGE_CURVE ( 'NONE', #49565, #49290, #11597, .T. ) ;
#46853 = CARTESIAN_POINT ( 'NONE',  ( -64.99999999999815259, 17.00000000000000000, 65.00000000000000000 ) ) ;
#46854 = ORIENTED_EDGE ( 'NONE', *, *, #38876, .T. ) ;
#46855 = CARTESIAN_POINT ( 'NONE',  ( 72.27890028733797578, 1.750000000000009548, 121.8434138227750623 ) ) ;
#46856 = CARTESIAN_POINT ( 'NONE',  ( -165.0000000000000284, 16.00000000000000000, 95.00000000000000000 ) ) ;
#46857 = EDGE_CURVE ( 'NONE', #45963, #38992, #25018, .T. ) ;
#46858 = ORIENTED_EDGE ( 'NONE', *, *, #27218, .T. ) ;
#46859 = EDGE_CURVE ( 'NONE', #34025, #28991, #4436, .T. ) ;
#46860 = CARTESIAN_POINT ( 'NONE',  ( 0.3370904143228924954, 0.2449105217885333141, 10.00000000000000000 ) ) ;
#46861 = DIRECTION ( 'NONE',  ( 0.000000000000000000, 1.000000000000000000, 0.000000000000000000 ) ) ;
#46862 = ORIENTED_EDGE ( 'NONE', *, *, #34991, .F. ) ;
#46863 = VERTEX_POINT ( 'NONE', #11096 ) ;
#46864 = ORIENTED_EDGE ( 'NONE', *, *, #6052, .F. ) ;
#46865 = CARTESIAN_POINT ( 'NONE',  ( -119.9999999999997158, 16.00000000000000000, -84.99999999999998579 ) ) ;
#46866 = ADVANCED_FACE ( 'NONE', ( #50549 ), #42637, .T. ) ;
#46867 = ADVANCED_FACE ( 'NONE', ( #38319 ), #15206, .F. ) ;
#46868 = DIRECTION ( 'NONE',  ( 0.000000000000000000, 0.000000000000000000, 1.000000000000000000 ) ) ;
#46869 = ORIENTED_EDGE ( 'NONE', *, *, #21630, .F. ) ;
#46870 = EDGE_CURVE ( 'NONE', #14588, #34800, #26000, .T. ) ;
#46871 = CARTESIAN_POINT ( 'NONE',  ( 154.1026953830863420, -97.66198943095992036, 23.74256005001722158 ) ) ;
#46872 = CARTESIAN_POINT ( 'NONE',  ( -48.98697415750977058, -11.03699497439218291, -8.016098858316205167 ) ) ;
#46873 = FACE_OUTER_BOUND ( 'NONE', #17273, .T. ) ;
#46874 = PLANE ( 'NONE',  #44340 ) ;
#46875 = CARTESIAN_POINT ( 'NONE',  ( 152.2789002873379900, -1.750000000000010214, 81.84341382277507648 ) ) ;
#46876 = PRESENTATION_LAYER_ASSIGNMENT (  '', '', ( #35443 ) ) ;
#46877 = DIRECTION ( 'NONE',  ( -1.000000000000000000, -0.000000000000000000, -0.000000000000000000 ) ) ;
#46878 =( NAMED_UNIT ( * ) PLANE_ANGLE_UNIT ( ) SI_UNIT ( $, .RADIAN. ) );
#46879 = VECTOR ( 'NONE', #35204, 1000.000000000000000 ) ;
#46880 = FACE_OUTER_BOUND ( 'NONE', #28538, .T. ) ;
#46881 = CARTESIAN_POINT ( 'NONE',  ( 31.55402655318503236, 0.000000000000000000, -120.9317124430720725 ) ) ;
#46882 = COLOUR_RGB ( '',0.7921568627450980005, 0.8196078431372548767, 0.9333333333333333481 ) ;
#46883 = VERTEX_POINT ( 'NONE', #49538 ) ;
#46884 = CARTESIAN_POINT ( 'NONE',  ( -167.4999999999999716, 102.9547873477646647, -7.018571579996165433 ) ) ;
#46885 = DIRECTION ( 'NONE',  ( 0.000000000000000000, -2.265761274745217480E-16, 1.000000000000000000 ) ) ;
#46886 = EDGE_CURVE ( 'NONE', #1823, #42650, #40944, .T. ) ;
#46887 = VECTOR ( 'NONE', #25221, 1000.000000000000000 ) ;
#46888 = DIRECTION ( 'NONE',  ( 1.000000000000000000, 0.000000000000000000, 0.000000000000000000 ) ) ;
#46889 = CARTESIAN_POINT ( 'NONE',  ( -34.08406891383351933, 15.63733501198486309, -8.192531242611266862 ) ) ;
#46890 = ORIENTED_EDGE ( 'NONE', *, *, #40902, .F. ) ;
#46891 = DIRECTION ( 'NONE',  ( 1.000000000000000000, 0.000000000000000000, -1.586032892321652482E-16 ) ) ;
#46892 = LINE ( 'NONE', #4599, #30224 ) ;
#46893 = CARTESIAN_POINT ( 'NONE',  ( -86.69597344681494633, 1.750000000000009992, 0.8182875569279768335 ) ) ;
#46894 = CARTESIAN_POINT ( 'NONE',  ( -16.52264463346130796, 2.779753662172870232, 9.403735324607438884 ) ) ;
#46895 = VERTEX_POINT ( 'NONE', #50295 ) ;
#46896 = DIRECTION ( 'NONE',  ( -4.758098676964957447E-16, -1.000000000000000000, 7.143884938411937192E-48 ) ) ;
#46897 = EDGE_LOOP ( 'NONE', ( #49736, #1708, #24374 ) ) ;
#46898 = CARTESIAN_POINT ( 'NONE',  ( 14.49999999999999822, -46.01315789473684248, -5.916985404131817283 ) ) ;
#46899 =( BOUNDED_CURVE ( )  B_SPLINE_CURVE ( 3, ( #11714, #27367, #43002, #7882 ),
 .UNSPECIFIED., .F., .F. ) 
 B_SPLINE_CURVE_WITH_KNOTS ( ( 4, 4 ),
 ( 3.141592653589793116, 4.712388980384689674 ),
 .UNSPECIFIED. ) 
 CURVE ( )  GEOMETRIC_REPRESENTATION_ITEM ( )  RATIONAL_B_SPLINE_CURVE ( ( 1.000000000000000000, 0.8047378541243649375, 0.8047378541243649375, 1.000000000000000000 ) ) 
 REPRESENTATION_ITEM ( '' )  );
#46900 = EDGE_LOOP ( 'NONE', ( #15147, #28981 ) ) ;
#46901 = CARTESIAN_POINT ( 'NONE',  ( 210.0000000000000568, 2.143131898507881116E-16, 39.06828755692797728 ) ) ;
#46903 = EDGE_CURVE ( 'NONE', #14416, #11052, #30349, .T. ) ;
#46902 = CARTESIAN_POINT ( 'NONE',  ( 194.3291528190321742, 1.750000000000010214, 121.8434138227750623 ) ) ;
#46904 = VERTEX_POINT ( 'NONE', #49786 ) ;
#46905 = LINE ( 'NONE', #38002, #43686 ) ;
#46906 = ORIENTED_EDGE ( 'NONE', *, *, #41357, .F. ) ;
#46907 = EDGE_LOOP ( 'NONE', ( #25187, #26384, #10791, #18716 ) ) ;
#46908 = CARTESIAN_POINT ( 'NONE',  ( 71.55402655318505367, -1.025126265847089213, 162.5682875569279133 ) ) ;
#46909 = DIRECTION ( 'NONE',  ( -0.000000000000000000, -1.000000000000000000, -0.000000000000000000 ) ) ;
#46910 = ORIENTED_EDGE ( 'NONE', *, *, #46650, .F. ) ;
#46911 = CARTESIAN_POINT ( 'NONE',  ( -86.69597344681494633, 1.750000000000010658, 120.8182875569279702 ) ) ;
#46912 = DIRECTION ( 'NONE',  ( -1.000000000000000000, 0.000000000000000000, -0.000000000000000000 ) ) ;
#46913 = CIRCLE ( 'NONE', #45273, 2.000000000000001776 ) ;
#46914 = CARTESIAN_POINT ( 'NONE',  ( 192.2789002873380184, 1.750000000000009548, 161.8434138227750907 ) ) ;
#46915 = ORIENTED_EDGE ( 'NONE', *, *, #9906, .F. ) ;
#46916 = LINE ( 'NONE', #7976, #44735 ) ;
#46917 = AXIS2_PLACEMENT_3D ( 'NONE', #17593, #33268, #21190 ) ;
#46918 = DIRECTION ( 'NONE',  ( 6.203854594147707562E-25, -2.067951531382569187E-25, 1.000000000000000000 ) ) ;
#46919 = EDGE_CURVE ( 'NONE', #24059, #572, #30866, .T. ) ;
#46920 = VERTEX_POINT ( 'NONE', #19034 ) ;
#46921 = EDGE_CURVE ( 'NONE', #28202, #16567, #42384, .T. ) ;
#46922 = CARTESIAN_POINT ( 'NONE',  ( -1.035950918207909632, -33.23661552194049307, -2.408242355805840784 ) ) ;
#46923 = VERTEX_POINT ( 'NONE', #37813 ) ;
#46924 = CARTESIAN_POINT ( 'NONE',  ( 191.5540265531851105, 0.000000000000000000, -0.9317124430720247208 ) ) ;
#46925 = EDGE_CURVE ( 'NONE', #9554, #31779, #3129, .T. ) ;
#46926 = EDGE_CURVE ( 'NONE', #37586, #38893, #14440, .T. ) ;
#46927 = CARTESIAN_POINT ( 'NONE',  ( 168.9999999999999716, -272.4999999999999432, -349.9999999999999432 ) ) ;
#46928 = B_SPLINE_SURFACE_WITH_KNOTS ( 'NONE', 3, 3, ( 
 ( #39728, #4564, #20213, #4799 ),
 ( #712, #16362, #43802, #27157 ),
 ( #23291, #35131, #50709, #46860 ),
 ( #11757, #7923, #23561, #219 ) ),
 .UNSPECIFIED., .F., .F., .F.,
 ( 4, 4 ),
 ( 4, 4 ),
 ( 0.000000000000000000, 1.000000000000000000 ),
 ( 0.000000000000000000, 1.000000000000000000 ),
 .UNSPECIFIED. ) ;
#46929 = ORIENTED_EDGE ( 'NONE', *, *, #1451, .F. ) ;
#46930 = CARTESIAN_POINT ( 'NONE',  ( -14.99999999999937472, 16.00000000000000000, -54.99999999999999289 ) ) ;
#46931 = EDGE_CURVE ( 'NONE', #29536, #43849, #18776, .T. ) ;
#46932 = CARTESIAN_POINT ( 'NONE',  ( 80.00000000000092371, 17.00000000000000000, -24.99999999999999289 ) ) ;
#46933 = CARTESIAN_POINT ( 'NONE',  ( 359.9999999999999432, -178.0000000000000000, 352.9999999999998295 ) ) ;
#46934 = EDGE_CURVE ( 'NONE', #17054, #34874, #50037, .T. ) ;
#46935 = DIRECTION ( 'NONE',  ( 1.333906992743555050E-23, -1.000000000000000000, 0.000000000000000000 ) ) ;
#46936 = VERTEX_POINT ( 'NONE', #10581 ) ;
#46937 = CARTESIAN_POINT ( 'NONE',  ( -23.82716369509181575, -44.49195112875988656, 8.356839323120299312 ) ) ;
#46938 = CARTESIAN_POINT ( 'NONE',  ( -2.052581215100349521, 0.2042358160481012597, 9.886433018048073507 ) ) ;
#46939 = EDGE_CURVE ( 'NONE', #25458, #19871, #27316, .T. ) ;
#46940 = CARTESIAN_POINT ( 'NONE',  ( -1.011271242968683426, -0.7347315653655928092, 10.00000000000000000 ) ) ;
#46941 = ORIENTED_EDGE ( 'NONE', *, *, #10867, .T. ) ;
#46942 = ORIENTED_EDGE ( 'NONE', *, *, #48078, .T. ) ;
#46943 = DIRECTION ( 'NONE',  ( -1.741512270944222404E-14, -1.772375685609419313E-17, -1.000000000000000000 ) ) ;
#46944 = CARTESIAN_POINT ( 'NONE',  ( 111.5540265531850679, 0.000000000000000000, -80.93171244307201562 ) ) ;
#46945 = CARTESIAN_POINT ( 'NONE',  ( 35.05402655318504657, 2.143131898507880377E-16, -117.4317124430720156 ) ) ;
#46946 = FILL_AREA_STYLE_COLOUR ( '', #6183 ) ;
#46947 = CIRCLE ( 'NONE', #21600, 1.749999999999987566 ) ;
#46948 = DIRECTION ( 'NONE',  ( -1.000000000000000000, -0.000000000000000000, -0.000000000000000000 ) ) ;
#46949 = DIRECTION ( 'NONE',  ( 0.000000000000000000, -2.969158215481698263E-48, 1.000000000000000000 ) ) ;
#46950 = EDGE_LOOP ( 'NONE', ( #18624, #32159, #20593, #38346, #26463, #34037 ) ) ;
#46951 = FACE_OUTER_BOUND ( 'NONE', #9968, .T. ) ;
#46952 = VECTOR ( 'NONE', #46819, 1000.000000000000000 ) ;
#46953 = DIRECTION ( 'NONE',  ( -1.000000000000000000, 0.000000000000000000, 0.000000000000000000 ) ) ;
#46954 = DIRECTION ( 'NONE',  ( 0.7233555441435720601, 0.6904757466825006684, -0.000000000000000000 ) ) ;
#46955 = VECTOR ( 'NONE', #5162, 1000.000000000000000 ) ;
#46956 =( BOUNDED_CURVE ( )  B_SPLINE_CURVE ( 3, ( #33437, #49011, #21879, #37543 ),
 .UNSPECIFIED., .F., .F. ) 
 B_SPLINE_CURVE_WITH_KNOTS ( ( 4, 4 ),
 ( 4.712388980384689674, 6.283185307179586232 ),
 .UNSPECIFIED. ) 
 CURVE ( )  GEOMETRIC_REPRESENTATION_ITEM ( )  RATIONAL_B_SPLINE_CURVE ( ( 1.000000000000000000, 0.8047378541243649375, 0.8047378541243649375, 1.000000000000000000 ) ) 
 REPRESENTATION_ITEM ( '' )  );
#46957 = ORIENTED_EDGE ( 'NONE', *, *, #33362, .T. ) ;
#46958 = CARTESIAN_POINT ( 'NONE',  ( 152.2789002873379900, 1.750000000000009548, -40.20683870891912193 ) ) ;
#46959 = VERTEX_POINT ( 'NONE', #46204 ) ;
#46960=STYLED_ITEM('',(#50747),#38306);
#46961 = FACE_OUTER_BOUND ( 'NONE', #41536, .T. ) ;
#46962 = ORIENTED_EDGE ( 'NONE', *, *, #23529, .T. ) ;
#46963 = DIRECTION ( 'NONE',  ( 0.000000000000000000, -1.000000000000000000, 0.000000000000000000 ) ) ;
#46964 = DIRECTION ( 'NONE',  ( 1.000000000000000000, 0.000000000000000000, 0.000000000000000000 ) ) ;
#46965 =( BOUNDED_CURVE ( )  B_SPLINE_CURVE ( 3, ( #48680, #44593, #5878, #25141 ),
 .UNSPECIFIED., .F., .F. ) 
 B_SPLINE_CURVE_WITH_KNOTS ( ( 4, 4 ),
 ( 1.570796326794896558, 3.141592653589793116 ),
 .UNSPECIFIED. ) 
 CURVE ( )  GEOMETRIC_REPRESENTATION_ITEM ( )  RATIONAL_B_SPLINE_CURVE ( ( 1.000000000000000000, 0.8047378541243649375, 0.8047378541243649375, 1.000000000000000000 ) ) 
 REPRESENTATION_ITEM ( '' )  );
#46966 =( LENGTH_UNIT ( ) NAMED_UNIT ( * ) SI_UNIT ( .MILLI., .METRE. ) );
#46967 = CARTESIAN_POINT ( 'NONE',  ( -4.945973446814903696, 2.143131898507912917E-16, 122.5682875569279986 ) ) ;
#46968 = VERTEX_POINT ( 'NONE', #7248 ) ;
#46969 = EDGE_CURVE ( 'NONE', #35861, #47433, #33948, .T. ) ;
#46970 = VECTOR ( 'NONE', #17313, 1000.000000000000000 ) ;
#46971 = DIRECTION ( 'NONE',  ( 1.000000000000000000, 0.000000000000000000, 0.000000000000000000 ) ) ;
#46972 = CARTESIAN_POINT ( 'NONE',  ( 168.9999999999999716, -164.9999999999999432, 355.9999999999998863 ) ) ;
#46973 = EDGE_LOOP ( 'NONE', ( #13256, #4945, #2722, #45031, #26753, #28815 ) ) ;
#46974 = CARTESIAN_POINT ( 'NONE',  ( 3.808200756227633654, 0.8261963378076531139, 9.741991644047248045 ) ) ;
#46975 = DIRECTION ( 'NONE',  ( 0.000000000000000000, -0.000000000000000000, -1.000000000000000000 ) ) ;
#46976 = CARTESIAN_POINT ( 'NONE',  ( 33.30402655318503946, 1.750000000000010658, 80.81828755692798438 ) ) ;
#46977 = DIRECTION ( 'NONE',  ( 0.000000000000000000, 0.000000000000000000, 1.000000000000000000 ) ) ;
#46978 = ORIENTED_EDGE ( 'NONE', *, *, #46595, .F. ) ;
#46979 = VERTEX_POINT ( 'NONE', #41890 ) ;
#46980 = DIRECTION ( 'NONE',  ( 0.000000000000000000, 0.000000000000000000, -1.000000000000000000 ) ) ;
#46981 = ORIENTED_EDGE ( 'NONE', *, *, #4220, .F. ) ;
#46982 = EDGE_CURVE ( 'NONE', #37466, #18505, #3382, .T. ) ;
#46983 = FACE_BOUND ( 'NONE', #6582, .T. ) ;
#46984 = VECTOR ( 'NONE', #6436, 1000.000000000000000 ) ;
#46985 = DIRECTION ( 'NONE',  ( 0.000000000000000000, 0.000000000000000000, 1.000000000000000000 ) ) ;
#46986 = ORIENTED_EDGE ( 'NONE', *, *, #45940, .T. ) ;
#46987 = FACE_OUTER_BOUND ( 'NONE', #41604, .T. ) ;
#46988 = VECTOR ( 'NONE', #28453, 1000.000000000000000 ) ;
#46989 = ORIENTED_EDGE ( 'NONE', *, *, #39942, .F. ) ;
#46990 = CARTESIAN_POINT ( 'NONE',  ( 0.3862712429686894766, -1.188820645368940276, -3.333333333333333481 ) ) ;
#46991 = AXIS2_PLACEMENT_3D ( 'NONE', #5036, #45022, #24807 ) ;
#46992 = LINE ( 'NONE', #44177, #49633 ) ;
#46993 = EDGE_CURVE ( 'NONE', #16851, #50400, #33132, .T. ) ;
#46994 = AXIS2_PLACEMENT_3D ( 'NONE', #8447, #40004, #36677 ) ;
#46995 = EDGE_CURVE ( 'NONE', #47971, #35326, #12353, .T. ) ;
#46996 = CARTESIAN_POINT ( 'NONE',  ( -582.5000000000000000, 57.49999999999996447, -58.60000000000003695 ) ) ;
#46997 = VERTEX_POINT ( 'NONE', #31374 ) ;
#46998 = ORIENTED_EDGE ( 'NONE', *, *, #4226, .F. ) ;
#46999 = ORIENTED_EDGE ( 'NONE', *, *, #3769, .T. ) ;
#47000 = CARTESIAN_POINT ( 'NONE',  ( 14.49999999999999822, 13.48684210526315930, 19.37312575500900280 ) ) ;
#47001 = EDGE_CURVE ( 'NONE', #46611, #10420, #18454, .T. ) ;
#47002 = SURFACE_SIDE_STYLE ('',( #4941 ) ) ;
#47003 = CARTESIAN_POINT ( 'NONE',  ( -165.6708471809677974, 1.750000000000009548, -40.20683870891912193 ) ) ;
#47004 = ORIENTED_EDGE ( 'NONE', *, *, #5259, .F. ) ;
#47005 = LINE ( 'NONE', #106, #47678 ) ;
#47006 = EDGE_LOOP ( 'NONE', ( #10165, #44326 ) ) ;
#47007 = DIRECTION ( 'NONE',  ( 0.000000000000000000, -1.000000000000000000, 1.604368532695312981E-16 ) ) ;
#47008 = ORIENTED_EDGE ( 'NONE', *, *, #9273, .T. ) ;
#47009 = CARTESIAN_POINT ( 'NONE',  ( 3.627208138665139803, 0.000000000000000000, 0.000000000000000000 ) ) ;
#47010 = DIRECTION ( 'NONE',  ( -0.000000000000000000, -0.000000000000000000, -1.000000000000000000 ) ) ;
#47011 = CIRCLE ( 'NONE', #19156, 1.750000000000015543 ) ;
#47012 = CARTESIAN_POINT ( 'NONE',  ( 1.066995270233474624, -33.23888904628638841, -3.760136334089591248 ) ) ;
#47013 = CARTESIAN_POINT ( 'NONE',  ( 4.672045878990125800, -33.19353511768168374, 1.847720168420772691 ) ) ;
#47014 = ORIENTED_EDGE ( 'NONE', *, *, #1159, .F. ) ;
#47015 = EDGE_LOOP ( 'NONE', ( #33428, #23015, #45037, #41959 ) ) ;
#47016 = DIRECTION ( 'NONE',  ( -1.000000000000000000, 0.000000000000000000, 0.000000000000000000 ) ) ;
#47017 = CARTESIAN_POINT ( 'NONE',  ( 5.551115123125782702E-14, -168.9999999999999432, 341.9999999999997726 ) ) ;
#47018 = CARTESIAN_POINT ( 'NONE',  ( 115.0540265531850395, -1.025126265847081664, 42.56828755692797017 ) ) ;
#47019 = CARTESIAN_POINT ( 'NONE',  ( -8.445973446814976526, 0.000000000000000000, -165.0000000000000000 ) ) ;
#47020 = B_SPLINE_CURVE_WITH_KNOTS ( 'NONE', 3,
 ( #23800, #16600, #32260, #12748 ),
 .UNSPECIFIED., .F., .F.,
 ( 4, 4 ),
 ( 0.000000000000000000, 0.001246897409371907316 ),
 .UNSPECIFIED. ) ;
#47021 = VECTOR ( 'NONE', #25252, 1000.000000000000000 ) ;
#47022 = CARTESIAN_POINT ( 'NONE',  ( 195.0540265531851105, -1.025126265847089657, 79.06828755692797017 ) ) ;
#47023 = ORIENTED_EDGE ( 'NONE', *, *, #37870, .F. ) ;
#47024 = VECTOR ( 'NONE', #48224, 1000.000000000000000 ) ;
#47025 = CARTESIAN_POINT ( 'NONE',  ( -165.3973046169136012, 54.43801056904003133, -94.69675437945474528 ) ) ;
#47026 = CARTESIAN_POINT ( 'NONE',  ( -164.9459734468149463, 2.143131898507880377E-16, -157.4317124430720582 ) ) ;
#47027 = CIRCLE ( 'NONE', #29050, 4.000000000000003553 ) ;
#47028 = EDGE_CURVE ( 'NONE', #19710, #13422, #20033, .T. ) ;
#47029 = VERTEX_POINT ( 'NONE', #11611 ) ;
#47030 = CARTESIAN_POINT ( 'NONE',  ( 210.0000000000000568, 2.143131898507876926E-16, 119.0682875569279560 ) ) ;
#47031 = B_SPLINE_CURVE_WITH_KNOTS ( 'NONE', 3,
 ( #37791, #14420, #30085, #29824 ),
 .UNSPECIFIED., .F., .F.,
 ( 4, 4 ),
 ( 4.818759382071585759E-16, 0.009782300387714815831 ),
 .UNSPECIFIED. ) ;
#47032 = CARTESIAN_POINT ( 'NONE',  ( -18.67411147745623978, -27.51799019669813973, -3.760136334089591248 ) ) ;
#47033 = DIRECTION ( 'NONE',  ( -1.000000000000000000, -0.000000000000000000, -0.000000000000000000 ) ) ;
#47034 = ORIENTED_EDGE ( 'NONE', *, *, #34476, .F. ) ;
#47035 = ORIENTED_EDGE ( 'NONE', *, *, #30806, .T. ) ;
#47036 = CARTESIAN_POINT ( 'NONE',  ( 194.3291528190321742, -1.750000000000009548, -78.15658617722490931 ) ) ;
#47037 = DIRECTION ( 'NONE',  ( -0.000000000000000000, -0.000000000000000000, -1.000000000000000000 ) ) ;
#47038 = VECTOR ( 'NONE', #44441, 1000.000000000000000 ) ;
#47039 = ORIENTED_EDGE ( 'NONE', *, *, #25079, .T. ) ;
#47040 = ORIENTED_EDGE ( 'NONE', *, *, #34132, .F. ) ;
#47041 = CARTESIAN_POINT ( 'NONE',  ( -124.9459734468149321, -1.025126265847081886, 39.06828755692799149 ) ) ;
#47042 = CARTESIAN_POINT ( 'NONE',  ( 12.97493236725083676, -11.05939663306990717, 8.953103998512858652 ) ) ;
#47043 = DIRECTION ( 'NONE',  ( 0.000000000000000000, -0.000000000000000000, 1.000000000000000000 ) ) ;
#47044 = DIRECTION ( 'NONE',  ( -0.000000000000000000, -0.000000000000000000, -1.000000000000000000 ) ) ;
#47045 = ORIENTED_EDGE ( 'NONE', *, *, #41934, .F. ) ;
#47046 = VECTOR ( 'NONE', #11014, 1000.000000000000000 ) ;
#47047 = ORIENTED_EDGE ( 'NONE', *, *, #43704, .F. ) ;
#47048 = ORIENTED_EDGE ( 'NONE', *, *, #28141, .T. ) ;
#47049 = CARTESIAN_POINT ( 'NONE',  ( -33.86622497129646092, 3.037805405905158462, 7.906207997025717304 ) ) ;
#47050 = DIRECTION ( 'NONE',  ( 0.000000000000000000, -1.000000000000000000, 0.000000000000000000 ) ) ;
#47051 = ORIENTED_EDGE ( 'NONE', *, *, #14505, .T. ) ;
#47052 = CARTESIAN_POINT ( 'NONE',  ( 358.0000000000001137, 167.8284271247464687, 342.8284271247463266 ) ) ;
#47053 = CARTESIAN_POINT ( 'NONE',  ( 356.0000000000006253, 167.0000000000000000, 341.9999999999998295 ) ) ;
#47054 = CARTESIAN_POINT ( 'NONE',  ( 34.99999999999997868, 17.00000000000000000, -90.00000000000000000 ) ) ;
#47055 = VECTOR ( 'NONE', #36830, 1000.000000000000000 ) ;
#47056 = VERTEX_POINT ( 'NONE', #16710 ) ;
#47057 = VERTEX_POINT ( 'NONE', #20310 ) ;
#47058 = CARTESIAN_POINT ( 'NONE',  ( -208.1473046169136580, -154.8119894309599260, 470.5025600500171095 ) ) ;
#47059 = ADVANCED_FACE ( 'NONE', ( #8525 ), #43396, .F. ) ;
#47060 = CARTESIAN_POINT ( 'NONE',  ( -45.67084718096785423, 1.750000000000009548, -40.20683870891912193 ) ) ;
#47061 = CYLINDRICAL_SURFACE ( 'NONE', #26541, 1.750000000000001554 ) ;
#47062 = ORIENTED_EDGE ( 'NONE', *, *, #4222, .F. ) ;
#47063 = ORIENTED_EDGE ( 'NONE', *, *, #6798, .T. ) ;
#47064 = VECTOR ( 'NONE', #32793, 1000.000000000000000 ) ;
#47065 = CARTESIAN_POINT ( 'NONE',  ( 164.9999999999999716, 16.00000000000000000, -60.00000000000000000 ) ) ;
#47066 = VERTEX_POINT ( 'NONE', #24179 ) ;
#47067 = CARTESIAN_POINT ( 'NONE',  ( 73.30402655318508209, 0.000000000000000000, 165.0000000000000000 ) ) ;
#47068 = CARTESIAN_POINT ( 'NONE',  ( -556.8973046169135159, -61.66198943095990614, -64.63743994998280584 ) ) ;
#47069 = CARTESIAN_POINT ( 'NONE',  ( 151.5540265531850537, -1.025126265847089435, -40.93171244307204404 ) ) ;
#47070 = ORIENTED_EDGE ( 'NONE', *, *, #17445, .T. ) ;
#47071 = CARTESIAN_POINT ( 'NONE',  ( 75.05402655318509630, 2.143131898507880377E-16, 165.0000000000000000 ) ) ;
#47072 = LINE ( 'NONE', #19912, #45309 ) ;
#47073 = CARTESIAN_POINT ( 'NONE',  ( 339.9999999999999432, -181.0000000000001421, -356.0000000000003411 ) ) ;
#47074 = ADVANCED_FACE ( 'NONE', ( #28011 ), #6474, .T. ) ;
#47075 = CARTESIAN_POINT ( 'NONE',  ( 359.9999999999999432, 174.9999999999996589, -356.0000000000003411 ) ) ;
#47076 = VECTOR ( 'NONE', #34712, 1000.000000000000000 ) ;
#47077 = CARTESIAN_POINT ( 'NONE',  ( 40.00000000000000000, 4.898587196589413026E-15, 790.0000000000000000 ) ) ;
#47078 = CARTESIAN_POINT ( 'NONE',  ( 4.641001526964560142, 50.00000000000000711, -8.016098858316199838 ) ) ;
#47079 = ADVANCED_FACE ( 'NONE', ( #35983 ), #15703, .T. ) ;
#47080 = LINE ( 'NONE', #27639, #24679 ) ;
#47082 = ORIENTED_EDGE ( 'NONE', *, *, #25874, .F. ) ;
#47081 = ADVANCED_FACE ( 'NONE', ( #23412 ), #4903, .F. ) ;
#47083 = CARTESIAN_POINT ( 'NONE',  ( 168.9999999999998863, 165.0000000000000000, 357.9999999999998863 ) ) ;
#47084 = VECTOR ( 'NONE', #48518, 1000.000000000000000 ) ;
#47085 = PLANE ( 'NONE',  #6523 ) ;
#47086 = AXIS2_PLACEMENT_3D ( 'NONE', #707, #16357, #32023 ) ;
#47087 = ORIENTED_EDGE ( 'NONE', *, *, #1093, .T. ) ;
#47088 = CARTESIAN_POINT ( 'NONE',  ( 35.05402655318504657, -1.025126265847089213, 42.56828755692799149 ) ) ;
#47089 = CARTESIAN_POINT ( 'NONE',  ( 0.000000000000000000, 0.000000000000000000, 15.00000000000000000 ) ) ;
#47090 = CARTESIAN_POINT ( 'NONE',  ( 19.81499429539178436, -31.87968861126187647, -5.338708898921614932 ) ) ;
#47091 = ORIENTED_EDGE ( 'NONE', *, *, #4524, .F. ) ;
#47092 = AXIS2_PLACEMENT_3D ( 'NONE', #50274, #42866, #22871 ) ;
#47093 = VERTEX_POINT ( 'NONE', #578 ) ;
#47094 = ORIENTED_EDGE ( 'NONE', *, *, #9820, .F. ) ;
#47095 = CARTESIAN_POINT ( 'NONE',  ( 31.93002621080262671, 9.285431160462559674, -2.408242355805840784 ) ) ;
#47096 = FACE_OUTER_BOUND ( 'NONE', #17919, .T. ) ;
#47097 =( BOUNDED_CURVE ( )  B_SPLINE_CURVE ( 3, ( #21325, #2821, #18479, #29280 ),
 .UNSPECIFIED., .F., .F. ) 
 B_SPLINE_CURVE_WITH_KNOTS ( ( 4, 4 ),
 ( 4.712388980384689674, 6.283185307179586232 ),
 .UNSPECIFIED. ) 
 CURVE ( )  GEOMETRIC_REPRESENTATION_ITEM ( )  RATIONAL_B_SPLINE_CURVE ( ( 1.000000000000000000, 0.8047378541243649375, 0.8047378541243649375, 1.000000000000000000 ) ) 
 REPRESENTATION_ITEM ( '' )  );
#47098 = EDGE_LOOP ( 'NONE', ( #3390, #2757, #9922, #23118, #29830 ) ) ;
#47099 = CARTESIAN_POINT ( 'NONE',  ( 29.99999999999998579, 16.00000000000000000, -114.9999999999999858 ) ) ;
#47100 = DIRECTION ( 'NONE',  ( 1.000000000000000000, 0.000000000000000000, 4.758098658057970186E-16 ) ) ;
#47101 =( BOUNDED_CURVE ( )  B_SPLINE_CURVE ( 3, ( #36231, #20805, #39316, #35473 ),
 .UNSPECIFIED., .F., .F. ) 
 B_SPLINE_CURVE_WITH_KNOTS ( ( 4, 4 ),
 ( 0.000000000000000000, 1.570796326794896558 ),
 .UNSPECIFIED. ) 
 CURVE ( )  GEOMETRIC_REPRESENTATION_ITEM ( )  RATIONAL_B_SPLINE_CURVE ( ( 1.000000000000000000, 0.8047378541243649375, 0.8047378541243649375, 1.000000000000000000 ) ) 
 REPRESENTATION_ITEM ( '' )  );
#47102 = DIRECTION ( 'NONE',  ( 2.958228394578793832E-31, 0.000000000000000000, 1.000000000000000000 ) ) ;
#47103 = ORIENTED_EDGE ( 'NONE', *, *, #16718, .T. ) ;
#47104 = LINE ( 'NONE', #12009, #21706 ) ;
#47105 = DIRECTION ( 'NONE',  ( 0.7233555441435720601, 0.6904757466825006684, 0.000000000000000000 ) ) ;
#47106 = LINE ( 'NONE', #12011, #7029 ) ;
#47107 = AXIS2_PLACEMENT_3D ( 'NONE', #13185, #41398, #1650 ) ;
#47108 = EDGE_CURVE ( 'NONE', #3038, #29536, #27517, .T. ) ;
#47109 = ORIENTED_EDGE ( 'NONE', *, *, #7377, .T. ) ;
#47110 = EDGE_CURVE ( 'NONE', #25007, #44339, #16217, .T. ) ;
#47111 = PLANE ( 'NONE',  #37432 ) ;
#47112 = DIRECTION ( 'NONE',  ( -0.000000000000000000, -0.000000000000000000, -1.000000000000000000 ) ) ;
#47113 = ORIENTED_EDGE ( 'NONE', *, *, #176, .F. ) ;
#47114 = VECTOR ( 'NONE', #8452, 1000.000000000000000 ) ;
#47115 = ORIENTED_EDGE ( 'NONE', *, *, #7621, .T. ) ;
#47116 = ORIENTED_EDGE ( 'NONE', *, *, #4189, .T. ) ;
#47117 = CARTESIAN_POINT ( 'NONE',  ( 20.37409433807990666, 26.28007012093483397, -2.408242355805840784 ) ) ;
#47118 = EDGE_CURVE ( 'NONE', #40366, #46863, #4163, .T. ) ;
#47119 = CIRCLE ( 'NONE', #34877, 4.000000000000003553 ) ;
#47120 =( BOUNDED_CURVE ( )  B_SPLINE_CURVE ( 3, ( #33135, #48215, #28763, #44140 ),
 .UNSPECIFIED., .F., .F. ) 
 B_SPLINE_CURVE_WITH_KNOTS ( ( 4, 4 ),
 ( 0.000000000000000000, 1.570796326794896558 ),
 .UNSPECIFIED. ) 
 CURVE ( )  GEOMETRIC_REPRESENTATION_ITEM ( )  RATIONAL_B_SPLINE_CURVE ( ( 1.000000000000000000, 0.8047378541243649375, 0.8047378541243649375, 1.000000000000000000 ) ) 
 REPRESENTATION_ITEM ( '' )  );
#47121 = CARTESIAN_POINT ( 'NONE',  ( 135.0000000000021600, 17.00000000000000000, 95.00000000000000000 ) ) ;
#47122 = EDGE_LOOP ( 'NONE', ( #25835, #48603, #6287, #39911, #35292, #21767 ) ) ;
#47123 = EDGE_CURVE ( 'NONE', #16301, #26083, #32573, .T. ) ;
#47124 = CARTESIAN_POINT ( 'NONE',  ( -7.241383964640739634, -3.469446951953614189E-15, 5.000000000000000000 ) ) ;
#47125 = DIRECTION ( 'NONE',  ( -1.000000000000000000, 0.000000000000000000, 0.000000000000000000 ) ) ;
#47126 = CARTESIAN_POINT ( 'NONE',  ( -15.00099850811941948, -7.462898891544107016, 9.403735324607438884 ) ) ;
#47127 = AXIS2_PLACEMENT_3D ( 'NONE', #23896, #32105, #12847 ) ;
#47128 = CARTESIAN_POINT ( 'NONE',  ( -1.114871695981121125, 0.4953159757245923500, 9.963925895596188909 ) ) ;
#47129 = CARTESIAN_POINT ( 'NONE',  ( 8.277096487746778308, -33.14818118907697198, 7.455576670931136185 ) ) ;
#47130 = DIRECTION ( 'NONE',  ( 1.734723475976805319E-15, 0.000000000000000000, 1.000000000000000000 ) ) ;
#47131 = DIRECTION ( 'NONE',  ( -1.000000000000000000, 0.000000000000000000, 0.000000000000000000 ) ) ;
#47132 = DIRECTION ( 'NONE',  ( 0.000000000000000000, 0.000000000000000000, -1.000000000000000000 ) ) ;
#47133 = DIRECTION ( 'NONE',  ( -0.000000000000000000, -0.000000000000000000, -1.000000000000000000 ) ) ;
#47134 = LINE ( 'NONE', #8188, #35929 ) ;
#47135 = AXIS2_PLACEMENT_3D ( 'NONE', #16631, #9434, #25100 ) ;
#47136 = AXIS2_PLACEMENT_3D ( 'NONE', #9347, #12682, #13189 ) ;
#47137 = DIRECTION ( 'NONE',  ( -4.625929269271635797E-16, 0.000000000000000000, -1.000000000000000000 ) ) ;
#47138 = LINE ( 'NONE', #30517, #42972 ) ;
#47139 = DIRECTION ( 'NONE',  ( 0.000000000000000000, -1.000000000000000000, 0.000000000000000000 ) ) ;
#47140 = CARTESIAN_POINT ( 'NONE',  ( 9.907356528111447957, -1.358045148324435347, 0.000000000000000000 ) ) ;
#47141 = ORIENTED_EDGE ( 'NONE', *, *, #1188, .T. ) ;
#47142 = CARTESIAN_POINT ( 'NONE',  ( -128.4459734468149463, 1.025126265847081886, -80.93171244307201562 ) ) ;
#47143 = DIRECTION ( 'NONE',  ( 0.000000000000000000, 0.000000000000000000, -1.000000000000000000 ) ) ;
#47144 = DIRECTION ( 'NONE',  ( 0.000000000000000000, 0.000000000000000000, 1.000000000000000000 ) ) ;
#47145 = EDGE_CURVE ( 'NONE', #29162, #9194, #23720, .T. ) ;
#47146 = EDGE_CURVE ( 'NONE', #25202, #7505, #33395, .T. ) ;
#47147 = DIRECTION ( 'NONE',  ( -0.000000000000000000, -0.000000000000000000, -1.000000000000000000 ) ) ;
#47149 = ORIENTED_EDGE ( 'NONE', *, *, #30990, .T. ) ;
#47148 = EDGE_CURVE ( 'NONE', #44274, #36068, #48472, .T. ) ;
#47150 = VECTOR ( 'NONE', #5613, 1000.000000000000000 ) ;
#47151 = CARTESIAN_POINT ( 'NONE',  ( 93.25146017538654064, 159.2880105690400399, 648.6585061788589428 ) ) ;
#47152 = EDGE_CURVE ( 'NONE', #2282, #8731, #17035, .T. ) ;
#47153 = ORIENTED_EDGE ( 'NONE', *, *, #27757, .T. ) ;
#47154 = DIRECTION ( 'NONE',  ( -1.586032892321652236E-16, -1.000000000000000000, -2.288264760618012091E-48 ) ) ;
#47155 = AXIS2_PLACEMENT_3D ( 'NONE', #13507, #17614, #41722 ) ;
#47156 = VERTEX_POINT ( 'NONE', #41327 ) ;
#47157 = ADVANCED_FACE ( 'NONE', ( #17225 ), #17471, .F. ) ;
#47158 = CARTESIAN_POINT ( 'NONE',  ( -6.880036658038818587, -197.4999999999999432, -228.6347188485896140 ) ) ;
#47159 = CARTESIAN_POINT ( 'NONE',  ( 370.7621192902014968, 70.03596893647589638, -94.69675437945477370 ) ) ;
#47160 = EDGE_CURVE ( 'NONE', #28712, #34498, #1332, .T. ) ;
#47161 = ORIENTED_EDGE ( 'NONE', *, *, #17069, .T. ) ;
#47162 = CARTESIAN_POINT ( 'NONE',  ( -165.3973046169136012, 103.9380105690400597, -17.65743994998277699 ) ) ;
#47163 = ORIENTED_EDGE ( 'NONE', *, *, #17840, .T. ) ;
#47164 = VECTOR ( 'NONE', #29418, 1000.000000000000000 ) ;
#47165 = ORIENTED_EDGE ( 'NONE', *, *, #14872, .T. ) ;
#47166 = CARTESIAN_POINT ( 'NONE',  ( 191.5540265531850537, 1.025126265847089435, 82.56828755692798438 ) ) ;
#47167 = DIRECTION ( 'NONE',  ( 0.000000000000000000, -1.000000000000000000, -3.186989995019654210E-49 ) ) ;
#47168 = CIRCLE ( 'NONE', #16050, 2.000000000000001776 ) ;
#47169 = VERTEX_POINT ( 'NONE', #9515 ) ;
#47170 = CARTESIAN_POINT ( 'NONE',  ( -10.70590866674912967, 12.76446523155714985, -3.546734833711462365 ) ) ;
#47171 = CARTESIAN_POINT ( 'NONE',  ( -1.197382828408634081, 0.5140992728904327791, 9.961922210043265835 ) ) ;
#47172 = CARTESIAN_POINT ( 'NONE',  ( 50.11058929355269953, -7.578863168071589662, 7.455576670931136185 ) ) ;
#47173 = VERTEX_POINT ( 'NONE', #29023 ) ;
#47174 = LINE ( 'NONE', #8223, #38231 ) ;
#47175 = ADVANCED_FACE ( 'NONE', ( #37504 ), #32630, .T. ) ;
#47176 = CARTESIAN_POINT ( 'NONE',  ( -84.94597344681493212, -1.025126265847089435, -117.4317124430720156 ) ) ;
#47177 = EDGE_CURVE ( 'NONE', #19067, #40717, #29524, .T. ) ;
#47178 = VERTEX_POINT ( 'NONE', #44641 ) ;
#47179 = EDGE_CURVE ( 'NONE', #7572, #214, #49284, .T. ) ;
#47180 = CARTESIAN_POINT ( 'NONE',  ( 153.3040265531850537, 1.750000000000010658, 80.81828755692798438 ) ) ;
#47181 = CARTESIAN_POINT ( 'NONE',  ( 2.500000000000002665, 204.9999999999999716, -234.7500000000000000 ) ) ;
#47182 = ORIENTED_EDGE ( 'NONE', *, *, #24898, .T. ) ;
#47183 = CARTESIAN_POINT ( 'NONE',  ( -86.69597344681494633, 1.750000000000009992, 0.8182875569279768335 ) ) ;
#47184 = CARTESIAN_POINT ( 'NONE',  ( -167.4999999999999716, 74.83106485270648989, -120.5992382549688955 ) ) ;
#47185 = EDGE_LOOP ( 'NONE', ( #20767, #36809, #38587, #20185 ) ) ;
#47186 = CARTESIAN_POINT ( 'NONE',  ( 0.9300423221600994106, 1.714483250866464914, 9.896382706792429929 ) ) ;
#47187 = CARTESIAN_POINT ( 'NONE',  ( -6.695973446814940111, 0.000000000000000000, 165.0000000000000000 ) ) ;
#47188 = CARTESIAN_POINT ( 'NONE',  ( 0.000000000000000000, 0.000000000000000000, 0.000000000000000000 ) ) ;
#47189 = DIRECTION ( 'NONE',  ( 0.000000000000000000, 1.000000000000000000, 0.000000000000000000 ) ) ;
#47190 = AXIS2_PLACEMENT_3D ( 'NONE', #87, #5182, #24197 ) ;
#47191 = VERTEX_POINT ( 'NONE', #10027 ) ;
#47192 = CARTESIAN_POINT ( 'NONE',  ( 34.99999999999997868, 17.00000000000000000, -90.00000000000000000 ) ) ;
#47193 = VECTOR ( 'NONE', #34180, 1000.000000000000000 ) ;
#47194 = CARTESIAN_POINT ( 'NONE',  ( 14.29087950072012170, 9.652079258044652832, 8.727788335465566760 ) ) ;
#47195 = EDGE_CURVE ( 'NONE', #3066, #19764, #12865, .T. ) ;
#47196 = CARTESIAN_POINT ( 'NONE',  ( 166.9999999999999716, -256.4999999999996589, -114.9999999999999574 ) ) ;
#47197 = EDGE_LOOP ( 'NONE', ( #44917, #47231, #18258, #10570 ) ) ;
#47198 = VERTEX_POINT ( 'NONE', #40324 ) ;
#47199 = CARTESIAN_POINT ( 'NONE',  ( 867.4995338190013854, 1458.153237050701819, 1561.986414963432480 ) ) ;
#47200 = DIRECTION ( 'NONE',  ( 1.000000000000000000, 0.000000000000000000, 0.000000000000000000 ) ) ;
#47201 = VECTOR ( 'NONE', #15666, 1000.000000000000000 ) ;
#47202 = CARTESIAN_POINT ( 'NONE',  ( -0.8285222815141961572, -1.889008401827320771, 9.886433018048073507 ) ) ;
#47203 = CARTESIAN_POINT ( 'NONE',  ( -23.29043492822808759, 24.10797434788186067, 1.847720168420772691 ) ) ;
#47204 = AXIS2_PLACEMENT_3D ( 'NONE', #30716, #34562, #38173 ) ;
#47205 = ADVANCED_FACE ( 'NONE', ( #5160 ), #44395, .T. ) ;
#47206 = CARTESIAN_POINT ( 'NONE',  ( -210.0000000000000568, 2.143131898507884075E-16, -40.93171244307203693 ) ) ;
#47207 = ORIENTED_EDGE ( 'NONE', *, *, #45305, .T. ) ;
#47208 = CARTESIAN_POINT ( 'NONE',  ( -114.9999999999978542, 16.00000000000000000, 95.00000000000000000 ) ) ;
#47209 = FACE_OUTER_BOUND ( 'NONE', #23515, .T. ) ;
#47210 = PLANE ( 'NONE',  #33193 ) ;
#47211 = FACE_OUTER_BOUND ( 'NONE', #32592, .T. ) ;
#47212 = VECTOR ( 'NONE', #44039, 1000.000000000000000 ) ;
#47214 = VERTEX_POINT ( 'NONE', #29274 ) ;
#47213 = ADVANCED_FACE ( 'NONE', ( #5412 ), #1827, .T. ) ;
#47215 = DIRECTION ( 'NONE',  ( -5.473822126268816076E-48, 1.000000000000000000, 1.654361225106055350E-24 ) ) ;
#47216 = EDGE_CURVE ( 'NONE', #31506, #9910, #24771, .T. ) ;
#47217 = ORIENTED_EDGE ( 'NONE', *, *, #23470, .T. ) ;
#47218 = DIRECTION ( 'NONE',  ( 0.000000000000000000, 0.000000000000000000, 1.000000000000000000 ) ) ;
#47219 = EDGE_LOOP ( 'NONE', ( #49224, #40092, #24497 ) ) ;
#47220 = CYLINDRICAL_SURFACE ( 'NONE', #5756, 1.750000000000008438 ) ;
#47221 = CARTESIAN_POINT ( 'NONE',  ( -206.6959734468149463, -1.750000000000009992, 160.8182875569279702 ) ) ;
#47222 = EDGE_CURVE ( 'NONE', #47848, #12229, #9766, .T. ) ;
#47223 = CARTESIAN_POINT ( 'NONE',  ( 339.9999999999999432, -169.0000000000001137, 344.0000000000000000 ) ) ;
#47224 = FACE_OUTER_BOUND ( 'NONE', #42312, .T. ) ;
#47225 = ORIENTED_EDGE ( 'NONE', *, *, #1804, .T. ) ;
#47226 = ADVANCED_FACE ( 'NONE', ( #22324 ), #22076, .T. ) ;
#47227 = EDGE_CURVE ( 'NONE', #10600, #6064, #3777, .T. ) ;
#47228 = DIRECTION ( 'NONE',  ( 1.000000000000000000, -0.000000000000000000, 0.000000000000000000 ) ) ;
#47229 = VECTOR ( 'NONE', #35638, 1000.000000000000000 ) ;
#47230 = PLANE ( 'NONE',  #40162 ) ;
#47231 = ORIENTED_EDGE ( 'NONE', *, *, #20390, .F. ) ;
#47232 = CARTESIAN_POINT ( 'NONE',  ( -0.8283411193296142949, -1.889045124114520080, 9.891980816076525684 ) ) ;
#47233 = CARTESIAN_POINT ( 'NONE',  ( 33.30402655318503946, -1.750000000000010214, 40.81828755692798438 ) ) ;
#47234 = DIRECTION ( 'NONE',  ( -1.000000000000000000, 0.000000000000000000, 1.586032892321651989E-16 ) ) ;
#47235 = CARTESIAN_POINT ( 'NONE',  ( 75.05402655318509630, 2.143131898507880377E-16, 165.0000000000000000 ) ) ;
#47236 = EDGE_CURVE ( 'NONE', #1434, #49119, #42575, .T. ) ;
#47237 = EDGE_LOOP ( 'NONE', ( #47476, #21490, #30601, #5118 ) ) ;
#47238 = ORIENTED_EDGE ( 'NONE', *, *, #33834, .T. ) ;
#47239 = CARTESIAN_POINT ( 'NONE',  ( -25.40454589245989325, -27.58367357691681931, -8.192531242611266862 ) ) ;
#47240 = ORIENTED_EDGE ( 'NONE', *, *, #13644, .F. ) ;
#47241 = LINE ( 'NONE', #34741, #45413 ) ;
#47242 = CARTESIAN_POINT ( 'NONE',  ( 80.00000000000061107, 16.00000000000000000, -54.99999999999999289 ) ) ;
#47243 = CYLINDRICAL_SURFACE ( 'NONE', #5955, 1.750000000000001554 ) ;
#47244 = VERTEX_POINT ( 'NONE', #46405 ) ;
#47245 = CARTESIAN_POINT ( 'NONE',  ( 432.7825420346616170, 47.50000000000000000, -120.5992382549688955 ) ) ;
#47246 = VERTEX_POINT ( 'NONE', #18974 ) ;
#47247 = ORIENTED_EDGE ( 'NONE', *, *, #24892, .T. ) ;
#47248 = VECTOR ( 'NONE', #4435, 1000.000000000000000 ) ;
#47249 = CARTESIAN_POINT ( 'NONE',  ( -20.72411365307686637, 36.23316402738157649, -8.080361901872242569 ) ) ;
#47250 = CARTESIAN_POINT ( 'NONE',  ( -1.249999999999999778, 0.000000000000000000, 10.00000000000000000 ) ) ;
#47251 = VERTEX_POINT ( 'NONE', #41827 ) ;
#47252 = ORIENTED_EDGE ( 'NONE', *, *, #2313, .T. ) ;
#47253 = ORIENTED_EDGE ( 'NONE', *, *, #22038, .F. ) ;
#47254 = PLANE ( 'NONE',  #13191 ) ;
#47255 = FACE_OUTER_BOUND ( 'NONE', #41869, .T. ) ;
#47256 = FACE_OUTER_BOUND ( 'NONE', #37591, .T. ) ;
#47257 = PRODUCT_DEFINITION_CONTEXT ( 'detailed design', #20728, 'design' ) ;
#47258 = EDGE_LOOP ( 'NONE', ( #16750, #35529, #36332, #28806 ) ) ;
#47259 = LINE ( 'NONE', #12896, #27261 ) ;
#47260 = ORIENTED_EDGE ( 'NONE', *, *, #37313, .F. ) ;
#47261 = EDGE_CURVE ( 'NONE', #23604, #15862, #49471, .T. ) ;
#47262 = CARTESIAN_POINT ( 'NONE',  ( 85.00000000000152056, 16.00000000000000000, 60.00000000000000000 ) ) ;
#47263 = EDGE_LOOP ( 'NONE', ( #10974, #43440 ) ) ;
#47264 = CARTESIAN_POINT ( 'NONE',  ( 0.000000000000000000, 17.00000000000000000, 0.000000000000000000 ) ) ;
#47265 = FACE_OUTER_BOUND ( 'NONE', #50293, .T. ) ;
#47266 = CARTESIAN_POINT ( 'NONE',  ( -86.69597344681494633, -1.750000000000009992, -159.1817124430720298 ) ) ;
#47267 = DIRECTION ( 'NONE',  ( 1.586032892321651989E-16, -3.736034562988530447E-32, 1.000000000000000000 ) ) ;
#47268 = AXIS2_PLACEMENT_3D ( 'NONE', #47910, #20750, #16649 ) ;
#47269 =( NAMED_UNIT ( * ) PLANE_ANGLE_UNIT ( ) SI_UNIT ( $, .RADIAN. ) );
#47270 = LINE ( 'NONE', #623, #8598 ) ;
#47271 = DIRECTION ( 'NONE',  ( 0.000000000000000000, 0.000000000000000000, -1.000000000000000000 ) ) ;
#47272 = ORIENTED_EDGE ( 'NONE', *, *, #25307, .T. ) ;
#47273 = VERTEX_POINT ( 'NONE', #38000 ) ;
#47274 = CARTESIAN_POINT ( 'NONE',  ( 80.00000000000186162, 17.00000000000000000, 65.00000000000000000 ) ) ;
#47275 =( BOUNDED_CURVE ( )  B_SPLINE_CURVE ( 3, ( #33867, #22298, #18441, #49455 ),
 .UNSPECIFIED., .F., .F. ) 
 B_SPLINE_CURVE_WITH_KNOTS ( ( 4, 4 ),
 ( 1.570796326794896558, 3.141592653589793116 ),
 .UNSPECIFIED. ) 
 CURVE ( )  GEOMETRIC_REPRESENTATION_ITEM ( )  RATIONAL_B_SPLINE_CURVE ( ( 1.000000000000000000, 0.8047378541243649375, 0.8047378541243649375, 1.000000000000000000 ) ) 
 REPRESENTATION_ITEM ( '' )  );
#47276 = CARTESIAN_POINT ( 'NONE',  ( 152.2789002873379900, -1.750000000000009548, 159.7931612910809065 ) ) ;
#47277 = CARTESIAN_POINT ( 'NONE',  ( 175.0000000000000000, 15.00000000000000000, 122.5000000000000142 ) ) ;
#47278 = B_SPLINE_CURVE_WITH_KNOTS ( 'NONE', 3,
 ( #38857, #50070, #15486, #46742 ),
 .UNSPECIFIED., .F., .F.,
 ( 4, 4 ),
 ( 0.000000000000000000, 0.2545280377015985418 ),
 .UNSPECIFIED. ) ;
#47279 = EDGE_CURVE ( 'NONE', #50433, #32098, #49980, .T. ) ;
#47280 = FACE_OUTER_BOUND ( 'NONE', #19567, .T. ) ;
#47281 = ADVANCED_FACE ( 'NONE', ( #45396 ), #38263, .T. ) ;
#47282 = DIRECTION ( 'NONE',  ( 1.000000000000000000, 0.000000000000000000, 0.000000000000000000 ) ) ;
#47283 = EDGE_LOOP ( 'NONE', ( #11383, #5011, #7466, #10393 ) ) ;
#47284 = DIRECTION ( 'NONE',  ( -0.000000000000000000, -1.000000000000000000, -0.000000000000000000 ) ) ;
#47285 = ADVANCED_FACE ( 'NONE', ( #22831 ), #34651, .T. ) ;
#47286 = CARTESIAN_POINT ( 'NONE',  ( -164.9999999999987779, 17.00000000000000000, 5.000000000000004441 ) ) ;
#47287 = EDGE_CURVE ( 'NONE', #12365, #8857, #9032, .T. ) ;
#47288 = EDGE_CURVE ( 'NONE', #45663, #19177, #47946, .T. ) ;
#47289 = ORIENTED_EDGE ( 'NONE', *, *, #46934, .T. ) ;
#47290 = FACE_OUTER_BOUND ( 'NONE', #27303, .T. ) ;
#47291 = ADVANCED_FACE ( 'NONE', ( #38755, #18212 ), #11293, .F. ) ;
#47292 = DIRECTION ( 'NONE',  ( 0.000000000000000000, 0.000000000000000000, -1.000000000000000000 ) ) ;
#47293 = ORIENTED_EDGE ( 'NONE', *, *, #9600, .T. ) ;
#47294 = EDGE_LOOP ( 'NONE', ( #37835, #33377, #24338, #16799 ) ) ;
#47295 = LINE ( 'NONE', #35552, #22600 ) ;
#47296 = DIRECTION ( 'NONE',  ( 1.000000000000000000, 0.000000000000000000, -0.000000000000000000 ) ) ;
#47297 = VECTOR ( 'NONE', #27628, 1000.000000000000000 ) ;
#47298 = VERTEX_POINT ( 'NONE', #26425 ) ;
#47299 = EDGE_LOOP ( 'NONE', ( #1071, #31920, #44562, #668 ) ) ;
#47300 = LINE ( 'NONE', #50444, #14669 ) ;
#47301 = CARTESIAN_POINT ( 'NONE',  ( 135.0000000000006253, 17.00000000000000000, -30.00000000000000000 ) ) ;
#47302 = CARTESIAN_POINT ( 'NONE',  ( -1.249999999999999778, 0.000000000000000000, 10.00000000000000000 ) ) ;
#47303 = DIRECTION ( 'NONE',  ( -1.000000000000000000, 0.000000000000000000, 0.000000000000000000 ) ) ;
#47304 = DIRECTION ( 'NONE',  ( -1.000000000000000000, 0.000000000000000000, 0.000000000000000000 ) ) ;
#47305 = ORIENTED_EDGE ( 'NONE', *, *, #10006, .T. ) ;
#47306 = ORIENTED_EDGE ( 'NONE', *, *, #39974, .T. ) ;
#47307 = ORIENTED_EDGE ( 'NONE', *, *, #2138, .F. ) ;
#47308 = CARTESIAN_POINT ( 'NONE',  ( 25.63461350838963071, -43.17876197216376255, -8.016098858316205167 ) ) ;
#47309 = EDGE_LOOP ( 'NONE', ( #5226, #20984, #33415, #41261, #37823, #2947 ) ) ;
#47310 = LINE ( 'NONE', #16305, #37762 ) ;
#47311 = ORIENTED_EDGE ( 'NONE', *, *, #12533, .F. ) ;
#47312 = ORIENTED_EDGE ( 'NONE', *, *, #16654, .F. ) ;
#47313 = CARTESIAN_POINT ( 'NONE',  ( 224.9999999999999432, -175.0000000000000000, 444.9999999999998295 ) ) ;
#47314 = ADVANCED_FACE ( 'NONE', ( #17959 ), #23081, .T. ) ;
#47315 = CARTESIAN_POINT ( 'NONE',  ( 2.569099690548740877, -33.19126772784019153, 3.199614146704519602 ) ) ;
#47316 = AXIS2_PLACEMENT_3D ( 'NONE', #6017, #33493, #10627 ) ;
#47317 = CARTESIAN_POINT ( 'NONE',  ( 8.277096487746778308, -50.00000000000000000, 7.455576670931136185 ) ) ;
#47318 = ORIENTED_EDGE ( 'NONE', *, *, #13519, .T. ) ;
#47319 = ORIENTED_EDGE ( 'NONE', *, *, #34632, .T. ) ;
#47320 = EDGE_CURVE ( 'NONE', #21137, #32019, #26691, .T. ) ;
#47321 = CARTESIAN_POINT ( 'NONE',  ( 31.55402655318503236, 0.000000000000000000, -0.9317124430720247208 ) ) ;
#47322 = LINE ( 'NONE', #19655, #36291 ) ;
#47323 = ORIENTED_EDGE ( 'NONE', *, *, #24926, .T. ) ;
#47324 = DIRECTION ( 'NONE',  ( 0.000000000000000000, -2.969158215481698263E-48, 1.000000000000000000 ) ) ;
#47325 = CYLINDRICAL_SURFACE ( 'NONE', #44021, 40.00000000000000000 ) ;
#47326 = CARTESIAN_POINT ( 'NONE',  ( -2.538055338523173443, -45.80735277814159190, -9.367992836599951190 ) ) ;
#47327 = DIRECTION ( 'NONE',  ( -0.000000000000000000, -0.000000000000000000, -1.000000000000000000 ) ) ;
#47328 = EDGE_LOOP ( 'NONE', ( #10618, #10585, #25996, #560, #36061, #30583 ) ) ;
#47329 = CARTESIAN_POINT ( 'NONE',  ( 35.00000000000122213, 16.00000000000000000, 30.00000000000000000 ) ) ;
#47330 = CARTESIAN_POINT ( 'NONE',  ( -8.445973446814976526, 0.000000000000000000, 42.56828755692802702 ) ) ;
#47331 = LINE ( 'NONE', #11978, #29386 ) ;
#47332 = CARTESIAN_POINT ( 'NONE',  ( 183.0000000000000000, -268.5000000000000000, -339.9999999999998863 ) ) ;
#47333 = AXIS2_PLACEMENT_3D ( 'NONE', #14288, #10952, #37923 ) ;
#47334 = CARTESIAN_POINT ( 'NONE',  ( 195.0540265531851105, -1.025126265847089213, -0.9317124430720324924 ) ) ;
#47335 = DIRECTION ( 'NONE',  ( 1.000000000000000000, 0.000000000000000000, 0.000000000000000000 ) ) ;
#47336 = CARTESIAN_POINT ( 'NONE',  ( 195.0540265531851105, 1.025126265847089213, -160.9317124430720014 ) ) ;
#47337 = ORIENTED_EDGE ( 'NONE', *, *, #4350, .F. ) ;
#47338 = SURFACE_STYLE_FILL_AREA ( #4776 ) ;
#47339 = DIRECTION ( 'NONE',  ( 0.000000000000000000, 1.000000000000000000, 0.000000000000000000 ) ) ;
#47340 = ORIENTED_EDGE ( 'NONE', *, *, #49699, .T. ) ;
#47341 = FACE_OUTER_BOUND ( 'NONE', #28139, .T. ) ;
#47342 = EDGE_CURVE ( 'NONE', #16365, #950, #3323, .T. ) ;
#47343 = LINE ( 'NONE', #23267, #26478 ) ;
#47344 = DIRECTION ( 'NONE',  ( -1.000000000000000000, 0.000000000000000000, 1.860490536778032451E-50 ) ) ;
#47345 = ORIENTED_EDGE ( 'NONE', *, *, #30059, .F. ) ;
#47346 = CARTESIAN_POINT ( 'NONE',  ( 339.9999999999999432, -166.9999999999999432, -356.0000000000002274 ) ) ;
#47347 = B_SPLINE_SURFACE_WITH_KNOTS ( 'NONE', 3, 3, ( 
 ( #21141, #25496, #33962, #36824 ),
 ( #49301, #25005, #25758, #44721 ),
 ( #32968, #37332, #41402, #6263 ),
 ( #2160, #5493, #45468, #29352 ) ),
 .UNSPECIFIED., .F., .F., .F.,
 ( 4, 4 ),
 ( 4, 4 ),
 ( 0.000000000000000000, 1.000000000000000000 ),
 ( 0.000000000000000000, 1.000000000000000000 ),
 .UNSPECIFIED. ) ;
#47348 = ORIENTED_EDGE ( 'NONE', *, *, #18325, .T. ) ;
#47349 = ORIENTED_EDGE ( 'NONE', *, *, #4981, .T. ) ;
#47350 = CARTESIAN_POINT ( 'NONE',  ( -239.0000000000000853, 0.000000000000000000, 0.000000000000000000 ) ) ;
#47351 = CARTESIAN_POINT ( 'NONE',  ( 356.0000000000000568, 183.0000000000000853, 357.9999999999998295 ) ) ;
#47352 = ORIENTED_EDGE ( 'NONE', *, *, #21188, .F. ) ;
#47353 = DIRECTION ( 'NONE',  ( -1.000000000000000000, 0.000000000000000000, -7.793956916774525800E-48 ) ) ;
#47354 = DIRECTION ( 'NONE',  ( 1.000000000000000000, 6.344131455081961406E-16, -4.759647537211363479E-16 ) ) ;
#47355 = VERTEX_POINT ( 'NONE', #14112 ) ;
#47356 = CARTESIAN_POINT ( 'NONE',  ( 0.5133303889071102466, -1.273801409042637944, 9.946805383069644790 ) ) ;
#47357 = ORIENTED_EDGE ( 'NONE', *, *, #24488, .T. ) ;
#47358 = DIRECTION ( 'NONE',  ( -1.156482317317870492E-16, 1.000000000000000000, 0.000000000000000000 ) ) ;
#47359 = CARTESIAN_POINT ( 'NONE',  ( -85.67084718096784002, -1.750000000000010436, -120.2068387089191219 ) ) ;
#47360 =( LENGTH_UNIT ( ) NAMED_UNIT ( * ) SI_UNIT ( .MILLI., .METRE. ) );
#47361 = VERTEX_POINT ( 'NONE', #25943 ) ;
#47362 = CIRCLE ( 'NONE', #12964, 2.000000000000001776 ) ;
#47363 = CARTESIAN_POINT ( 'NONE',  ( -4.945973446814903696, 2.143131898507912917E-16, -0.9317124430720524764 ) ) ;
#47364 = DIRECTION ( 'NONE',  ( -1.000000000000000000, 0.000000000000000000, 0.000000000000000000 ) ) ;
#47365 = ORIENTED_EDGE ( 'NONE', *, *, #9293, .F. ) ;
#47366 = ORIENTED_EDGE ( 'NONE', *, *, #44105, .F. ) ;
#47367 = ORIENTED_EDGE ( 'NONE', *, *, #39555, .F. ) ;
#47368 = CARTESIAN_POINT ( 'NONE',  ( -7.721099712662037540, -1.750000000000023315, 159.7931612910808781 ) ) ;
#47369 = DIRECTION ( 'NONE',  ( 0.000000000000000000, 0.000000000000000000, -1.000000000000000000 ) ) ;
#47370 = ORIENTED_EDGE ( 'NONE', *, *, #28748, .F. ) ;
#47371 = CLOSED_SHELL ( 'NONE', ( #33704, #24746, #23676, #11738, #17735, #6302, #19686, #15298, #12787, #28997, #3103, #17087, #44601, #12039, #36046, #13011, #50618, #39161 ) ) ;
#47372 = CARTESIAN_POINT ( 'NONE',  ( -1.011271242968683426, -0.7347315653655928092, 10.00000000000000000 ) ) ;
#47373 = CARTESIAN_POINT ( 'NONE',  ( 130.0000000000018474, 17.00000000000000000, 65.00000000000000000 ) ) ;
#47374 = CARTESIAN_POINT ( 'NONE',  ( -14.29087950072019098, -9.652079258044555132, 8.727788335465566760 ) ) ;
#47375 = DIRECTION ( 'NONE',  ( -1.000000000000000000, -0.000000000000000000, -0.000000000000000000 ) ) ;
#47376 = CARTESIAN_POINT ( 'NONE',  ( -10.49999999999999467, -46.51315789473684248, -5.916985404131818171 ) ) ;
#47377 = CARTESIAN_POINT ( 'NONE',  ( 6.875132362119187768, -50.00000000000000711, 8.356839323120299312 ) ) ;
#47378 = CARTESIAN_POINT ( 'NONE',  ( 135.0000000000000000, 17.00000000000000000, -114.9999999999999858 ) ) ;
#47379 = DIRECTION ( 'NONE',  ( 1.000000000000000000, 0.000000000000000000, 0.000000000000000000 ) ) ;
#47380 = CARTESIAN_POINT ( 'NONE',  ( 1.553324196727133621, -1.431239106454483379, 9.890170120223999106 ) ) ;
#47381 = DIRECTION ( 'NONE',  ( 1.000000000000000000, 0.000000000000000000, -0.000000000000000000 ) ) ;
#47382 = DIRECTION ( 'NONE',  ( 0.000000000000000000, 0.000000000000000000, -1.000000000000000000 ) ) ;
#47383 = DIRECTION ( 'NONE',  ( 3.364279341222519273E-16, -0.7071067811865474617, 0.7071067811865476838 ) ) ;
#47384 = CARTESIAN_POINT ( 'NONE',  ( -206.6959734468149463, -1.750000000000010214, 40.81828755692798438 ) ) ;
#47385 = CARTESIAN_POINT ( 'NONE',  ( 169.0000000000000000, -174.9999999999999716, -95.00000000000014211 ) ) ;
#47386 = VERTEX_POINT ( 'NONE', #41578 ) ;
#47387 = LINE ( 'NONE', #24105, #5688 ) ;
#47388 = CARTESIAN_POINT ( 'NONE',  ( 153.2026953830863647, -98.56198943095992604, 23.74256005001722158 ) ) ;
#47389 = PLANE ( 'NONE',  #42202 ) ;
#47390 = CARTESIAN_POINT ( 'NONE',  ( -16.76006782980216059, 2.050259795448645228, 9.178419661560148768 ) ) ;
#47391 = AXIS2_PLACEMENT_3D ( 'NONE', #20667, #1187, #24786 ) ;
#47392 =( BOUNDED_CURVE ( )  B_SPLINE_CURVE ( 3, ( #24681, #4416, #6108, #8272 ),
 .UNSPECIFIED., .F., .F. ) 
 B_SPLINE_CURVE_WITH_KNOTS ( ( 4, 4 ),
 ( 3.141592653589793116, 4.712388980384689674 ),
 .UNSPECIFIED. ) 
 CURVE ( )  GEOMETRIC_REPRESENTATION_ITEM ( )  RATIONAL_B_SPLINE_CURVE ( ( 1.000000000000000000, 0.8047378541243649375, 0.8047378541243649375, 1.000000000000000000 ) ) 
 REPRESENTATION_ITEM ( '' )  );
#47393 = ORIENTED_EDGE ( 'NONE', *, *, #4272, .F. ) ;
#47394 = CARTESIAN_POINT ( 'NONE',  ( 166.9999999999999716, -5.999999999999950262, -350.0000000000001705 ) ) ;
#47396 = ORIENTED_EDGE ( 'NONE', *, *, #1066, .T. ) ;
#47395 = CIRCLE ( 'NONE', #38450, 4.000000000000003553 ) ;
#47397 = DIRECTION ( 'NONE',  ( -1.000000000000000000, 0.000000000000000000, -1.612977847700450206E-50 ) ) ;
#47398 = VECTOR ( 'NONE', #34960, 1000.000000000000000 ) ;
#47399 = VERTEX_POINT ( 'NONE', #12544 ) ;
#47400 = CIRCLE ( 'NONE', #24530, 33.33601305720110020 ) ;
#47401 = CARTESIAN_POINT ( 'NONE',  ( 210.0000000000000568, 0.000000000000000000, 120.8182875569279702 ) ) ;
#47402 = EDGE_CURVE ( 'NONE', #9482, #27139, #50268, .T. ) ;
#47403 = CARTESIAN_POINT ( 'NONE',  ( 0.6677345994475253343, -1.504830332935386483, 9.927568724237806563 ) ) ;
#47404 = DIRECTION ( 'NONE',  ( -1.000000000000000000, 0.000000000000000000, 1.132880637372608740E-16 ) ) ;
#47405 =( BOUNDED_CURVE ( )  B_SPLINE_CURVE ( 3, ( #3631, #11336, #31094, #42872 ),
 .UNSPECIFIED., .F., .F. ) 
 B_SPLINE_CURVE_WITH_KNOTS ( ( 4, 4 ),
 ( 4.712388980384689674, 6.283185307179586232 ),
 .UNSPECIFIED. ) 
 CURVE ( )  GEOMETRIC_REPRESENTATION_ITEM ( )  RATIONAL_B_SPLINE_CURVE ( ( 1.000000000000000000, 0.8047378541243649375, 0.8047378541243649375, 1.000000000000000000 ) ) 
 REPRESENTATION_ITEM ( '' )  );
#47406 = EDGE_LOOP ( 'NONE', ( #26533, #89, #352 ) ) ;
#47407 = CARTESIAN_POINT ( 'NONE',  ( 14.49999999999999822, -46.01315789473684248, 0.000000000000000000 ) ) ;
#47408 = AXIS2_PLACEMENT_3D ( 'NONE', #3617, #10812, #38546 ) ;
#47409 = ORIENTED_EDGE ( 'NONE', *, *, #33432, .F. ) ;
#47410 = EDGE_CURVE ( 'NONE', #21250, #26375, #19481, .T. ) ;
#47411 = EDGE_CURVE ( 'NONE', #41652, #23545, #24369, .T. ) ;
#47412 = AXIS2_PLACEMENT_3D ( 'NONE', #31639, #47228, #27769 ) ;
#47413 = VERTEX_POINT ( 'NONE', #24121 ) ;
#47414 = CARTESIAN_POINT ( 'NONE',  ( 73.30402655318508209, 1.750000000000010658, 80.81828755692798438 ) ) ;
#47415 = LINE ( 'NONE', #19489, #19950 ) ;
#47416 = VERTEX_POINT ( 'NONE', #4102 ) ;
#47417 = CARTESIAN_POINT ( 'NONE',  ( -127.7210997126620242, 1.749999999999996669, -160.2068387089191219 ) ) ;
#47418 = CARTESIAN_POINT ( 'NONE',  ( 114.3291528190321173, 1.749999999999996891, -78.15658617722492352 ) ) ;
#47419 = ADVANCED_FACE ( 'NONE', ( #3578 ), #8721, .F. ) ;
#47420 = DIRECTION ( 'NONE',  ( 1.000000000000000000, 0.000000000000000000, 0.000000000000000000 ) ) ;
#47421 = ADVANCED_FACE ( 'NONE', ( #43592 ), #43843, .T. ) ;
#47422 =( BOUNDED_CURVE ( )  B_SPLINE_CURVE ( 3, ( #9925, #25583, #41223, #37410 ),
 .UNSPECIFIED., .F., .F. ) 
 B_SPLINE_CURVE_WITH_KNOTS ( ( 4, 4 ),
 ( 1.570796326794896558, 3.141592653589793116 ),
 .UNSPECIFIED. ) 
 CURVE ( )  GEOMETRIC_REPRESENTATION_ITEM ( )  RATIONAL_B_SPLINE_CURVE ( ( 1.000000000000000000, 0.8047378541243649375, 0.8047378541243649375, 1.000000000000000000 ) ) 
 REPRESENTATION_ITEM ( '' )  );
#47423 = CARTESIAN_POINT ( 'NONE',  ( -168.4459734468149463, 0.000000000000000000, 159.0682875569279702 ) ) ;
#47424 = VERTEX_POINT ( 'NONE', #19224 ) ;
#47425 = CARTESIAN_POINT ( 'NONE',  ( 7.896046458374581967, -6.155518428822127852, 6.185594734181547594 ) ) ;
#47426 = EDGE_CURVE ( 'NONE', #10712, #45613, #42950, .T. ) ;
#47427 = VERTEX_POINT ( 'NONE', #519 ) ;
#47428 = DIRECTION ( 'NONE',  ( -1.000000000000000000, -0.000000000000000000, -0.000000000000000000 ) ) ;
#47429 = CARTESIAN_POINT ( 'NONE',  ( -204.9459734468149463, 2.143131898507880377E-16, 122.5682875569279702 ) ) ;
#47430 = ORIENTED_EDGE ( 'NONE', *, *, #27156, .F. ) ;
#47431 = DIRECTION ( 'NONE',  ( 0.000000000000000000, -0.000000000000000000, 1.000000000000000000 ) ) ;
#47432 = EDGE_CURVE ( 'NONE', #38061, #11639, #19500, .T. ) ;
#47433 = VERTEX_POINT ( 'NONE', #4358 ) ;
#47434 = EDGE_CURVE ( 'NONE', #40403, #32098, #5722, .T. ) ;
#47435 = DIRECTION ( 'NONE',  ( 6.203854594147707562E-25, -2.067951531382569187E-25, 1.000000000000000000 ) ) ;
#47436 = CIRCLE ( 'NONE', #37643, 0.5000000000000004441 ) ;
#47437 = CARTESIAN_POINT ( 'NONE',  ( 168.9999999999999716, -268.4999999999999432, -349.9999999999999432 ) ) ;
#47438 = LINE ( 'NONE', #12324, #19685 ) ;
#47439 = CARTESIAN_POINT ( 'NONE',  ( 342.0000000000000568, -178.0000000000000853, 2.999999999999892086 ) ) ;
#47440 = EDGE_CURVE ( 'NONE', #12400, #16599, #9268, .T. ) ;
#47441 = ADVANCED_FACE ( 'NONE', ( #35169 ), #47654, .T. ) ;
#47442 = AXIS2_PLACEMENT_3D ( 'NONE', #33204, #29583, #2620 ) ;
#47443 = ORIENTED_EDGE ( 'NONE', *, *, #30705, .F. ) ;
#47444 = DIRECTION ( 'NONE',  ( -0.000000000000000000, -1.000000000000000000, -0.000000000000000000 ) ) ;
#47445 = AXIS2_PLACEMENT_3D ( 'NONE', #41476, #29933, #22977 ) ;
#47446 = EDGE_CURVE ( 'NONE', #22094, #13764, #15231, .T. ) ;
#47447 = DIRECTION ( 'NONE',  ( 1.000000000000000000, 0.000000000000000000, -4.625929269271635797E-16 ) ) ;
#47448 = VECTOR ( 'NONE', #22256, 1000.000000000000000 ) ;
#47449 = EDGE_CURVE ( 'NONE', #13767, #50570, #31315, .T. ) ;
#47450 = ORIENTED_EDGE ( 'NONE', *, *, #8043, .T. ) ;
#47451 = ORIENTED_EDGE ( 'NONE', *, *, #25511, .T. ) ;
#47453 = CARTESIAN_POINT ( 'NONE',  ( 210.0000000000000568, 2.143131898507880377E-16, -160.9317124430720298 ) ) ;
#47452 = VECTOR ( 'NONE', #16036, 1000.000000000000000 ) ;
#47454 = DIRECTION ( 'NONE',  ( 1.000000000000000000, 0.000000000000000000, 0.000000000000000000 ) ) ;
#47455 =( NAMED_UNIT ( * ) SI_UNIT ( $, .STERADIAN. ) SOLID_ANGLE_UNIT ( ) );
#47456 = CARTESIAN_POINT ( 'NONE',  ( -84.94597344681493212, 1.025126265847089879, -117.4317124430720156 ) ) ;
#47457 = VERTEX_POINT ( 'NONE', #8211 ) ;
#47458 = FACE_OUTER_BOUND ( 'NONE', #21561, .T. ) ;
#47459 = CARTESIAN_POINT ( 'NONE',  ( -385.4922279792746167, 0.000000000000000000, 224.8704663212436117 ) ) ;
#47460 = CARTESIAN_POINT ( 'NONE',  ( 0.000000000000000000, 17.00000000000000000, 0.000000000000000000 ) ) ;
#47461 = EDGE_CURVE ( 'NONE', #14175, #3395, #8462, .T. ) ;
#47462 = CARTESIAN_POINT ( 'NONE',  ( 210.0000000000000568, 0.000000000000000000, -119.1817124430720440 ) ) ;
#47463 = ORIENTED_EDGE ( 'NONE', *, *, #10813, .F. ) ;
#47464 = EDGE_CURVE ( 'NONE', #30248, #40610, #33589, .T. ) ;
#47465 = DIRECTION ( 'NONE',  ( 1.542934785277601468E-15, -0.9749645535258959494, -0.2223603367690620558 ) ) ;
#47466 = ORIENTED_EDGE ( 'NONE', *, *, #45870, .F. ) ;
#47467 = EDGE_CURVE ( 'NONE', #29654, #34586, #12295, .T. ) ;
#47468 = CARTESIAN_POINT ( 'NONE',  ( -46.69597344681494633, 0.000000000000000000, 165.0000000000000000 ) ) ;
#47469 = ORIENTED_EDGE ( 'NONE', *, *, #19952, .F. ) ;
#47470 = DIRECTION ( 'NONE',  ( -1.000000000000000000, 0.000000000000000000, 0.000000000000000000 ) ) ;
#47471 = CARTESIAN_POINT ( 'NONE',  ( 1.040834085586084257E-14, -6.912230148066169200, 5.000000000000000000 ) ) ;
#47472 = B_SPLINE_CURVE_WITH_KNOTS ( 'NONE', 3,
 ( #25292, #28632, #12732, #9392 ),
 .UNSPECIFIED., .F., .F.,
 ( 4, 4 ),
 ( 1.734723475976807094E-18, 8.326314924666556211E-06 ),
 .UNSPECIFIED. ) ;
#47473 = DIRECTION ( 'NONE',  ( -0.000000000000000000, -1.000000000000000000, -0.000000000000000000 ) ) ;
#47474 = CARTESIAN_POINT ( 'NONE',  ( 15.00000000000000000, 13.48684210526315930, -19.37312575500899570 ) ) ;
#47475 = AXIS2_PLACEMENT_3D ( 'NONE', #3330, #45402, #49989 ) ;
#47476 = ORIENTED_EDGE ( 'NONE', *, *, #33700, .T. ) ;
#47477 = ADVANCED_FACE ( 'NONE', ( #44570 ), #24615, .F. ) ;
#47478 = CIRCLE ( 'NONE', #13079, 0.5000000000000004441 ) ;
#47479 = VECTOR ( 'NONE', #21184, 1000.000000000000000 ) ;
#47480 = CARTESIAN_POINT ( 'NONE',  ( 0.8433491450857230065, -0.9182416014173362395, 9.981352469109934233 ) ) ;
#47481 = LINE ( 'NONE', #12359, #24634 ) ;
#47482 = VERTEX_POINT ( 'NONE', #40515 ) ;
#47483 = CARTESIAN_POINT ( 'NONE',  ( 341.9999999999999432, -182.1715728752535597, 357.1715728752534460 ) ) ;
#47484 = CARTESIAN_POINT ( 'NONE',  ( 210.0000000000000568, 0.000000000000000000, -117.4317124430720298 ) ) ;
#47485 = CARTESIAN_POINT ( 'NONE',  ( 359.9999999999999432, 181.0000000000002274, -356.0000000000003411 ) ) ;
#47486 = DIRECTION ( 'NONE',  ( -1.000000000000000000, 0.000000000000000000, -0.000000000000000000 ) ) ;
#47487 = VECTOR ( 'NONE', #6642, 1000.000000000000000 ) ;
#47488 = ORIENTED_EDGE ( 'NONE', *, *, #35320, .F. ) ;
#47489 = VERTEX_POINT ( 'NONE', #5858 ) ;
#47490 = LINE ( 'NONE', #31895, #32512 ) ;
#47491 = EDGE_CURVE ( 'NONE', #46801, #21789, #1109, .T. ) ;
#47492 = VECTOR ( 'NONE', #47234, 1000.000000000000000 ) ;
#47493 = ORIENTED_EDGE ( 'NONE', *, *, #36847, .F. ) ;
#47494 = CARTESIAN_POINT ( 'NONE',  ( 181.0000000000000000, -272.4999999999999432, -349.9999999999999432 ) ) ;
#47495 = LINE ( 'NONE', #33412, #13635 ) ;
#47496 = DIRECTION ( 'NONE',  ( -0.000000000000000000, -0.000000000000000000, -1.000000000000000000 ) ) ;
#47497 = EDGE_CURVE ( 'NONE', #6873, #48314, #13548, .T. ) ;
#47498 = ORIENTED_EDGE ( 'NONE', *, *, #33201, .T. ) ;
#47499 = CARTESIAN_POINT ( 'NONE',  ( 0.000000000000000000, 17.00000000000000000, 0.000000000000000000 ) ) ;
#47500 = ORIENTED_EDGE ( 'NONE', *, *, #16510, .F. ) ;
#47501 = CYLINDRICAL_SURFACE ( 'NONE', #14448, 4.000000000000003553 ) ;
#47502 = CYLINDRICAL_SURFACE ( 'NONE', #42725, 2.000000000000001776 ) ;
#47503 = EDGE_CURVE ( 'NONE', #18068, #20648, #4839, .T. ) ;
#47505 = VERTEX_POINT ( 'NONE', #28955 ) ;
#47504 = ADVANCED_FACE ( 'NONE', ( #36693 ), #45080, .T. ) ;
#47506 = VERTEX_POINT ( 'NONE', #24860 ) ;
#47507 = ORIENTED_EDGE ( 'NONE', *, *, #8016, .F. ) ;
#47508 = DIRECTION ( 'NONE',  ( -7.793956916774525800E-48, 0.000000000000000000, -1.000000000000000000 ) ) ;
#47509 = ADVANCED_FACE ( 'NONE', ( #20498 ), #47909, .F. ) ;
#47510 =( LENGTH_UNIT ( ) NAMED_UNIT ( * ) SI_UNIT ( .MILLI., .METRE. ) );
#47511 = DIRECTION ( 'NONE',  ( -0.000000000000000000, -1.000000000000000000, -0.000000000000000000 ) ) ;
#47512 = EDGE_CURVE ( 'NONE', #29738, #37447, #17408, .T. ) ;
#47513 = ORIENTED_EDGE ( 'NONE', *, *, #17415, .T. ) ;
#47514 = DIRECTION ( 'NONE',  ( -0.000000000000000000, -0.000000000000000000, -1.000000000000000000 ) ) ;
#47516 = ORIENTED_EDGE ( 'NONE', *, *, #25020, .T. ) ;
#47515 = AXIS2_PLACEMENT_3D ( 'NONE', #30226, #17904, #49174 ) ;
#47517 = ADVANCED_FACE ( 'NONE', ( #20749 ), #36430, .T. ) ;
#47518 = CARTESIAN_POINT ( 'NONE',  ( -15.44803555374685189, -6.237487519713257100, -3.546734833711462365 ) ) ;
#47520 = VERTEX_POINT ( 'NONE', #44333 ) ;
#47519 = AXIS2_PLACEMENT_3D ( 'NONE', #34265, #26817, #42449 ) ;
#47521 = DIRECTION ( 'NONE',  ( 0.000000000000000000, -0.000000000000000000, -1.000000000000000000 ) ) ;
#47522 = CARTESIAN_POINT ( 'NONE',  ( 358.3431457505076310, 185.0000000000000284, -360.0000000000002274 ) ) ;
#47523 = DIRECTION ( 'NONE',  ( 0.000000000000000000, 0.000000000000000000, -1.000000000000000000 ) ) ;
#47524 = FACE_OUTER_BOUND ( 'NONE', #22602, .T. ) ;
#47525 = LINE ( 'NONE', #17015, #17643 ) ;
#47526 = FACE_OUTER_BOUND ( 'NONE', #30648, .T. ) ;
#47527 = CARTESIAN_POINT ( 'NONE',  ( 25.61277432017878297, -22.36370378792834757, 7.906207997025717304 ) ) ;
#47528 = ORIENTED_EDGE ( 'NONE', *, *, #46279, .T. ) ;
#47529 = ORIENTED_EDGE ( 'NONE', *, *, #40359, .T. ) ;
#47530 = CARTESIAN_POINT ( 'NONE',  ( -177.4999999999999716, 57.49999999999996447, -9.999999999999973355 ) ) ;
#47531 = CIRCLE ( 'NONE', #27902, 4.000000000000003553 ) ;
#47532 = CARTESIAN_POINT ( 'NONE',  ( -44.34968358615014239, -11.74141640735424019, -9.367992836599951190 ) ) ;
#47533 = SURFACE_STYLE_FILL_AREA ( #9080 ) ;
#47534 = EDGE_CURVE ( 'NONE', #9513, #4058, #25070, .T. ) ;
#47535 = LINE ( 'NONE', #12414, #33569 ) ;
#47536 = VERTEX_POINT ( 'NONE', #13792 ) ;
#47537 = DIRECTION ( 'NONE',  ( 1.333906992743555050E-23, -1.000000000000000000, 0.000000000000000000 ) ) ;
#47538 = CARTESIAN_POINT ( 'NONE',  ( 194.3291528190321742, -1.750000000000009548, -160.2068387089191219 ) ) ;
#47539 = ORIENTED_EDGE ( 'NONE', *, *, #46653, .F. ) ;
#47540 = CARTESIAN_POINT ( 'NONE',  ( 340.0000000000000000, 175.0000000000000284, -94.00000000000019895 ) ) ;
#47541 = FACE_OUTER_BOUND ( 'NONE', #27622, .T. ) ;
#47542 = DIRECTION ( 'NONE',  ( 2.958228394578793832E-31, 0.000000000000000000, 1.000000000000000000 ) ) ;
#47543 = VERTEX_POINT ( 'NONE', #21011 ) ;
#47544 = ORIENTED_EDGE ( 'NONE', *, *, #18808, .F. ) ;
#47545 = CARTESIAN_POINT ( 'NONE',  ( 155.0540265531850537, 1.025126265847089879, 82.56828755692798438 ) ) ;
#47546 = CARTESIAN_POINT ( 'NONE',  ( 154.3291528190321458, 1.750000000000010214, 79.79316129108087807 ) ) ;
#47547 = VECTOR ( 'NONE', #25617, 1000.000000000000000 ) ;
#47548 = ORIENTED_EDGE ( 'NONE', *, *, #40051, .T. ) ;
#47549 = ORIENTED_EDGE ( 'NONE', *, *, #50536, .F. ) ;
#47550 = CARTESIAN_POINT ( 'NONE',  ( -22.82242230425432439, -2.816136035261162185, 230.0000000000000000 ) ) ;
#47551 = CARTESIAN_POINT ( 'NONE',  ( -124.9459734468149463, 2.143131898507847836E-16, -157.4317124430720582 ) ) ;
#47552 = CARTESIAN_POINT ( 'NONE',  ( 151.5540265531850537, 1.025126265847089657, 79.06828755692797017 ) ) ;
#47553 = CARTESIAN_POINT ( 'NONE',  ( 349.9999999999999432, -180.9999999999999716, 343.9999999999997726 ) ) ;
#47554 = ORIENTED_EDGE ( 'NONE', *, *, #50091, .F. ) ;
#47555 = ORIENTED_EDGE ( 'NONE', *, *, #5552, .T. ) ;
#47556 = ORIENTED_EDGE ( 'NONE', *, *, #19040, .F. ) ;
#47557 = AXIS2_PLACEMENT_3D ( 'NONE', #38120, #14751, #45010 ) ;
#47558 = B_SPLINE_CURVE_WITH_KNOTS ( 'NONE', 3,
 ( #28665, #25319, #47616, #12502 ),
 .UNSPECIFIED., .F., .F.,
 ( 4, 4 ),
 ( 0.0009679537044798808103, 0.001281751046851268335 ),
 .UNSPECIFIED. ) ;
#47559 = CARTESIAN_POINT ( 'NONE',  ( -16.76006782980216059, 2.050259795448645228, 9.178419661560148768 ) ) ;
#47560 = ORIENTED_EDGE ( 'NONE', *, *, #45653, .F. ) ;
#47561 = EDGE_CURVE ( 'NONE', #19563, #47056, #32826, .T. ) ;
#47562 = EDGE_CURVE ( 'NONE', #24104, #47298, #7684, .T. ) ;
#47563 = LINE ( 'NONE', #43744, #18063 ) ;
#47564 = VERTEX_POINT ( 'NONE', #48158 ) ;
#47565 = VERTEX_POINT ( 'NONE', #13045 ) ;
#47566 = DIRECTION ( 'NONE',  ( 1.000000000000000000, 0.000000000000000000, 0.000000000000000000 ) ) ;
#47567 = CARTESIAN_POINT ( 'NONE',  ( -31.44259251615275019, -38.95901822126145220, -9.367992836599954742 ) ) ;
#47568 =( BOUNDED_CURVE ( )  B_SPLINE_CURVE ( 3, ( #49557, #25011, #2166, #10367 ),
 .UNSPECIFIED., .F., .F. ) 
 B_SPLINE_CURVE_WITH_KNOTS ( ( 4, 4 ),
 ( 3.141592653589793116, 4.712388980384689674 ),
 .UNSPECIFIED. ) 
 CURVE ( )  GEOMETRIC_REPRESENTATION_ITEM ( )  RATIONAL_B_SPLINE_CURVE ( ( 1.000000000000000000, 0.8047378541243649375, 0.8047378541243649375, 1.000000000000000000 ) ) 
 REPRESENTATION_ITEM ( '' )  );
#47569 = CARTESIAN_POINT ( 'NONE',  ( 112.2789002873379758, 1.749999999999996891, -40.20683870891911482 ) ) ;
#47570 = EDGE_CURVE ( 'NONE', #20193, #27159, #28037, .T. ) ;
#47571 = ORIENTED_EDGE ( 'NONE', *, *, #48868, .T. ) ;
#47573 = ORIENTED_EDGE ( 'NONE', *, *, #29322, .F. ) ;
#47572 = B_SPLINE_CURVE_WITH_KNOTS ( 'NONE', 3,
 ( #37319, #1888, #17027, #36303 ),
 .UNSPECIFIED., .F., .F.,
 ( 4, 4 ),
 ( 0.0008678710649527057426, 0.007006382029922212512 ),
 .UNSPECIFIED. ) ;
#47574 = ADVANCED_FACE ( 'NONE', ( #9453 ), #5597, .T. ) ;
#47575 = CARTESIAN_POINT ( 'NONE',  ( 33.30402655318503946, -1.750000000000010658, 80.81828755692798438 ) ) ;
#47576 = CARTESIAN_POINT ( 'NONE',  ( 210.0000000000000568, 0.000000000000000000, 2.568287556927987048 ) ) ;
#47577 = EDGE_LOOP ( 'NONE', ( #754, #36337, #3646, #32313 ) ) ;
#47578 = EDGE_CURVE ( 'NONE', #12301, #24963, #33076, .T. ) ;
#47579 = DIRECTION ( 'NONE',  ( -1.000000000000000000, -0.000000000000000000, -0.000000000000000000 ) ) ;
#47580 = DIRECTION ( 'NONE',  ( 0.000000000000000000, 0.000000000000000000, 1.000000000000000000 ) ) ;
#47581 = DIRECTION ( 'NONE',  ( -0.000000000000000000, -1.000000000000000000, -0.000000000000000000 ) ) ;
#47582 = LINE ( 'NONE', #11974, #27384 ) ;
#47583 = ORIENTED_EDGE ( 'NONE', *, *, #934, .T. ) ;
#47584 = DIRECTION ( 'NONE',  ( 0.000000000000000000, 0.000000000000000000, -1.000000000000000000 ) ) ;
#47585 = CARTESIAN_POINT ( 'NONE',  ( 193.3040265531851105, 1.750000000000010658, -119.1817124430720440 ) ) ;
#47586 = EDGE_CURVE ( 'NONE', #4462, #38061, #9332, .T. ) ;
#47587 = VECTOR ( 'NONE', #42457, 1000.000000000000000 ) ;
#47588 = LINE ( 'NONE', #11980, #12390 ) ;
#47589 =( REPRESENTATION_RELATIONSHIP ('NONE','NONE', #45699, #41838 ) REPRESENTATION_RELATIONSHIP_WITH_TRANSFORMATION ( #33372 )SHAPE_REPRESENTATION_RELATIONSHIP( ) );
#47590 = DIRECTION ( 'NONE',  ( 0.000000000000000000, -1.604368532695312981E-16, -1.000000000000000000 ) ) ;
#47591 = VECTOR ( 'NONE', #942, 1000.000000000000000 ) ;
#47592 = DIRECTION ( 'NONE',  ( 1.000000000000000000, 0.000000000000000000, 0.000000000000000000 ) ) ;
#47593 = CARTESIAN_POINT ( 'NONE',  ( -45.67084718096785423, -1.750000000000010436, 79.79316129108087807 ) ) ;
#47594 = ORIENTED_EDGE ( 'NONE', *, *, #31177, .F. ) ;
#47595 = FACE_OUTER_BOUND ( 'NONE', #13175, .T. ) ;
#47596 = LINE ( 'NONE', #28144, #27892 ) ;
#47597 = EDGE_LOOP ( 'NONE', ( #26511, #48682, #20967, #161, #29617, #35817 ) ) ;
#47598 = CARTESIAN_POINT ( 'NONE',  ( -6.695973446814940111, -1.750000000000024203, -119.1817124430720440 ) ) ;
#47599 = FACE_OUTER_BOUND ( 'NONE', #43334, .T. ) ;
#47600 = CARTESIAN_POINT ( 'NONE',  ( 33.30402655318503946, -1.750000000000010658, -79.18171244307201562 ) ) ;
#47601 = ORIENTED_EDGE ( 'NONE', *, *, #6428, .T. ) ;
#47602 = CYLINDRICAL_SURFACE ( 'NONE', #27369, 1.750000000000008438 ) ;
#47603 = ORIENTED_EDGE ( 'NONE', *, *, #2916, .F. ) ;
#47604 = VERTEX_POINT ( 'NONE', #6110 ) ;
#47605 = LINE ( 'NONE', #12486, #17693 ) ;
#47606 = EDGE_CURVE ( 'NONE', #4486, #40841, #32268, .T. ) ;
#47607 = CARTESIAN_POINT ( 'NONE',  ( -167.7210997126620384, -1.750000000000010214, -80.20683870891910772 ) ) ;
#47608 = VERTEX_POINT ( 'NONE', #26624 ) ;
#47609 = CARTESIAN_POINT ( 'NONE',  ( -1.305659100530649264, 0.2632760600738136558, 9.951893257059998277 ) ) ;
#47610 = PLANE ( 'NONE',  #10982 ) ;
#47611 = ORIENTED_EDGE ( 'NONE', *, *, #31783, .T. ) ;
#47612 = DIRECTION ( 'NONE',  ( -1.000000000000000000, -0.000000000000000000, -0.000000000000000000 ) ) ;
#47613 = VERTEX_POINT ( 'NONE', #22768 ) ;
#47614 = CARTESIAN_POINT ( 'NONE',  ( -204.9459734468148895, 1.025126265847089657, 119.0682875569279560 ) ) ;
#47615 = DIRECTION ( 'NONE',  ( -1.000000000000000000, 0.000000000000000000, 0.000000000000000000 ) ) ;
#47616 = CARTESIAN_POINT ( 'NONE',  ( 0.3618874479333703542, -1.945951947734774645, 9.897807938190485544 ) ) ;
#47617 = ORIENTED_EDGE ( 'NONE', *, *, #26257, .T. ) ;
#47618 = DIRECTION ( 'NONE',  ( -1.000000000000000000, -0.000000000000000000, -0.000000000000000000 ) ) ;
#47619 = VECTOR ( 'NONE', #36477, 1000.000000000000000 ) ;
#47620 = CARTESIAN_POINT ( 'NONE',  ( -14.49999999999999822, 12.98684210526315930, -19.37312575500900280 ) ) ;
#47621 = VERTEX_POINT ( 'NONE', #7129 ) ;
#47622 = EDGE_LOOP ( 'NONE', ( #5156, #3531, #26166, #49532 ) ) ;
#47623 = ORIENTED_EDGE ( 'NONE', *, *, #27370, .F. ) ;
#47624 = DIRECTION ( 'NONE',  ( 0.000000000000000000, -1.000000000000000000, 0.000000000000000000 ) ) ;
#47625 = CARTESIAN_POINT ( 'NONE',  ( 73.30402655318508209, -1.750000000000010658, -119.1817124430720440 ) ) ;
#47626 = VECTOR ( 'NONE', #24432, 1000.000000000000000 ) ;
#47627 = ORIENTED_EDGE ( 'NONE', *, *, #8457, .T. ) ;
#47628 = CARTESIAN_POINT ( 'NONE',  ( -46.69597344681494633, -1.750000000000010658, 120.8182875569279702 ) ) ;
#47629 = CARTESIAN_POINT ( 'NONE',  ( 181.0000000000000000, -174.9999999999999716, -344.0000000000001137 ) ) ;
#47630 = EDGE_CURVE ( 'NONE', #20716, #21514, #5939, .T. ) ;
#47631 = CARTESIAN_POINT ( 'NONE',  ( -48.44597344681496054, -1.025126265847089213, 159.0682875569279418 ) ) ;
#47632 = DIRECTION ( 'NONE',  ( -0.000000000000000000, 1.000000000000000000, -1.604368532695312981E-16 ) ) ;
#47633 = CARTESIAN_POINT ( 'NONE',  ( -166.6959734468149463, -1.750000000000009992, -159.1817124430720298 ) ) ;
#47635 = ADVANCED_FACE ( 'NONE', ( #41761 ), #18153, .T. ) ;
#47634 = CARTESIAN_POINT ( 'NONE',  ( 1.962712821592840662, 1.022159834731142691, 9.881002359080275355 ) ) ;
#47636 = LINE ( 'NONE', #28685, #16025 ) ;
#47637 = FACE_OUTER_BOUND ( 'NONE', #45280, .T. ) ;
#47638 = DIRECTION ( 'NONE',  ( 0.000000000000000000, 1.000000000000000000, 1.544785076050074834E-48 ) ) ;
#47639 = CARTESIAN_POINT ( 'NONE',  ( -6.695973446814940111, 0.000000000000000000, 165.0000000000000000 ) ) ;
#47640 =( BOUNDED_CURVE ( )  B_SPLINE_CURVE ( 3, ( #4618, #20263, #32072, #27461 ),
 .UNSPECIFIED., .F., .F. ) 
 B_SPLINE_CURVE_WITH_KNOTS ( ( 4, 4 ),
 ( 1.570796326794896558, 3.141592653589793116 ),
 .UNSPECIFIED. ) 
 CURVE ( )  GEOMETRIC_REPRESENTATION_ITEM ( )  RATIONAL_B_SPLINE_CURVE ( ( 1.000000000000000000, 0.8047378541243649375, 0.8047378541243649375, 1.000000000000000000 ) ) 
 REPRESENTATION_ITEM ( '' )  );
#47641 = FACE_OUTER_BOUND ( 'NONE', #12926, .T. ) ;
#47642 = CARTESIAN_POINT ( 'NONE',  ( -0.8155877869437639927, -0.9072449372115535260, 9.963925895596188909 ) ) ;
#47643 = ORIENTED_EDGE ( 'NONE', *, *, #12105, .F. ) ;
#47644 = DIRECTION ( 'NONE',  ( 0.000000000000000000, 0.000000000000000000, 1.000000000000000000 ) ) ;
#47645 = CARTESIAN_POINT ( 'NONE',  ( 214.9999999999999432, 164.9999999999999716, 500.0000000000000000 ) ) ;
#47646 = LINE ( 'NONE', #5344, #32408 ) ;
#47647 = CARTESIAN_POINT ( 'NONE',  ( 28.96803024440893992, 18.11533787072037072, 7.455576670931136185 ) ) ;
#47648 = EDGE_LOOP ( 'NONE', ( #37266, #7237, #5038, #28245 ) ) ;
#47649 = CARTESIAN_POINT ( 'NONE',  ( -0.9989200098981521059, -1.123829893718962802, 9.927319414211225990 ) ) ;
#47650 = VECTOR ( 'NONE', #39534, 1000.000000000000000 ) ;
#47651 = LINE ( 'NONE', #20746, #27037 ) ;
#47652 = ORIENTED_EDGE ( 'NONE', *, *, #35010, .F. ) ;
#47653 = LINE ( 'NONE', #24368, #46737 ) ;
#47654 = CYLINDRICAL_SURFACE ( 'NONE', #1909, 1.750000000000010214 ) ;
#47655 = DIRECTION ( 'NONE',  ( 0.000000000000000000, -1.000000000000000000, 8.021842663476564905E-17 ) ) ;
#47656 = ORIENTED_EDGE ( 'NONE', *, *, #6542, .F. ) ;
#47657 = DIRECTION ( 'NONE',  ( -0.000000000000000000, -0.000000000000000000, -1.000000000000000000 ) ) ;
#47658 = ORIENTED_EDGE ( 'NONE', *, *, #13922, .F. ) ;
#47659 = VERTEX_POINT ( 'NONE', #33831 ) ;
#47660 = EDGE_CURVE ( 'NONE', #28177, #19656, #15075, .T. ) ;
#47661 = ORIENTED_EDGE ( 'NONE', *, *, #11528, .F. ) ;
#47662 = DIRECTION ( 'NONE',  ( -0.000000000000000000, -0.000000000000000000, 1.000000000000000000 ) ) ;
#47663 = LINE ( 'NONE', #42833, #9301 ) ;
#47664 = ORIENTED_EDGE ( 'NONE', *, *, #5838, .T. ) ;
#47665 = CARTESIAN_POINT ( 'NONE',  ( 359.9999999999999432, -181.0000000000001421, -349.9999999999998863 ) ) ;
#47666 = CYLINDRICAL_SURFACE ( 'NONE', #10317, 1.750000000000001554 ) ;
#47667 = CARTESIAN_POINT ( 'NONE',  ( -24.87155650802101903, 38.55075836233108788, -9.367992836599951190 ) ) ;
#47668 = AXIS2_PLACEMENT_3D ( 'NONE', #39860, #24198, #1350 ) ;
#47669 = CARTESIAN_POINT ( 'NONE',  ( -0.3370904143228943828, -0.2449105217885308716, -10.00000000000000000 ) ) ;
#47670 = EDGE_LOOP ( 'NONE', ( #3695, #23222, #13458, #20426 ) ) ;
#47671 = DIRECTION ( 'NONE',  ( 0.000000000000000000, -3.186989995019654210E-49, -1.000000000000000000 ) ) ;
#47672 = ORIENTED_EDGE ( 'NONE', *, *, #28027, .F. ) ;
#47673 = CARTESIAN_POINT ( 'NONE',  ( 240.0000000000000000, -175.0000000000000000, 474.9999999999998863 ) ) ;
#47674 = CYLINDRICAL_SURFACE ( 'NONE', #8955, 1.750000000000015543 ) ;
#47675 = MECHANICAL_DESIGN_GEOMETRIC_PRESENTATION_REPRESENTATION (  '', ( #35443 ), #37090 ) ;
#47676 = EDGE_LOOP ( 'NONE', ( #23421, #11560, #477, #18012 ) ) ;
#47677 = CARTESIAN_POINT ( 'NONE',  ( -5.670847180967843570, 1.750000000000023537, 79.79316129108087807 ) ) ;
#47678 = VECTOR ( 'NONE', #38607, 1000.000000000000000 ) ;
#47679 = DIRECTION ( 'NONE',  ( 0.000000000000000000, 3.186989995019654210E-49, 1.000000000000000000 ) ) ;
#47680 = ORIENTED_EDGE ( 'NONE', *, *, #29595, .F. ) ;
#47681 = AXIS2_PLACEMENT_3D ( 'NONE', #31626, #47215, #12114 ) ;
#47682 = CARTESIAN_POINT ( 'NONE',  ( -14.99999999999906919, 17.00000000000000000, 0.000000000000000000 ) ) ;
#47683 = CARTESIAN_POINT ( 'NONE',  ( -24.47767542868268364, 23.18653802921800278, 8.807470649214879543 ) ) ;
#47684 = DIRECTION ( 'NONE',  ( 0.000000000000000000, 0.000000000000000000, -1.000000000000000000 ) ) ;
#47685 = CARTESIAN_POINT ( 'NONE',  ( 75.05402655318509630, -1.025126265847089435, -77.43171244307200141 ) ) ;
#47686 = CIRCLE ( 'NONE', #15796, 1.750000000000001554 ) ;
#47687 = ORIENTED_EDGE ( 'NONE', *, *, #14539, .T. ) ;
#47688 = FACE_OUTER_BOUND ( 'NONE', #40599, .T. ) ;
#47690 = EDGE_CURVE ( 'NONE', #46923, #28634, #38440, .T. ) ;
#47689 = DIRECTION ( 'NONE',  ( 1.132880637372608740E-16, 4.718402560806925739E-50, 1.000000000000000000 ) ) ;
#47691 = CARTESIAN_POINT ( 'NONE',  ( 45.21167770612395742, 22.65616271077811206, 7.906207997025717304 ) ) ;
#47692 = ORIENTED_EDGE ( 'NONE', *, *, #13150, .T. ) ;
#47693 = B_SPLINE_CURVE_WITH_KNOTS ( 'NONE', 3,
 ( #7904, #24313, #31252, #11736 ),
 .UNSPECIFIED., .F., .F.,
 ( 4, 4 ),
 ( 3.066586833366748373E-19, 0.0002708531562719474124 ),
 .UNSPECIFIED. ) ;
#47694 = ORIENTED_EDGE ( 'NONE', *, *, #41286, .F. ) ;
#47695 = APPLICATION_PROTOCOL_DEFINITION ( 'draft international standard', 'automotive_design', 1998, #1417 ) ;
#47696 = CARTESIAN_POINT ( 'NONE',  ( -7.721099712662037540, 1.750000000000023315, -38.15658617722493062 ) ) ;
#47697 =( BOUNDED_CURVE ( )  B_SPLINE_CURVE ( 3, ( #43326, #31811, #23333, #748 ),
 .UNSPECIFIED., .F., .F. ) 
 B_SPLINE_CURVE_WITH_KNOTS ( ( 4, 4 ),
 ( 0.000000000000000000, 1.570796326794896558 ),
 .UNSPECIFIED. ) 
 CURVE ( )  GEOMETRIC_REPRESENTATION_ITEM ( )  RATIONAL_B_SPLINE_CURVE ( ( 1.000000000000000000, 0.8047378541243649375, 0.8047378541243649375, 1.000000000000000000 ) ) 
 REPRESENTATION_ITEM ( '' )  );
#47698 = CARTESIAN_POINT ( 'NONE',  ( 356.0000000000001137, 183.0000000000000284, 357.9999999999998295 ) ) ;
#47699 = CARTESIAN_POINT ( 'NONE',  ( -0.4400426740873942810, 2.015233077865125733, 9.886433018048068178 ) ) ;
#47700 = CARTESIAN_POINT ( 'NONE',  ( 358.0000000000000000, 169.0000000000000000, -344.0000000000001137 ) ) ;
#47701 = DIRECTION ( 'NONE',  ( 0.000000000000000000, 0.000000000000000000, -1.000000000000000000 ) ) ;
#47702 = ORIENTED_EDGE ( 'NONE', *, *, #19625, .F. ) ;
#47703 = CARTESIAN_POINT ( 'NONE',  ( 71.55402655318505367, 0.000000000000000000, -80.93171244307204404 ) ) ;
#47704 = EDGE_CURVE ( 'NONE', #35493, #2551, #45823, .T. ) ;
#47705 =( BOUNDED_CURVE ( )  B_SPLINE_CURVE ( 3, ( #24687, #44895, #40332, #36757 ),
 .UNSPECIFIED., .F., .F. ) 
 B_SPLINE_CURVE_WITH_KNOTS ( ( 4, 4 ),
 ( 0.000000000000000000, 1.570796326794896558 ),
 .UNSPECIFIED. ) 
 CURVE ( )  GEOMETRIC_REPRESENTATION_ITEM ( )  RATIONAL_B_SPLINE_CURVE ( ( 1.000000000000000000, 0.8047378541243649375, 0.8047378541243649375, 1.000000000000000000 ) ) 
 REPRESENTATION_ITEM ( '' )  );
#47706 = VECTOR ( 'NONE', #11312, 1000.000000000000000 ) ;
#47707 = LINE ( 'NONE', #12592, #46593 ) ;
#47708 = CARTESIAN_POINT ( 'NONE',  ( 210.0000000000000568, 0.000000000000000000, 0.8182875569279768335 ) ) ;
#47709 = CARTESIAN_POINT ( 'NONE',  ( 154.3291528190321458, -1.750000000000010436, -80.20683870891910772 ) ) ;
#47710 = EDGE_CURVE ( 'NONE', #4446, #46038, #6021, .T. ) ;
#47711 = VERTEX_POINT ( 'NONE', #22007 ) ;
#47712 = CARTESIAN_POINT ( 'NONE',  ( 0.000000000000000000, 0.000000000000000000, 10.00000000000000000 ) ) ;
#47713 = ORIENTED_EDGE ( 'NONE', *, *, #47461, .F. ) ;
#47714 = FACE_OUTER_BOUND ( 'NONE', #9803, .T. ) ;
#47715 = COLOUR_RGB ( '',0.7921568627450980005, 0.8196078431372548767, 0.9333333333333333481 ) ;
#47716 = ORIENTED_EDGE ( 'NONE', *, *, #2492, .F. ) ;
#47717 = CARTESIAN_POINT ( 'NONE',  ( 73.30402655318508209, 1.750000000000009992, -159.1817124430720298 ) ) ;
#47718 = CARTESIAN_POINT ( 'NONE',  ( 181.0000000000000000, -164.9999999999999432, -356.0000000000001705 ) ) ;
#47719 = EDGE_CURVE ( 'NONE', #1381, #45635, #9675, .T. ) ;
#47720 = LINE ( 'NONE', #29525, #15869 ) ;
#47721 = CARTESIAN_POINT ( 'NONE',  ( 210.0000000000000568, 0.000000000000000000, -159.1817124430720298 ) ) ;
#47722 = EDGE_CURVE ( 'NONE', #3623, #14442, #3255, .T. ) ;
#47723 = ORIENTED_EDGE ( 'NONE', *, *, #41816, .T. ) ;
#47724 = AXIS2_PLACEMENT_3D ( 'NONE', #16335, #46834, #8391 ) ;
#47725 = ADVANCED_FACE ( 'NONE', ( #33574 ), #30471, .F. ) ;
#47726 = EDGE_CURVE ( 'NONE', #44375, #38075, #29974, .T. ) ;
#47727 = DIRECTION ( 'NONE',  ( -1.000000000000000000, -0.000000000000000000, -0.000000000000000000 ) ) ;
#47728 = VECTOR ( 'NONE', #14071, 1000.000000000000000 ) ;
#47729 = DIRECTION ( 'NONE',  ( 0.000000000000000000, 0.000000000000000000, 1.000000000000000000 ) ) ;
#47730 = ORIENTED_EDGE ( 'NONE', *, *, #28054, .T. ) ;
#47731 = PLANE ( 'NONE',  #20560 ) ;
#47732 = DIRECTION ( 'NONE',  ( 0.000000000000000000, 0.000000000000000000, 1.000000000000000000 ) ) ;
#47733 = DIRECTION ( 'NONE',  ( 0.000000000000000000, 0.000000000000000000, -1.000000000000000000 ) ) ;
#47734 = VERTEX_POINT ( 'NONE', #42270 ) ;
#47735 = EDGE_LOOP ( 'NONE', ( #31023, #4206, #26396, #5602, #7819 ) ) ;
#47736 = CARTESIAN_POINT ( 'NONE',  ( -0.3656201545664206076, 2.182515578491385000, 9.881002359080270026 ) ) ;
#47737 = VERTEX_POINT ( 'NONE', #38198 ) ;
#47738 = LINE ( 'NONE', #48240, #12664 ) ;
#47739 = CARTESIAN_POINT ( 'NONE',  ( -582.5000000000000000, 57.49999999999996447, -58.60000000000003695 ) ) ;
#47740 = ORIENTED_EDGE ( 'NONE', *, *, #15062, .T. ) ;
#47741 = CARTESIAN_POINT ( 'NONE',  ( 0.2050626648100478400, -1.807624707196173519, 9.903764339332001398 ) ) ;
#47742 = EDGE_CURVE ( 'NONE', #10525, #28510, #20758, .T. ) ;
#47743 = DIRECTION ( 'NONE',  ( 6.203854594147707562E-25, -2.067951531382569187E-25, 1.000000000000000000 ) ) ;
#47744 = CARTESIAN_POINT ( 'NONE',  ( -4.672045878990125800, 33.19353511768168374, 1.847720168420772691 ) ) ;
#47745 = EDGE_CURVE ( 'NONE', #11842, #19947, #30587, .T. ) ;
#47746 = ORIENTED_EDGE ( 'NONE', *, *, #13920, .F. ) ;
#47747 = ADVANCED_FACE ( 'NONE', ( #3781 ), #11480, .F. ) ;
#47748 = ORIENTED_EDGE ( 'NONE', *, *, #32192, .T. ) ;
#47749 = VECTOR ( 'NONE', #37386, 1000.000000000000000 ) ;
#47750 = VERTEX_POINT ( 'NONE', #35863 ) ;
#47751 = CARTESIAN_POINT ( 'NONE',  ( 210.0000000000000568, 2.143131898507880377E-16, -0.9317124430720331585 ) ) ;
#47752 = ADVANCED_FACE ( 'NONE', ( #35366 ), #199, .T. ) ;
#47753 = CARTESIAN_POINT ( 'NONE',  ( 85.00000000000090949, 17.00000000000000000, 0.000000000000000000 ) ) ;
#47754 = ORIENTED_EDGE ( 'NONE', *, *, #12283, .T. ) ;
#47755 = CARTESIAN_POINT ( 'NONE',  ( 192.2789002873380184, 1.750000000000009548, -0.2068387089191121020 ) ) ;
#47756 = ORIENTED_EDGE ( 'NONE', *, *, #19386, .T. ) ;
#47757 = B_SPLINE_CURVE_WITH_KNOTS ( 'NONE', 3,
 ( #33559, #26093, #6596, #30196, #48890, #6855 ),
 .UNSPECIFIED., .F., .F.,
 ( 4, 2, 4 ),
 ( 2.453269466693398698E-18, 0.009877169331704828414, 0.01975433866340965683 ),
 .UNSPECIFIED. ) ;
#47758 = ADVANCED_FACE ( 'NONE', ( #19161, #7639 ), #39706, .T. ) ;
#47759 = CARTESIAN_POINT ( 'NONE',  ( -14.86945752723352498, -7.944783388878907004, 2.590526750877053086 ) ) ;
#47760 = ORIENTED_EDGE ( 'NONE', *, *, #18145, .F. ) ;
#47761 = DIRECTION ( 'NONE',  ( 0.000000000000000000, 1.577721810442023611E-30, 0.9999999999999998890 ) ) ;
#47762 = FACE_OUTER_BOUND ( 'NONE', #30109, .T. ) ;
#47763 = LINE ( 'NONE', #16762, #16212 ) ;
#47764 = FACE_OUTER_BOUND ( 'NONE', #1138, .T. ) ;
#47765 = VECTOR ( 'NONE', #1317, 1000.000000000000000 ) ;
#47766 = DIRECTION ( 'NONE',  ( -1.000000000000000000, -0.000000000000000000, -0.000000000000000000 ) ) ;
#47767 = LINE ( 'NONE', #43953, #14995 ) ;
#47768 = VERTEX_POINT ( 'NONE', #23012 ) ;
#47769 = B_SPLINE_CURVE_WITH_KNOTS ( 'NONE', 3,
 ( #31950, #4980, #32452, #27594 ),
 .UNSPECIFIED., .F., .F.,
 ( 4, 4 ),
 ( 0.002217981418793440844, 0.002368422649471284280 ),
 .UNSPECIFIED. ) ;
#47770 = LINE ( 'NONE', #36797, #28837 ) ;
#47771 = B_SPLINE_SURFACE_WITH_KNOTS ( 'NONE', 3, 3, ( 
 ( #45814, #2248, #29448, #14549 ),
 ( #49660, #6605, #17886, #5850 ),
 ( #10701, #21493, #10207, #33564 ),
 ( #45578, #33317, #30462, #33819 ) ),
 .UNSPECIFIED., .F., .F., .F.,
 ( 4, 4 ),
 ( 4, 4 ),
 ( 0.000000000000000000, 1.000000000000000000 ),
 ( 0.000000000000000000, 1.000000000000000000 ),
 .UNSPECIFIED. ) ;
#47772 = CARTESIAN_POINT ( 'NONE',  ( 151.5540265531850537, -1.025126265847089213, 159.0682875569279418 ) ) ;
#47773 = CARTESIAN_POINT ( 'NONE',  ( 113.3040265531850537, 0.000000000000000000, 165.0000000000000000 ) ) ;
#47774 = AXIS2_PLACEMENT_3D ( 'NONE', #32412, #40363, #13152 ) ;
#47775 =( NAMED_UNIT ( * ) SI_UNIT ( $, .STERADIAN. ) SOLID_ANGLE_UNIT ( ) );
#47776 = EDGE_LOOP ( 'NONE', ( #35496, #32082, #7379, #45734, #37257, #15945 ) ) ;
#47777 = ADVANCED_FACE ( 'NONE', ( #38690 ), #31249, .F. ) ;
#47778 = FACE_OUTER_BOUND ( 'NONE', #46021, .T. ) ;
#47779 = ORIENTED_EDGE ( 'NONE', *, *, #5136, .F. ) ;
#47780 = CARTESIAN_POINT ( 'NONE',  ( -45.88383801556796016, 6.205508426777106123, 7.455576670931137073 ) ) ;
#47781 = LINE ( 'NONE', #14441, #24719 ) ;
#47782 = ADVANCED_FACE ( 'NONE', ( #15836, #43019 ), #19429, .T. ) ;
#47783 = ORIENTED_EDGE ( 'NONE', *, *, #16785, .T. ) ;
#47784 = EDGE_CURVE ( 'NONE', #23962, #34772, #690, .T. ) ;
#47785 = EDGE_CURVE ( 'NONE', #15688, #23492, #47343, .T. ) ;
#47786 = FACE_OUTER_BOUND ( 'NONE', #19292, .T. ) ;
#47787 = CARTESIAN_POINT ( 'NONE',  ( -6.695973446814940111, 1.750000000000023315, 160.8182875569279702 ) ) ;
#47788 = VECTOR ( 'NONE', #33586, 1000.000000000000000 ) ;
#47789 = CARTESIAN_POINT ( 'NONE',  ( -47.87295225382221275, -14.46560184742400423, -2.408242355805840784 ) ) ;
#47790 = ADVANCED_FACE ( 'NONE', ( #24053 ), #38949, .F. ) ;
#47791 = CARTESIAN_POINT ( 'NONE',  ( 49.46074318306830975, -9.578883844006833570, 8.807470649214879543 ) ) ;
#47792 = CIRCLE ( 'NONE', #44539, 3.749999999999975575 ) ;
#47793 = EDGE_CURVE ( 'NONE', #13192, #3794, #27388, .T. ) ;
#47794 = ORIENTED_EDGE ( 'NONE', *, *, #4239, .F. ) ;
#47795 = EDGE_LOOP ( 'NONE', ( #8922, #9245, #44825, #27724, #14020, #32374 ) ) ;
#47796 = CARTESIAN_POINT ( 'NONE',  ( 356.0000000000000568, 165.0000000000000000, -94.00000000000019895 ) ) ;
#47797 = CIRCLE ( 'NONE', #42107, 5.000000000000000888 ) ;
#47798 = CARTESIAN_POINT ( 'NONE',  ( -0.3862712429686729343, -1.188820645368946050, -3.333333333333333481 ) ) ;
#47799 = AXIS2_PLACEMENT_3D ( 'NONE', #23060, #38239, #34375 ) ;
#47800 = ORIENTED_EDGE ( 'NONE', *, *, #778, .T. ) ;
#47801 = ORIENTED_EDGE ( 'NONE', *, *, #19007, .F. ) ;
#47802 = DIRECTION ( 'NONE',  ( 0.000000000000000000, 2.537652627714642000E-15, 1.000000000000000000 ) ) ;
#47803 = CARTESIAN_POINT ( 'NONE',  ( 71.55402655318505367, 1.025126265847089435, 82.56828755692798438 ) ) ;
#47804 = CARTESIAN_POINT ( 'NONE',  ( 14.29087950072012170, 9.652079258044652832, 8.727788335465566760 ) ) ;
#47805 = CARTESIAN_POINT ( 'NONE',  ( 112.2789002873379758, -1.749999999999996891, -120.2068387089191219 ) ) ;
#47806 = VERTEX_POINT ( 'NONE', #8146 ) ;
#47807 = VERTEX_POINT ( 'NONE', #50430 ) ;
#47808 = ORIENTED_EDGE ( 'NONE', *, *, #20260, .T. ) ;
#47809 = PLANE ( 'NONE',  #13559 ) ;
#47810 = VECTOR ( 'NONE', #17074, 1000.000000000000000 ) ;
#47811 = ADVANCED_FACE ( 'NONE', ( #7900 ), #34851, .T. ) ;
#47812 = CARTESIAN_POINT ( 'NONE',  ( -128.4459734468149463, -1.025126265847081442, 159.0682875569279418 ) ) ;
#47813 = EDGE_LOOP ( 'NONE', ( #39614, #11627, #42106, #23601 ) ) ;
#47814 = ORIENTED_EDGE ( 'NONE', *, *, #29081, .T. ) ;
#47815 = CARTESIAN_POINT ( 'NONE',  ( -6.695973446814940111, -1.750000000000024203, 80.81828755692798438 ) ) ;
#47816 = ORIENTED_EDGE ( 'NONE', *, *, #34594, .T. ) ;
#47817 = PRODUCT_DEFINITION ( 'UNKNOWN', '', #34038, #613 ) ;
#47818 = EDGE_LOOP ( 'NONE', ( #1203, #7345, #37816, #41634 ) ) ;
#47819 = DIRECTION ( 'NONE',  ( 1.000000000000000000, -0.000000000000000000, -0.000000000000000000 ) ) ;
#47820 = DIRECTION ( 'NONE',  ( 4.758098676964954489E-16, 1.000000000000000000, 1.751623080406021339E-46 ) ) ;
#47821 = ORIENTED_EDGE ( 'NONE', *, *, #11419, .T. ) ;
#47822 = CARTESIAN_POINT ( 'NONE',  ( -19.99999999999846523, 16.00000000000000000, 35.00000000000000000 ) ) ;
#47823 = CARTESIAN_POINT ( 'NONE',  ( 153.3040265531850537, 1.750000000000010658, 120.8182875569279702 ) ) ;
#47824 = CARTESIAN_POINT ( 'NONE',  ( -1.655785408455817675, -0.7536129375911022610, 9.903764339332079558 ) ) ;
#47825 = CIRCLE ( 'NONE', #50262, 1.750000000000009992 ) ;
#47826 = AXIS2_PLACEMENT_3D ( 'NONE', #31714, #50375, #23997 ) ;
#47827 = DIRECTION ( 'NONE',  ( -1.000000000000000000, -0.000000000000000000, -0.000000000000000000 ) ) ;
#47828 = VERTEX_POINT ( 'NONE', #23792 ) ;
#47829 = VECTOR ( 'NONE', #6179, 1000.000000000000000 ) ;
#47830 = EDGE_CURVE ( 'NONE', #1161, #37697, #32241, .T. ) ;
#47831 = DIRECTION ( 'NONE',  ( 1.000000000000000000, 0.000000000000000000, 0.000000000000000000 ) ) ;
#47832 = LINE ( 'NONE', #33001, #38806 ) ;
#47833 = CARTESIAN_POINT ( 'NONE',  ( -15.80799809827351154, 29.65358618225718956, -8.016098858316199838 ) ) ;
#47834 = AXIS2_PLACEMENT_3D ( 'NONE', #28546, #36266, #21092 ) ;
#47835 = CARTESIAN_POINT ( 'NONE',  ( -0.1291457462285138802, -10.01396534242280545, 3.215106848023631336 ) ) ;
#47836 = ADVANCED_FACE ( 'NONE', ( #4033 ), #19683, .T. ) ;
#47837 = CARTESIAN_POINT ( 'NONE',  ( 10.06660411345801620, 8.486842105263159297, 18.70408263333243326 ) ) ;
#47838 = CARTESIAN_POINT ( 'NONE',  ( -0.4098590526157695479, -3.751478160727021116, 9.865049507598754985 ) ) ;
#47839 = LINE ( 'NONE', #31999, #107 ) ;
#47840 =( BOUNDED_CURVE ( )  B_SPLINE_CURVE ( 3, ( #19875, #24758, #28092, #24251 ),
 .UNSPECIFIED., .F., .F. ) 
 B_SPLINE_CURVE_WITH_KNOTS ( ( 4, 4 ),
 ( 4.712388980384689674, 6.283185307179586232 ),
 .UNSPECIFIED. ) 
 CURVE ( )  GEOMETRIC_REPRESENTATION_ITEM ( )  RATIONAL_B_SPLINE_CURVE ( ( 1.000000000000000000, 0.8047378541243649375, 0.8047378541243649375, 1.000000000000000000 ) ) 
 REPRESENTATION_ITEM ( '' )  );
#47841 = EDGE_LOOP ( 'NONE', ( #43643, #40508, #9440, #32154 ) ) ;
#47842 = CARTESIAN_POINT ( 'NONE',  ( 18.79997501618727895, 32.48828710620309579, 6.057468652304064172 ) ) ;
#47843 = EDGE_CURVE ( 'NONE', #16057, #29337, #12912, .T. ) ;
#47844 = AXIS2_PLACEMENT_3D ( 'NONE', #372, #16016, #15259 ) ;
#47845 = EDGE_CURVE ( 'NONE', #1676, #39341, #32006, .T. ) ;
#47846 = DIRECTION ( 'NONE',  ( 1.000000000000000000, 0.000000000000000000, -0.000000000000000000 ) ) ;
#47847 = VECTOR ( 'NONE', #26916, 1000.000000000000227 ) ;
#47848 = VERTEX_POINT ( 'NONE', #8655 ) ;
#47849 = CARTESIAN_POINT ( 'NONE',  ( 33.30402655318503946, 0.000000000000000000, 165.0000000000000000 ) ) ;
#47850 = CARTESIAN_POINT ( 'NONE',  ( 74.32915281903215998, 1.750000000000009548, 1.843413822775065825 ) ) ;
#47851 = DIRECTION ( 'NONE',  ( -0.000000000000000000, -1.000000000000000000, -0.000000000000000000 ) ) ;
#47852 = EDGE_CURVE ( 'NONE', #36506, #10553, #32753, .T. ) ;
#47853 = EDGE_LOOP ( 'NONE', ( #2454, #17068, #34080, #19434, #42280, #31913 ) ) ;
#47854 = ORIENTED_EDGE ( 'NONE', *, *, #7055, .F. ) ;
#47855 = ORIENTED_EDGE ( 'NONE', *, *, #6057, .F. ) ;
#47856 = CARTESIAN_POINT ( 'NONE',  ( 16.15814872688565984, 4.048305257546810587, -2.870787844569587133 ) ) ;
#47857 = EDGE_CURVE ( 'NONE', #13694, #19053, #20672, .T. ) ;
#47858 = LINE ( 'NONE', #12986, #18089 ) ;
#47859 = ADVANCED_FACE ( 'NONE', ( #47599 ), #49449, .T. ) ;
#47860 = ORIENTED_EDGE ( 'NONE', *, *, #40758, .F. ) ;
#47861 = CARTESIAN_POINT ( 'NONE',  ( 31.55402655318503236, 1.025126265847089657, 79.06828755692797017 ) ) ;
#47862 = CARTESIAN_POINT ( 'NONE',  ( 166.9999999999999716, -256.4999999999999432, -339.9999999999998863 ) ) ;
#47863 = VECTOR ( 'NONE', #29733, 1000.000000000000000 ) ;
#47864 = VERTEX_POINT ( 'NONE', #40197 ) ;
#47865 = EDGE_CURVE ( 'NONE', #13851, #16979, #31693, .T. ) ;
#47866 =( BOUNDED_CURVE ( )  B_SPLINE_CURVE ( 3, ( #38142, #34535, #50116, #26831 ),
 .UNSPECIFIED., .F., .F. ) 
 B_SPLINE_CURVE_WITH_KNOTS ( ( 4, 4 ),
 ( 3.141592653589793116, 4.712388980384689674 ),
 .UNSPECIFIED. ) 
 CURVE ( )  GEOMETRIC_REPRESENTATION_ITEM ( )  RATIONAL_B_SPLINE_CURVE ( ( 1.000000000000000000, 0.8047378541243649375, 0.8047378541243649375, 1.000000000000000000 ) ) 
 REPRESENTATION_ITEM ( '' )  );
#47867 = EDGE_LOOP ( 'NONE', ( #3287, #9537, #20132, #6988 ) ) ;
#47868 = AXIS2_PLACEMENT_3D ( 'NONE', #8432, #13015, #5323 ) ;
#47869 = DIRECTION ( 'NONE',  ( -1.586032892321652236E-16, -1.000000000000000000, -2.288264760618012091E-48 ) ) ;
#47870 = PLANE ( 'NONE',  #25846 ) ;
#47871 = CARTESIAN_POINT ( 'NONE',  ( 153.3040265531850537, 0.000000000000000000, 165.0000000000000000 ) ) ;
#47872 = EDGE_LOOP ( 'NONE', ( #48581, #16875, #43805, #44282 ) ) ;
#47873 = FACE_OUTER_BOUND ( 'NONE', #9987, .T. ) ;
#47874 = DIRECTION ( 'NONE',  ( 1.000000000000000000, 0.000000000000000000, 1.612977847700450206E-50 ) ) ;
#47875 = ORIENTED_EDGE ( 'NONE', *, *, #21630, .T. ) ;
#47876 = ORIENTED_EDGE ( 'NONE', *, *, #13368, .T. ) ;
#47877 = ORIENTED_EDGE ( 'NONE', *, *, #40862, .F. ) ;
#47878 = CYLINDRICAL_SURFACE ( 'NONE', #15586, 1.750000000000015543 ) ;
#47879 = CARTESIAN_POINT ( 'NONE',  ( -1.841192853132492813, -1.035021892307830482, 9.890170120223997330 ) ) ;
#47880 = VERTEX_POINT ( 'NONE', #20428 ) ;
#47881 = CARTESIAN_POINT ( 'NONE',  ( -19.99999999999878142, 16.00000000000000000, 5.000000000000004441 ) ) ;
#47882 = DIRECTION ( 'NONE',  ( 0.000000000000000000, -1.000000000000000000, -3.186989995019654210E-49 ) ) ;
#47883 = DIRECTION ( 'NONE',  ( 1.156482317317870492E-16, -1.000000000000000000, -0.000000000000000000 ) ) ;
#47884 = AXIS2_PLACEMENT_3D ( 'NONE', #28899, #36884, #37629 ) ;
#47885 = CARTESIAN_POINT ( 'NONE',  ( 112.2789002873379758, 1.749999999999996669, -38.15658617722495194 ) ) ;
#47886 = CARTESIAN_POINT ( 'NONE',  ( -42.99990394833793061, 47.95759300784327905, -5.000000000000000000 ) ) ;
#47887 = CARTESIAN_POINT ( 'NONE',  ( -88.44597344681494633, -1.025126265847089657, 79.06828755692797017 ) ) ;
#47888 = CARTESIAN_POINT ( 'NONE',  ( 195.0540265531851105, 1.025126265847089435, 2.568287556927986159 ) ) ;
#47889 = CARTESIAN_POINT ( 'NONE',  ( -1.019713130072858798, -3.848720492505054658, 6.098637220230962441E-17 ) ) ;
#47890 = CARTESIAN_POINT ( 'NONE',  ( 30.00000000000187228, 16.00000000000000000, 65.00000000000000000 ) ) ;
#47891 = CARTESIAN_POINT ( 'NONE',  ( 0.3862712429686978033, -1.188820645368937834, -3.333333333333333481 ) ) ;
#47892 = EDGE_CURVE ( 'NONE', #20200, #18355, #36113, .T. ) ;
#47893 = CARTESIAN_POINT ( 'NONE',  ( 135.0000000000015632, 16.00000000000000000, 35.00000000000000000 ) ) ;
#47894 = AXIS2_PLACEMENT_3D ( 'NONE', #10749, #42307, #34370 ) ;
#47895 = DIRECTION ( 'NONE',  ( 0.000000000000000000, -0.000000000000000000, -1.000000000000000000 ) ) ;
#47896 = ORIENTED_EDGE ( 'NONE', *, *, #27469, .F. ) ;
#47897 = DIRECTION ( 'NONE',  ( -0.000000000000000000, 0.000000000000000000, -1.000000000000000000 ) ) ;
#47898 = CARTESIAN_POINT ( 'NONE',  ( 35.05402655318504657, 2.143131898507880377E-16, 122.5682875569279702 ) ) ;
#47899 = DIRECTION ( 'NONE',  ( -0.000000000000000000, -0.000000000000000000, -1.000000000000000000 ) ) ;
#47900 = AXIS2_PLACEMENT_3D ( 'NONE', #31032, #3819, #43063 ) ;
#47901 = DIRECTION ( 'NONE',  ( 1.000000000000000000, 0.000000000000000000, 0.000000000000000000 ) ) ;
#47902 = ORIENTED_EDGE ( 'NONE', *, *, #12727, .F. ) ;
#47903 = FILL_AREA_STYLE_COLOUR ( '', #37097 ) ;
#47904 = EDGE_CURVE ( 'NONE', #42641, #26504, #2140, .T. ) ;
#47905 = ADVANCED_FACE ( 'NONE', ( #32253 ), #17095, .T. ) ;
#47906 = CARTESIAN_POINT ( 'NONE',  ( -48.44597344681496054, 1.025126265847089213, -160.9317124430720014 ) ) ;
#47907 = EDGE_LOOP ( 'NONE', ( #45043, #18931, #18045, #9660 ) ) ;
#47908 = CARTESIAN_POINT ( 'NONE',  ( -44.94597344681493922, -1.025126265847089435, -117.4317124430720156 ) ) ;
#47909 = PLANE ( 'NONE',  #7659 ) ;
#47910 = CARTESIAN_POINT ( 'NONE',  ( 9.358026734184097251, 0.000000000000000000, 0.000000000000000000 ) ) ;
#47911 = ORIENTED_EDGE ( 'NONE', *, *, #20076, .T. ) ;
#47912 = PLANE ( 'NONE',  #24127 ) ;
#47913 = EDGE_LOOP ( 'NONE', ( #5164, #30642, #29214, #15275, #25264, #10099 ) ) ;
#47914 = ORIENTED_EDGE ( 'NONE', *, *, #47177, .F. ) ;
#47915 = EDGE_CURVE ( 'NONE', #14561, #49775, #28363, .T. ) ;
#47916 = EDGE_CURVE ( 'NONE', #19896, #47246, #21193, .T. ) ;
#47917 = VECTOR ( 'NONE', #47982, 1000.000000000000000 ) ;
#47918 = ORIENTED_EDGE ( 'NONE', *, *, #13260, .F. ) ;
#47919 = DIRECTION ( 'NONE',  ( -0.000000000000000000, -1.000000000000000000, -0.000000000000000000 ) ) ;
#47920 = LINE ( 'NONE', #20005, #33922 ) ;
#47921 = AXIS2_PLACEMENT_3D ( 'NONE', #36388, #28664, #47615 ) ;
#47922 = ORIENTED_EDGE ( 'NONE', *, *, #49464, .T. ) ;
#47923 = CARTESIAN_POINT ( 'NONE',  ( 240.0000000000000000, -164.9999999999999716, 32.29650858650035161 ) ) ;
#47924 = DIRECTION ( 'NONE',  ( -1.000000000000000000, 0.000000000000000000, 0.000000000000000000 ) ) ;
#47925 = ADVANCED_FACE ( 'NONE', ( #32519 ), #13492, .F. ) ;
#47926 = DIRECTION ( 'NONE',  ( -0.000000000000000000, -0.000000000000000000, -1.000000000000000000 ) ) ;
#47927 = AXIS2_PLACEMENT_3D ( 'NONE', #9315, #13405, #24977 ) ;
#47928 = CARTESIAN_POINT ( 'NONE',  ( 370.7621192902014968, -67.00570555996102939, -94.69675437945474528 ) ) ;
#47929 = ORIENTED_EDGE ( 'NONE', *, *, #16369, .F. ) ;
#47930 = CYLINDRICAL_SURFACE ( 'NONE', #26450, 1.750000000000015543 ) ;
#47931 = AXIS2_PLACEMENT_3D ( 'NONE', #37549, #17270, #45439 ) ;
#47932 = ORIENTED_EDGE ( 'NONE', *, *, #33791, .F. ) ;
#47933 = CARTESIAN_POINT ( 'NONE',  ( 210.0000000000000568, 0.000000000000000000, 0.8182875569279768335 ) ) ;
#47934 = CARTESIAN_POINT ( 'NONE',  ( -19.99999999999785416, 16.00000000000000000, 115.0000000000000142 ) ) ;
#47935 = AXIS2_PLACEMENT_3D ( 'NONE', #2539, #33861, #49448 ) ;
#47936 = ORIENTED_EDGE ( 'NONE', *, *, #9729, .F. ) ;
#47937 = CARTESIAN_POINT ( 'NONE',  ( -6.695973446814940111, 1.750000000000024203, 80.81828755692798438 ) ) ;
#47938 = CARTESIAN_POINT ( 'NONE',  ( 5.551115123125782702E-14, -180.9999999999999716, 359.9999999999997726 ) ) ;
#47939 = EDGE_LOOP ( 'NONE', ( #12645, #34683, #127, #13639 ) ) ;
#47940 = AXIS2_PLACEMENT_3D ( 'NONE', #674, #16326, #36865 ) ;
#47941 = CARTESIAN_POINT ( 'NONE',  ( -31.94178169330213279, 9.256608784834037706, -3.760136334089591248 ) ) ;
#47942 = CARTESIAN_POINT ( 'NONE',  ( 0.6215990105956902267, -1.608617984725389860, 9.928159647716132241 ) ) ;
#47943 = CARTESIAN_POINT ( 'NONE',  ( -45.67084718096785423, -1.750000000000010436, -80.20683870891910772 ) ) ;
#47944 = CARTESIAN_POINT ( 'NONE',  ( 194.3291528190321742, 1.750000000000009548, 159.7931612910809065 ) ) ;
#47945 = ORIENTED_EDGE ( 'NONE', *, *, #28369, .F. ) ;
#47946 =( BOUNDED_CURVE ( )  B_SPLINE_CURVE ( 3, ( #30287, #29781, #37748, #15134 ),
 .UNSPECIFIED., .F., .F. ) 
 B_SPLINE_CURVE_WITH_KNOTS ( ( 4, 4 ),
 ( 1.570796326794896558, 3.141592653589793116 ),
 .UNSPECIFIED. ) 
 CURVE ( )  GEOMETRIC_REPRESENTATION_ITEM ( )  RATIONAL_B_SPLINE_CURVE ( ( 1.000000000000000000, 0.8047378541243649375, 0.8047378541243649375, 1.000000000000000000 ) ) 
 REPRESENTATION_ITEM ( '' )  );
#47947 = DIRECTION ( 'NONE',  ( -0.000000000000000000, -0.000000000000000000, -1.000000000000000000 ) ) ;
#47948 = FACE_OUTER_BOUND ( 'NONE', #29282, .T. ) ;
#47949 = DIRECTION ( 'NONE',  ( 1.000000000000000000, 0.000000000000000000, 0.000000000000000000 ) ) ;
#47950 = ORIENTED_EDGE ( 'NONE', *, *, #28088, .F. ) ;
#47951 = ADVANCED_FACE ( 'NONE', ( #48097, #12979 ), #9143, .T. ) ;
#47952 = EDGE_LOOP ( 'NONE', ( #29909, #34053 ) ) ;
#47953 = DIRECTION ( 'NONE',  ( -0.1191452206184307888, 0.000000000000000000, 0.9928768384869220975 ) ) ;
#47954 = CARTESIAN_POINT ( 'NONE',  ( 115.0540265531850395, 2.143131898507847836E-16, -77.43171244307204404 ) ) ;
#47955 = VECTOR ( 'NONE', #14122, 1000.000000000000000 ) ;
#47956 =( NAMED_UNIT ( * ) PLANE_ANGLE_UNIT ( ) SI_UNIT ( $, .RADIAN. ) );
#47958 = VECTOR ( 'NONE', #19637, 1000.000000000000000 ) ;
#47957 = DIRECTION ( 'NONE',  ( 0.000000000000000000, -1.000000000000000000, 0.000000000000000000 ) ) ;
#47959 = CARTESIAN_POINT ( 'NONE',  ( 8.831420117243668599, 14.12636088103192655, -3.546734833711462365 ) ) ;
#47960 = ORIENTED_EDGE ( 'NONE', *, *, #9844, .F. ) ;
#47961 = CARTESIAN_POINT ( 'NONE',  ( 21.85563210430597181, 40.58578877481934910, 8.807470649214879543 ) ) ;
#47962 = AXIS2_PLACEMENT_3D ( 'NONE', #23967, #39627, #23468 ) ;
#47963 = CYLINDRICAL_SURFACE ( 'NONE', #32373, 1.750000000000010214 ) ;
#47964 = CARTESIAN_POINT ( 'NONE',  ( -48.44597344681495343, 0.000000000000000000, 79.06828755692797017 ) ) ;
#47965 = AXIS2_PLACEMENT_3D ( 'NONE', #35126, #12010, #34599 ) ;
#47966 = ORIENTED_EDGE ( 'NONE', *, *, #47236, .F. ) ;
#47967 = DIRECTION ( 'NONE',  ( -1.000000000000000000, 0.000000000000000000, 0.000000000000000000 ) ) ;
#47968 = ORIENTED_EDGE ( 'NONE', *, *, #24099, .T. ) ;
#47969 = CARTESIAN_POINT ( 'NONE',  ( 9.999999999999998224, 8.486842105263161073, 18.34680996553531784 ) ) ;
#47970 = VECTOR ( 'NONE', #39113, 1000.000000000000000 ) ;
#47971 = VERTEX_POINT ( 'NONE', #49103 ) ;
#47972 = CARTESIAN_POINT ( 'NONE',  ( 135.0000000000000000, 17.00000000000000000, -114.9999999999999858 ) ) ;
#47973 = CARTESIAN_POINT ( 'NONE',  ( -9.174209336589896679, -3.979181203266159095, 9.646707543097347681 ) ) ;
#47974 = CARTESIAN_POINT ( 'NONE',  ( -204.9459734468148895, -1.025126265847089213, -37.43171244307202272 ) ) ;
#47975 = FACE_OUTER_BOUND ( 'NONE', #23766, .T. ) ;
#47976 = ORIENTED_EDGE ( 'NONE', *, *, #28537, .F. ) ;
#47977 = CARTESIAN_POINT ( 'NONE',  ( 0.000000000000000000, 185.0000000000000284, 355.9999999999997726 ) ) ;
#47978 = ORIENTED_EDGE ( 'NONE', *, *, #1148, .F. ) ;
#47979 = DIRECTION ( 'NONE',  ( -1.000000000000000000, -0.000000000000000000, -0.000000000000000000 ) ) ;
#47980 = LINE ( 'NONE', #44649, #50222 ) ;
#47981 = CARTESIAN_POINT ( 'NONE',  ( 1.186340292695366783, -0.3298841998003522735, 9.975326647350891918 ) ) ;
#47982 = DIRECTION ( 'NONE',  ( -1.000000000000000000, -0.000000000000000000, -0.000000000000000000 ) ) ;
#47983 = EDGE_CURVE ( 'NONE', #10796, #6015, #49357, .T. ) ;
#47984 = ORIENTED_EDGE ( 'NONE', *, *, #24747, .F. ) ;
#47985 = ORIENTED_EDGE ( 'NONE', *, *, #19250, .T. ) ;
#47986 = LINE ( 'NONE', #24193, #39069 ) ;
#47987 = ORIENTED_EDGE ( 'NONE', *, *, #31586, .F. ) ;
#47988 = AXIS2_PLACEMENT_3D ( 'NONE', #49243, #37025, #33165 ) ;
#47989 = CARTESIAN_POINT ( 'NONE',  ( -5.000000000000000000, -165.1999999999999602, 340.1999999999997044 ) ) ;
#47990 = CARTESIAN_POINT ( 'NONE',  ( 155.0540265531850537, 2.143131898507880377E-16, 82.56828755692798438 ) ) ;
#47991 = CARTESIAN_POINT ( 'NONE',  ( 344.0000000000000000, -174.9999999999999432, 339.9999999999998295 ) ) ;
#47992 = AXIS2_PLACEMENT_3D ( 'NONE', #7219, #26963, #39040 ) ;
#47993 = ORIENTED_EDGE ( 'NONE', *, *, #18608, .T. ) ;
#47994 = DIRECTION ( 'NONE',  ( -1.586032892321652236E-16, -1.000000000000000000, -6.853681917100419162E-49 ) ) ;
#47995 = FACE_OUTER_BOUND ( 'NONE', #36802, .T. ) ;
#47996 = PLANE ( 'NONE',  #36644 ) ;
#47997 = CARTESIAN_POINT ( 'NONE',  ( 343.9999999999999432, -181.0000000000001421, -349.9999999999998863 ) ) ;
#47998 = CARTESIAN_POINT ( 'NONE',  ( -69.99999999999972999, 17.00000000000000000, -84.99999999999998579 ) ) ;
#47999 =( BOUNDED_CURVE ( )  B_SPLINE_CURVE ( 3, ( #32963, #8838, #20635, #48544 ),
 .UNSPECIFIED., .F., .F. ) 
 B_SPLINE_CURVE_WITH_KNOTS ( ( 4, 4 ),
 ( 1.570796326794903663, 3.141592653589793116 ),
 .UNSPECIFIED. ) 
 CURVE ( )  GEOMETRIC_REPRESENTATION_ITEM ( )  RATIONAL_B_SPLINE_CURVE ( ( 1.000000000000000000, 0.8047378541243667138, 0.8047378541243667138, 1.000000000000000000 ) ) 
 REPRESENTATION_ITEM ( '' )  );
#48001 = VECTOR ( 'NONE', #19639, 1000.000000000000000 ) ;
#48000 = FACE_BOUND ( 'NONE', #49225, .T. ) ;
#48002 = ORIENTED_EDGE ( 'NONE', *, *, #41882, .F. ) ;
#48003 = ORIENTED_EDGE ( 'NONE', *, *, #8336, .T. ) ;
#48004 = CIRCLE ( 'NONE', #1365, 1.750000000000015543 ) ;
#48005 = VERTEX_POINT ( 'NONE', #7781 ) ;
#48006 = DIRECTION ( 'NONE',  ( -1.000000000000000000, -0.000000000000000000, -0.000000000000000000 ) ) ;
#48007 = CARTESIAN_POINT ( 'NONE',  ( 358.0000000000000000, 181.0000000000000284, -356.0000000000001705 ) ) ;
#48008 =( BOUNDED_CURVE ( )  B_SPLINE_CURVE ( 3, ( #10642, #26553, #17148, #41949 ),
 .UNSPECIFIED., .F., .F. ) 
 B_SPLINE_CURVE_WITH_KNOTS ( ( 4, 4 ),
 ( 4.712388980384689674, 6.283185307179586232 ),
 .UNSPECIFIED. ) 
 CURVE ( )  GEOMETRIC_REPRESENTATION_ITEM ( )  RATIONAL_B_SPLINE_CURVE ( ( 1.000000000000000000, 0.8047378541243649375, 0.8047378541243649375, 1.000000000000000000 ) ) 
 REPRESENTATION_ITEM ( '' )  );
#48009 = DIRECTION ( 'NONE',  ( -0.000000000000000000, -1.000000000000000000, -0.000000000000000000 ) ) ;
#48010 = DIRECTION ( 'NONE',  ( 0.000000000000000000, 0.000000000000000000, 1.000000000000000000 ) ) ;
#48011 = ORIENTED_EDGE ( 'NONE', *, *, #22650, .F. ) ;
#48012 = AXIS2_PLACEMENT_3D ( 'NONE', #34221, #10097, #49798 ) ;
#48013 = CARTESIAN_POINT ( 'NONE',  ( -167.7210997126620384, 1.750000000000009548, -40.20683870891912193 ) ) ;
#48014 = ORIENTED_EDGE ( 'NONE', *, *, #15233, .T. ) ;
#48015 = CARTESIAN_POINT ( 'NONE',  ( -2.462075149652696027, 16.57295996686994499, 9.403735324607438884 ) ) ;
#48016 = DIRECTION ( 'NONE',  ( 1.000000000000000000, 0.000000000000000000, -0.000000000000000000 ) ) ;
#48017 = CARTESIAN_POINT ( 'NONE',  ( -44.94597344681493922, 1.025126265847089879, -117.4317124430720156 ) ) ;
#48018 = DIRECTION ( 'NONE',  ( -1.000000000000000000, -1.156482317317870492E-16, 0.000000000000000000 ) ) ;
#48019 = FACE_OUTER_BOUND ( 'NONE', #41140, .T. ) ;
#48020 = CARTESIAN_POINT ( 'NONE',  ( 35.51846793572394034, -35.99772139009119343, 7.906207997025717304 ) ) ;
#48021 = ORIENTED_EDGE ( 'NONE', *, *, #41819, .F. ) ;
#48022 = DIRECTION ( 'NONE',  ( -1.000000000000000000, 0.000000000000000000, 0.000000000000000000 ) ) ;
#48023 = CARTESIAN_POINT ( 'NONE',  ( 151.5540265531850537, 0.000000000000000000, 159.0682875569279702 ) ) ;
#48024 = DIRECTION ( 'NONE',  ( 0.000000000000000000, 1.000000000000000000, 6.123233995736766036E-17 ) ) ;
#48025 = FILL_AREA_STYLE_COLOUR ( '', #10842 ) ;
#48027 = ORIENTED_EDGE ( 'NONE', *, *, #42734, .T. ) ;
#48026 = VECTOR ( 'NONE', #6069, 1000.000000000000000 ) ;
#48028 = B_SPLINE_CURVE_WITH_KNOTS ( 'NONE', 3,
 ( #11107, #15213, #26758, #39334 ),
 .UNSPECIFIED., .F., .F.,
 ( 4, 4 ),
 ( 0.7998230999345287140, 0.9869080488566185361 ),
 .UNSPECIFIED. ) ;
#48029 = ORIENTED_EDGE ( 'NONE', *, *, #15059, .F. ) ;
#48030 = DIRECTION ( 'NONE',  ( 7.793956916774525800E-48, 0.000000000000000000, -1.000000000000000000 ) ) ;
#48031 = CARTESIAN_POINT ( 'NONE',  ( 1.436574951976903991, -1.361596091069418701, 9.897807938190499755 ) ) ;
#48032 = ORIENTED_EDGE ( 'NONE', *, *, #27289, .T. ) ;
#48033 = ORIENTED_EDGE ( 'NONE', *, *, #36701, .T. ) ;
#48034 = EDGE_CURVE ( 'NONE', #32484, #50534, #14502, .T. ) ;
#48035 = CARTESIAN_POINT ( 'NONE',  ( 183.0000000000000000, -93.50000000000005684, -340.0000000000001137 ) ) ;
#48036 = CARTESIAN_POINT ( 'NONE',  ( 23.31729631074197329, 24.19776167542427814, -8.016098858316199838 ) ) ;
#48037 = CARTESIAN_POINT ( 'NONE',  ( -167.7210997126620384, 1.750000000000009548, -160.2068387089191219 ) ) ;
#48038 = DIRECTION ( 'NONE',  ( -1.000000000000000000, -0.000000000000000000, -0.000000000000000000 ) ) ;
#48039 = EDGE_CURVE ( 'NONE', #214, #27650, #4387, .T. ) ;
#48040 = VERTEX_POINT ( 'NONE', #49605 ) ;
#48041 = ORIENTED_EDGE ( 'NONE', *, *, #25203, .T. ) ;
#48042 = ADVANCED_FACE ( 'NONE', ( #29651 ), #6806, .T. ) ;
#48043 = VECTOR ( 'NONE', #24325, 1000.000000000000000 ) ;
#48044 = CARTESIAN_POINT ( 'NONE',  ( 153.3040265531850537, 1.750000000000010658, 80.81828755692798438 ) ) ;
#48045 = EDGE_CURVE ( 'NONE', #47536, #25227, #3908, .T. ) ;
#48046 = EDGE_LOOP ( 'NONE', ( #12387, #17052, #11950, #34282 ) ) ;
#48047 = VERTEX_POINT ( 'NONE', #41192 ) ;
#48048 = CARTESIAN_POINT ( 'NONE',  ( -46.69597344681494633, 1.750000000000010214, -39.18171244307202983 ) ) ;
#48049 = CARTESIAN_POINT ( 'NONE',  ( 1.320835335343329753, -0.01943189459118491516, 9.943883492372847854 ) ) ;
#48050 = CARTESIAN_POINT ( 'NONE',  ( 191.5540265531850537, -1.025126265847089879, -77.43171244307200141 ) ) ;
#48051 = DIRECTION ( 'NONE',  ( -1.000000000000000000, -0.000000000000000000, -0.000000000000000000 ) ) ;
#48052 = EDGE_LOOP ( 'NONE', ( #5812, #28292, #20928, #7636 ) ) ;
#48053 = ORIENTED_EDGE ( 'NONE', *, *, #21603, .F. ) ;
#48054 = ORIENTED_EDGE ( 'NONE', *, *, #27730, .F. ) ;
#48055 = LINE ( 'NONE', #8361, #26688 ) ;
#48056 = AXIS2_PLACEMENT_3D ( 'NONE', #1987, #2731, #9682 ) ;
#48057 = CARTESIAN_POINT ( 'NONE',  ( -34.38425513258695077, 36.82177522737848108, 8.807470649214879543 ) ) ;
#48058 = ORIENTED_EDGE ( 'NONE', *, *, #42272, .F. ) ;
#48059 = ORIENTED_EDGE ( 'NONE', *, *, #38410, .F. ) ;
#48060 = CARTESIAN_POINT ( 'NONE',  ( -28.52604530808686079, -41.07801380285659576, -3.760136334089591248 ) ) ;
#48061 = DIRECTION ( 'NONE',  ( -0.000000000000000000, -0.000000000000000000, -1.000000000000000000 ) ) ;
#48062 = ORIENTED_EDGE ( 'NONE', *, *, #15856, .F. ) ;
#48063 = EDGE_CURVE ( 'NONE', #20388, #14316, #29907, .T. ) ;
#48064 = ADVANCED_FACE ( 'NONE', ( #33512 ), #38477, .T. ) ;
#48065 = ORIENTED_EDGE ( 'NONE', *, *, #33211, .T. ) ;
#48066 = FACE_OUTER_BOUND ( 'NONE', #36763, .T. ) ;
#48067 = SURFACE_STYLE_USAGE ( .BOTH. , #32487 ) ;
#48068 = ORIENTED_EDGE ( 'NONE', *, *, #37858, .T. ) ;
#48069 = EDGE_CURVE ( 'NONE', #9965, #28730, #11758, .T. ) ;
#48070 = CARTESIAN_POINT ( 'NONE',  ( 177.5000000000000000, -77.43746236555679729, -130.5992382549688671 ) ) ;
#48071 = CARTESIAN_POINT ( 'NONE',  ( 151.5540265531850537, 0.000000000000000000, 122.5682875569279702 ) ) ;
#48072 = DIRECTION ( 'NONE',  ( 1.000000000000000000, 0.000000000000000000, 0.000000000000000000 ) ) ;
#48073 = EDGE_CURVE ( 'NONE', #9715, #45355, #14256, .T. ) ;
#48074 = CARTESIAN_POINT ( 'NONE',  ( 5.551115123125782702E-14, -182.9999999999999716, 355.9999999999997726 ) ) ;
#48075 = ORIENTED_EDGE ( 'NONE', *, *, #19907, .F. ) ;
#48076 = EDGE_CURVE ( 'NONE', #42991, #45968, #49845, .T. ) ;
#48077 = DIRECTION ( 'NONE',  ( 0.000000000000000000, 0.000000000000000000, -1.000000000000000000 ) ) ;
#48078 = EDGE_CURVE ( 'NONE', #26951, #48972, #11278, .T. ) ;
#48079 = DIRECTION ( 'NONE',  ( -0.000000000000000000, -0.000000000000000000, -1.000000000000000000 ) ) ;
#48080 = B_SPLINE_SURFACE_WITH_KNOTS ( 'NONE', 3, 3, ( 
 ( #4355, #19220, #26687, #46402 ),
 ( #3573, #42572, #15899, #7450 ),
 ( #23077, #23593, #19992, #23336 ),
 ( #35677, #14883, #30534, #30797 ) ),
 .UNSPECIFIED., .F., .F., .F.,
 ( 4, 4 ),
 ( 4, 4 ),
 ( 0.000000000000000000, 1.000000000000000000 ),
 ( 0.000000000000000000, 1.000000000000000000 ),
 .UNSPECIFIED. ) ;
#48081 = DIRECTION ( 'NONE',  ( 0.000000000000000000, 1.000000000000000000, -0.000000000000000000 ) ) ;
#48082 = DIRECTION ( 'NONE',  ( -1.000000000000000000, 0.000000000000000000, 0.000000000000000000 ) ) ;
#48083 = CARTESIAN_POINT ( 'NONE',  ( -119.9999999999987921, 16.00000000000000000, 30.00000000000000000 ) ) ;
#48084 = CARTESIAN_POINT ( 'NONE',  ( 210.0000000000000568, 0.000000000000000000, 160.8182875569279702 ) ) ;
#48085 = CARTESIAN_POINT ( 'NONE',  ( -6.695973446814940111, -1.750000000000024203, -119.1817124430720440 ) ) ;
#48086 = EDGE_CURVE ( 'NONE', #13210, #47506, #516, .T. ) ;
#48087 = CARTESIAN_POINT ( 'NONE',  ( 33.08717642956892746, 5.870837526465160217, -8.016098858316199838 ) ) ;
#48088 = ADVANCED_FACE ( 'NONE', ( #18096 ), #28531, .F. ) ;
#48089 = EDGE_LOOP ( 'NONE', ( #41278, #47544, #18230 ) ) ;
#48090 = CARTESIAN_POINT ( 'NONE',  ( 113.3040265531850537, 1.749999999999997335, 120.8182875569279702 ) ) ;
#48091 = EDGE_CURVE ( 'NONE', #13146, #36974, #35996, .T. ) ;
#48092 = AXIS2_PLACEMENT_3D ( 'NONE', #28377, #8866, #24524 ) ;
#48093 = EDGE_CURVE ( 'NONE', #5809, #11044, #35754, .T. ) ;
#48094 = DIRECTION ( 'NONE',  ( -1.000000000000000000, -1.156482317317870492E-16, 0.000000000000000000 ) ) ;
#48095 = ORIENTED_EDGE ( 'NONE', *, *, #16718, .F. ) ;
#48096 = CARTESIAN_POINT ( 'NONE',  ( -4.641001526964561918, -45.74479092860853058, -8.016098858316205167 ) ) ;
#48097 = FACE_BOUND ( 'NONE', #49503, .T. ) ;
#48098 = LINE ( 'NONE', #8399, #15183 ) ;
#48099 = ORIENTED_EDGE ( 'NONE', *, *, #7333, .F. ) ;
#48100 = CARTESIAN_POINT ( 'NONE',  ( -84.94597344681494633, 2.143131898507880377E-16, -160.9317124430720014 ) ) ;
#48101 = ORIENTED_EDGE ( 'NONE', *, *, #5889, .T. ) ;
#48103 = VERTEX_POINT ( 'NONE', #16227 ) ;
#48102 = B_SPLINE_CURVE_WITH_KNOTS ( 'NONE', 3,
 ( #23011, #35106, #24493, #42754 ),
 .UNSPECIFIED., .F., .F.,
 ( 4, 4 ),
 ( 0.003479523240173989628, 0.009617604115990840280 ),
 .UNSPECIFIED. ) ;
#48104 = CARTESIAN_POINT ( 'NONE',  ( 1.035950918207909632, 33.23661552194049307, -2.408242355805840784 ) ) ;
#48105 = ADVANCED_FACE ( 'NONE', ( #27531 ), #16723, .T. ) ;
#48106 = DIRECTION ( 'NONE',  ( -1.000000000000000000, -0.000000000000000000, -0.000000000000000000 ) ) ;
#48107 = ORIENTED_EDGE ( 'NONE', *, *, #45303, .F. ) ;
#48108 = CARTESIAN_POINT ( 'NONE',  ( -64.99999999999909051, 17.00000000000000000, -24.99999999999999289 ) ) ;
#48109 = CARTESIAN_POINT ( 'NONE',  ( 33.30402655318503946, 1.750000000000009992, 0.8182875569279768335 ) ) ;
#48110 = VERTEX_POINT ( 'NONE', #47484 ) ;
#48111 = ORIENTED_EDGE ( 'NONE', *, *, #27288, .F. ) ;
#48112 = CARTESIAN_POINT ( 'NONE',  ( 71.55402655318505367, 0.000000000000000000, 79.06828755692797017 ) ) ;
#48113 = VERTEX_POINT ( 'NONE', #12128 ) ;
#48114 = DIRECTION ( 'NONE',  ( -1.586032892321652236E-16, -1.000000000000000000, -2.288264760618012091E-48 ) ) ;
#48115 = CARTESIAN_POINT ( 'NONE',  ( 155.0540265531850537, 0.000000000000000000, 162.5682875569279702 ) ) ;
#48116 = CARTESIAN_POINT ( 'NONE',  ( 1.011271242968688311, -0.7347315653655855927, 10.00000000000000000 ) ) ;
#48117 = EDGE_LOOP ( 'NONE', ( #19893, #38761, #36177, #38848, #33112, #31175, #14462, #2546 ) ) ;
#48118 = PLANE ( 'NONE',  #33364 ) ;
#48119 = LINE ( 'NONE', #40478, #1601 ) ;
#48120 = VERTEX_POINT ( 'NONE', #20069 ) ;
#48121 = ADVANCED_FACE ( 'NONE', ( #43170 ), #39586, .T. ) ;
#48122 = EDGE_LOOP ( 'NONE', ( #28592, #11632, #20349, #33971 ) ) ;
#48123 = ORIENTED_EDGE ( 'NONE', *, *, #35978, .F. ) ;
#48124 = LINE ( 'NONE', #13009, #21331 ) ;
#48125 = CARTESIAN_POINT ( 'NONE',  ( 35.00000000000152767, 17.00000000000000000, 60.00000000000000000 ) ) ;
#48126 = VERTEX_POINT ( 'NONE', #44157 ) ;
#48127 = FACE_OUTER_BOUND ( 'NONE', #30620, .T. ) ;
#48128 = DIRECTION ( 'NONE',  ( 0.000000000000000000, 1.000000000000000000, 0.000000000000000000 ) ) ;
#48129 = EDGE_CURVE ( 'NONE', #33010, #42224, #33613, .T. ) ;
#48130 = CARTESIAN_POINT ( 'NONE',  ( -0.3147652639076214398, 1.255102005797271936, 9.947020512645419643 ) ) ;
#48131 = LINE ( 'NONE', #9178, #37827 ) ;
#48132 = EDGE_CURVE ( 'NONE', #6887, #29772, #44506, .T. ) ;
#48133 = DIRECTION ( 'NONE',  ( 6.203854594147707562E-25, -2.067951531382569187E-25, 1.000000000000000000 ) ) ;
#48134 = CARTESIAN_POINT ( 'NONE',  ( 193.3040265531851105, 1.750000000000009992, 0.8182875569279768335 ) ) ;
#48135 = CARTESIAN_POINT ( 'NONE',  ( 183.0000000000000000, -93.49999999999998579, -340.0000000000001137 ) ) ;
#48136 = EDGE_CURVE ( 'NONE', #34969, #21408, #14554, .T. ) ;
#48137 = DIRECTION ( 'NONE',  ( -1.000000000000000000, -0.000000000000000000, -0.000000000000000000 ) ) ;
#48138 = FACE_OUTER_BOUND ( 'NONE', #43729, .T. ) ;
#48139 = EDGE_CURVE ( 'NONE', #15830, #11949, #35544, .T. ) ;
#48140 = EDGE_CURVE ( 'NONE', #8986, #10351, #8534, .T. ) ;
#48141 = DIRECTION ( 'NONE',  ( -0.9928768384869219865, 0.000000000000000000, -0.1191452206184307749 ) ) ;
#48142 =( BOUNDED_CURVE ( )  B_SPLINE_CURVE ( 3, ( #49109, #13998, #45279, #10159 ),
 .UNSPECIFIED., .F., .F. ) 
 B_SPLINE_CURVE_WITH_KNOTS ( ( 4, 4 ),
 ( 0.000000000000000000, 1.570796326794896558 ),
 .UNSPECIFIED. ) 
 CURVE ( )  GEOMETRIC_REPRESENTATION_ITEM ( )  RATIONAL_B_SPLINE_CURVE ( ( 1.000000000000000000, 0.8047378541243649375, 0.8047378541243649375, 1.000000000000000000 ) ) 
 REPRESENTATION_ITEM ( '' )  );
#48143 = UNCERTAINTY_MEASURE_WITH_UNIT (LENGTH_MEASURE( 1.000000000000000082E-05 ), #34954, 'distance_accuracy_value', 'NONE');
#48144 = LINE ( 'NONE', #37425, #22445 ) ;
#48145 = ORIENTED_EDGE ( 'NONE', *, *, #41771, .F. ) ;
#48146 = CARTESIAN_POINT ( 'NONE',  ( -0.7831114705608903659, -7.934214658316839142, -3.496552006265751800E-15 ) ) ;
#48147 =( BOUNDED_CURVE ( )  B_SPLINE_CURVE ( 3, ( #44059, #5572, #5063, #20723 ),
 .UNSPECIFIED., .F., .F. ) 
 B_SPLINE_CURVE_WITH_KNOTS ( ( 4, 4 ),
 ( 1.570796326794896558, 3.141592653589793116 ),
 .UNSPECIFIED. ) 
 CURVE ( )  GEOMETRIC_REPRESENTATION_ITEM ( )  RATIONAL_B_SPLINE_CURVE ( ( 1.000000000000000000, 0.8047378541243649375, 0.8047378541243649375, 1.000000000000000000 ) ) 
 REPRESENTATION_ITEM ( '' )  );
#48148 = ADVANCED_FACE ( 'NONE', ( #4681 ), #20321, .T. ) ;
#48149 = DIRECTION ( 'NONE',  ( 0.000000000000000000, 0.000000000000000000, -1.000000000000000000 ) ) ;
#48150 = LINE ( 'NONE', #32566, #20935 ) ;
#48151 = LINE ( 'NONE', #28459, #18857 ) ;
#48152 = VERTEX_POINT ( 'NONE', #23919 ) ;
#48153 = CARTESIAN_POINT ( 'NONE',  ( 168.9999999999999716, -166.9999999999999432, -350.0000000000001705 ) ) ;
#48154 = EDGE_CURVE ( 'NONE', #5511, #29610, #16529, .T. ) ;
#48155 = CARTESIAN_POINT ( 'NONE',  ( 350.0000000000000000, 169.0000000000000000, -342.0000000000001705 ) ) ;
#48156 = ORIENTED_EDGE ( 'NONE', *, *, #26070, .T. ) ;
#48157 = CARTESIAN_POINT ( 'NONE',  ( -1.224655226406675013, -1.100228625579989572, 9.936700280135884356 ) ) ;
#48158 = CARTESIAN_POINT ( 'NONE',  ( 31.55402655318506788, 0.000000000000000000, 162.5682875569279702 ) ) ;
#48159 = CARTESIAN_POINT ( 'NONE',  ( -44.94597344681493922, 1.025126265847089213, -0.9317124430720324924 ) ) ;
#48160 =( BOUNDED_CURVE ( )  B_SPLINE_CURVE ( 3, ( #42802, #39998, #4584, #19722 ),
 .UNSPECIFIED., .F., .F. ) 
 B_SPLINE_CURVE_WITH_KNOTS ( ( 4, 4 ),
 ( 4.712388980384689674, 6.283185307179586232 ),
 .UNSPECIFIED. ) 
 CURVE ( )  GEOMETRIC_REPRESENTATION_ITEM ( )  RATIONAL_B_SPLINE_CURVE ( ( 1.000000000000000000, 0.8047378541243649375, 0.8047378541243649375, 1.000000000000000000 ) ) 
 REPRESENTATION_ITEM ( '' )  );
#48161 = VERTEX_POINT ( 'NONE', #4916 ) ;
#48162 = CARTESIAN_POINT ( 'NONE',  ( 210.0000000000000568, 0.000000000000000000, 40.81828755692798438 ) ) ;
#48163 = ORIENTED_EDGE ( 'NONE', *, *, #9821, .T. ) ;
#48164 = VERTEX_POINT ( 'NONE', #19550 ) ;
#48165 = AXIS2_PLACEMENT_3D ( 'NONE', #31170, #10894, #3701 ) ;
#48166 = EDGE_LOOP ( 'NONE', ( #3090, #12122, #14078, #5490 ) ) ;
#48167 = CARTESIAN_POINT ( 'NONE',  ( -168.4459734468149747, -1.025126265847089435, 39.06828755692797728 ) ) ;
#48168 = CARTESIAN_POINT ( 'NONE',  ( -13.35436367797847801, -31.26996044524040741, 7.906207997025717304 ) ) ;
#48169 = ORIENTED_EDGE ( 'NONE', *, *, #17825, .T. ) ;
#48170 = CARTESIAN_POINT ( 'NONE',  ( 0.000000000000000000, 13.98684210526316107, 0.000000000000000000 ) ) ;
#48171 = CARTESIAN_POINT ( 'NONE',  ( -126.6959734468149321, 0.000000000000000000, 165.0000000000000000 ) ) ;
#48172 = DIRECTION ( 'NONE',  ( 0.000000000000000000, 0.000000000000000000, -1.000000000000000000 ) ) ;
#48173 = CARTESIAN_POINT ( 'NONE',  ( 7.499999999999948486, -194.9999999999999716, -224.9999999999999716 ) ) ;
#48174 = CLOSED_SHELL ( 'NONE', ( #40023, #25865, #46774, #22738, #24966, #11457, #20739, #3859, #48415, #26293, #42685, #40024, #48416, #9571, #18741, #39688, #17423, #31390 ) ) ;
#48175 = ORIENTED_EDGE ( 'NONE', *, *, #1241, .F. ) ;
#48176 = CARTESIAN_POINT ( 'NONE',  ( 185.0000000000000000, -93.49999999999998579, -350.0000000000001705 ) ) ;
#48177 = VERTEX_POINT ( 'NONE', #15975 ) ;
#48178 = CARTESIAN_POINT ( 'NONE',  ( -214.9999999999999432, -173.0000000000000000, 352.0000000000000568 ) ) ;
#48179 = DIRECTION ( 'NONE',  ( -1.000000000000000000, 0.000000000000000000, -7.793956916774525800E-48 ) ) ;
#48180 = VERTEX_POINT ( 'NONE', #32382 ) ;
#48181 = ORIENTED_EDGE ( 'NONE', *, *, #14357, .F. ) ;
#48182 = DIRECTION ( 'NONE',  ( 6.203854594147707562E-25, -2.067951531382569187E-25, 1.000000000000000000 ) ) ;
#48183 = LINE ( 'NONE', #5379, #50378 ) ;
#48184 = B_SPLINE_SURFACE_WITH_KNOTS ( 'NONE', 3, 3, ( 
 ( #40120, #20098, #44435, #12646 ),
 ( #866, #36283, #47759, #16256 ),
 ( #28556, #27808, #47518, #36026 ),
 ( #40367, #44190, #23953, #1119 ) ),
 .UNSPECIFIED., .F., .F., .F.,
 ( 4, 4 ),
 ( 4, 4 ),
 ( 0.000000000000000000, 1.000000000000000000 ),
 ( 0.000000000000000000, 1.000000000000000000 ),
 .UNSPECIFIED. ) ;
#48185 = EDGE_LOOP ( 'NONE', ( #28551, #9065, #32980, #13631 ) ) ;
#48186 = LINE ( 'NONE', #5383, #45388 ) ;
#48187 = CARTESIAN_POINT ( 'NONE',  ( 210.0000000000000568, 2.143131898507881116E-16, -40.93171244307203693 ) ) ;
#48188 = CARTESIAN_POINT ( 'NONE',  ( -1.011271242968693862, 0.7347315653655780432, -3.333333333333333481 ) ) ;
#48189 = EDGE_CURVE ( 'NONE', #41782, #34169, #35874, .T. ) ;
#48190 = B_SPLINE_CURVE_WITH_KNOTS ( 'NONE', 3,
 ( #16978, #48475, #9522, #20316 ),
 .UNSPECIFIED., .F., .F.,
 ( 4, 4 ),
 ( 0.7491799374948681089, 1.000000000000000000 ),
 .UNSPECIFIED. ) ;
#48191 = EDGE_CURVE ( 'NONE', #13514, #40964, #47980, .T. ) ;
#48192 = EDGE_LOOP ( 'NONE', ( #33680, #3943, #25246, #37024 ) ) ;
#48193 = LINE ( 'NONE', #8499, #32696 ) ;
#48194 = CARTESIAN_POINT ( 'NONE',  ( -0.8813680857948604785, -1.919528421257472139, 9.884520316594375799 ) ) ;
#48195 = B_SPLINE_CURVE_WITH_KNOTS ( 'NONE', 3,
 ( #18538, #49295, #22151, #10093 ),
 .UNSPECIFIED., .F., .F.,
 ( 4, 4 ),
 ( 0.0004299334430849502051, 0.0007706806524480078798 ),
 .UNSPECIFIED. ) ;
#48196 = ADVANCED_FACE ( 'NONE', ( #21328 ), #13119, .T. ) ;
#48197 = FACE_OUTER_BOUND ( 'NONE', #28849, .T. ) ;
#48198 = ORIENTED_EDGE ( 'NONE', *, *, #42406, .T. ) ;
#48199 = VERTEX_POINT ( 'NONE', #40827 ) ;
#48200 = EDGE_CURVE ( 'NONE', #45415, #12448, #43928, .T. ) ;
#48201 = CONTEXT_DEPENDENT_SHAPE_REPRESENTATION ( #45943, #38894 ) ;
#48202 = VECTOR ( 'NONE', #6528, 1000.000000000000000 ) ;
#48203 = EDGE_CURVE ( 'NONE', #46968, #23694, #25357, .T. ) ;
#48204 = LINE ( 'NONE', #4885, #33540 ) ;
#48205 = CARTESIAN_POINT ( 'NONE',  ( 168.9999999999999716, -268.4999999999999432, -339.9999999999998863 ) ) ;
#48206 = VECTOR ( 'NONE', #40810, 1000.000000000000000 ) ;
#48207 = CARTESIAN_POINT ( 'NONE',  ( 181.0000000000000284, -9.999999999999953815, -113.0000000000001563 ) ) ;
#48208 = DIRECTION ( 'NONE',  ( -1.000000000000000000, -0.000000000000000000, -0.000000000000000000 ) ) ;
#48209 = ORIENTED_EDGE ( 'NONE', *, *, #29333, .T. ) ;
#48210 = AXIS2_PLACEMENT_3D ( 'NONE', #114, #27567, #27811 ) ;
#48211 = CIRCLE ( 'NONE', #28618, 2.000000000000001776 ) ;
#48212 = CARTESIAN_POINT ( 'NONE',  ( -165.0000000000000284, 16.00000000000000000, -114.9999999999999858 ) ) ;
#48213 = ADVANCED_FACE ( 'NONE', ( #1835 ), #5923, .T. ) ;
#48214 = DIRECTION ( 'NONE',  ( -0.8637789008984334549, 0.000000000000000000, 0.5038710255240862468 ) ) ;
#48215 = CARTESIAN_POINT ( 'NONE',  ( -84.94597344681493212, 1.025126265847089657, 79.06828755692797017 ) ) ;
#48216 = VECTOR ( 'NONE', #47444, 1000.000000000000000 ) ;
#48217 = LINE ( 'NONE', #48466, #21367 ) ;
#48218 = VECTOR ( 'NONE', #14116, 1000.000000000000000 ) ;
#48219 = ORIENTED_EDGE ( 'NONE', *, *, #23784, .F. ) ;
#48220 = DIRECTION ( 'NONE',  ( 0.000000000000000000, -0.000000000000000000, 1.000000000000000000 ) ) ;
#48221 = ORIENTED_EDGE ( 'NONE', *, *, #726, .T. ) ;
#48222 = CARTESIAN_POINT ( 'NONE',  ( 25.04522487443081502, -22.77512090857307925, 8.356839323120299312 ) ) ;
#48223 = ORIENTED_EDGE ( 'NONE', *, *, #48867, .T. ) ;
#48224 = DIRECTION ( 'NONE',  ( 0.000000000000000000, 0.000000000000000000, -1.000000000000000000 ) ) ;
#48225 = CARTESIAN_POINT ( 'NONE',  ( -204.9459734468148895, 1.025126265847089435, -157.4317124430720582 ) ) ;
#48226 = ORIENTED_EDGE ( 'NONE', *, *, #5443, .F. ) ;
#48227 = LINE ( 'NONE', #43651, #50668 ) ;
#48228 = VERTEX_POINT ( 'NONE', #36502 ) ;
#48229 = CARTESIAN_POINT ( 'NONE',  ( 0.8155877869298099325, 0.9072449372238458043, 9.963925895597341764 ) ) ;
#48230 = CARTESIAN_POINT ( 'NONE',  ( 1.150625731496811355, -0.4126014017553309987, 9.969517326150313608 ) ) ;
#48231 = CARTESIAN_POINT ( 'NONE',  ( -165.4943081650523027, 53.53801056904005407, -93.79675437945476801 ) ) ;
#48232 = FACE_OUTER_BOUND ( 'NONE', #49535, .T. ) ;
#48233 = VERTEX_POINT ( 'NONE', #24939 ) ;
#48234 = VERTEX_POINT ( 'NONE', #9281 ) ;
#48235 = CARTESIAN_POINT ( 'NONE',  ( 195.0540265531851105, 1.025126265847089435, -157.4317124430720582 ) ) ;
#48236 = ADVANCED_FACE ( 'NONE', ( #13627 ), #32637, .T. ) ;
#48237 = VECTOR ( 'NONE', #8878, 1000.000000000000000 ) ;
#48238 = VECTOR ( 'NONE', #46201, 1000.000000000000000 ) ;
#48239 = ORIENTED_EDGE ( 'NONE', *, *, #47001, .F. ) ;
#48240 = CARTESIAN_POINT ( 'NONE',  ( -64.99999999999815259, 16.00000000000000000, 65.00000000000000000 ) ) ;
#48241 = CARTESIAN_POINT ( 'NONE',  ( -124.9459734468149463, 2.143131898507847836E-16, -80.93171244307201562 ) ) ;
#48242 = LINE ( 'NONE', #44417, #49350 ) ;
#48243 =( BOUNDED_CURVE ( )  B_SPLINE_CURVE ( 3, ( #16888, #20986, #49572, #36406 ),
 .UNSPECIFIED., .F., .F. ) 
 B_SPLINE_CURVE_WITH_KNOTS ( ( 4, 4 ),
 ( 4.712388980384689674, 6.283185307179586232 ),
 .UNSPECIFIED. ) 
 CURVE ( )  GEOMETRIC_REPRESENTATION_ITEM ( )  RATIONAL_B_SPLINE_CURVE ( ( 1.000000000000000000, 0.8047378541243649375, 0.8047378541243649375, 1.000000000000000000 ) ) 
 REPRESENTATION_ITEM ( '' )  );
#48244 = ORIENTED_EDGE ( 'NONE', *, *, #21907, .F. ) ;
#48245 = DIRECTION ( 'NONE',  ( -0.000000000000000000, -1.000000000000000000, -0.000000000000000000 ) ) ;
#48246 = AXIS2_PLACEMENT_3D ( 'NONE', #27920, #32281, #43555 ) ;
#48247 = CIRCLE ( 'NONE', #8958, 2.000000000000001776 ) ;
#48248 = LINE ( 'NONE', #21862, #37414 ) ;
#48249 = DIRECTION ( 'NONE',  ( 1.000000000000000000, -0.000000000000000000, 0.000000000000000000 ) ) ;
#48250 = LINE ( 'NONE', #45166, #43131 ) ;
#48251 = FACE_OUTER_BOUND ( 'NONE', #17265, .T. ) ;
#48252 = CARTESIAN_POINT ( 'NONE',  ( -164.9999999999994031, 17.00000000000000000, -30.00000000000000000 ) ) ;
#48253 = ORIENTED_EDGE ( 'NONE', *, *, #31190, .F. ) ;
#48254 = ORIENTED_EDGE ( 'NONE', *, *, #39811, .F. ) ;
#48255 = VERTEX_POINT ( 'NONE', #29284 ) ;
#48256 = CARTESIAN_POINT ( 'NONE',  ( -0.04754753503590647412, 0.8311582663284536876, 9.985686052694765280 ) ) ;
#48257 = FACE_OUTER_BOUND ( 'NONE', #20391, .T. ) ;
#48258 = CARTESIAN_POINT ( 'NONE',  ( 385.4922279792745030, 0.000000000000000000, 224.8704663212433275 ) ) ;
#48259 = CARTESIAN_POINT ( 'NONE',  ( 342.8284271247460993, 167.0000000000001990, -342.0000000000002842 ) ) ;
#48260 = ORIENTED_EDGE ( 'NONE', *, *, #1451, .T. ) ;
#48261 = CARTESIAN_POINT ( 'NONE',  ( -46.69597344681494633, -1.750000000000010658, 80.81828755692798438 ) ) ;
#48262 = ORIENTED_EDGE ( 'NONE', *, *, #32443, .T. ) ;
#48263 =( LENGTH_UNIT ( ) NAMED_UNIT ( * ) SI_UNIT ( .MILLI., .METRE. ) );
#48264 = CARTESIAN_POINT ( 'NONE',  ( -7.576114424932982594, 50.00000000000000711, 7.906207997025717304 ) ) ;
#48265 = CARTESIAN_POINT ( 'NONE',  ( 1.401094519807298155, -0.7138523880601698179, 9.927288994922820464 ) ) ;
#48266 = CARTESIAN_POINT ( 'NONE',  ( 339.9999999999999432, -169.0000000000001137, -349.9999999999998863 ) ) ;
#48267 = FILL_AREA_STYLE_COLOUR ( '', #29912 ) ;
#48268 = CARTESIAN_POINT ( 'NONE',  ( -6.010192544690008631, 37.05120237258827132, 4.835783797351798974 ) ) ;
#48269 = CARTESIAN_POINT ( 'NONE',  ( -128.4459734468149463, 1.025126265847081442, -0.9317124430720195027 ) ) ;
#48270 = ORIENTED_EDGE ( 'NONE', *, *, #36226, .F. ) ;
#48271 = EDGE_CURVE ( 'NONE', #36396, #32219, #34143, .T. ) ;
#48272 = CYLINDRICAL_SURFACE ( 'NONE', #11628, 1.750000000000015543 ) ;
#48273 = DIRECTION ( 'NONE',  ( 1.000000000000000000, -0.000000000000000000, -0.000000000000000000 ) ) ;
#48274 = FACE_OUTER_BOUND ( 'NONE', #18568, .T. ) ;
#48275 = VECTOR ( 'NONE', #2329, 1000.000000000000000 ) ;
#48276 = VECTOR ( 'NONE', #33321, 1000.000000000000000 ) ;
#48277 = AXIS2_PLACEMENT_3D ( 'NONE', #6799, #26307, #30149 ) ;
#48278 = CARTESIAN_POINT ( 'NONE',  ( -168.4459734468149463, 0.000000000000000000, -0.9317124430720247208 ) ) ;
#48279 = ORIENTED_EDGE ( 'NONE', *, *, #37199, .T. ) ;
#48280 = DIRECTION ( 'NONE',  ( -0.000000000000000000, -0.000000000000000000, -1.000000000000000000 ) ) ;
#48281 = ORIENTED_EDGE ( 'NONE', *, *, #23675, .F. ) ;
#48282 = VECTOR ( 'NONE', #34114, 1000.000000000000000 ) ;
#48283 = LINE ( 'NONE', #21629, #42592 ) ;
#48284 = CARTESIAN_POINT ( 'NONE',  ( -15.00000000000001421, 17.00000000000000000, -114.9999999999999858 ) ) ;
#48285 = LINE ( 'NONE', #21131, #27967 ) ;
#48286 = ORIENTED_EDGE ( 'NONE', *, *, #2969, .T. ) ;
#48287 = VECTOR ( 'NONE', #6945, 1000.000000000000000 ) ;
#48288 = CARTESIAN_POINT ( 'NONE',  ( 22.69295089195473736, 45.31600496604706052, 7.455576670931136185 ) ) ;
#48289 = DIRECTION ( 'NONE',  ( -0.000000000000000000, -1.000000000000000000, -0.000000000000000000 ) ) ;
#48290 = CARTESIAN_POINT ( 'NONE',  ( -0.3862712429686895876, 1.188820645368940720, -3.333333333333333481 ) ) ;
#48291 = FACE_OUTER_BOUND ( 'NONE', #43428, .T. ) ;
#48292 = ORIENTED_EDGE ( 'NONE', *, *, #47660, .F. ) ;
#48293 = ORIENTED_EDGE ( 'NONE', *, *, #34192, .F. ) ;
#48294 = CARTESIAN_POINT ( 'NONE',  ( -5.990542248694146643, -8.025558178072376592, 3.215106848023455921 ) ) ;
#48295 = CARTESIAN_POINT ( 'NONE',  ( -48.44597344681495343, 0.000000000000000000, -157.4317124430720014 ) ) ;
#48296 = EDGE_CURVE ( 'NONE', #11814, #16962, #33497, .T. ) ;
#48297 =( BOUNDED_CURVE ( )  B_SPLINE_CURVE ( 3, ( #35936, #46914, #23869, #21 ),
 .UNSPECIFIED., .F., .F. ) 
 B_SPLINE_CURVE_WITH_KNOTS ( ( 4, 4 ),
 ( 4.712388980384689674, 6.283185307179586232 ),
 .UNSPECIFIED. ) 
 CURVE ( )  GEOMETRIC_REPRESENTATION_ITEM ( )  RATIONAL_B_SPLINE_CURVE ( ( 1.000000000000000000, 0.8047378541243649375, 0.8047378541243649375, 1.000000000000000000 ) ) 
 REPRESENTATION_ITEM ( '' )  );
#48298 = EDGE_LOOP ( 'NONE', ( #24937, #8150, #12708, #26776, #7094 ) ) ;
#48299 = ORIENTED_EDGE ( 'NONE', *, *, #4826, .F. ) ;
#48300 = FACE_OUTER_BOUND ( 'NONE', #27035, .T. ) ;
#48301 = CYLINDRICAL_SURFACE ( 'NONE', #26588, 1.750000000000001554 ) ;
#48302 = CARTESIAN_POINT ( 'NONE',  ( 14.52758583651987223, 8.922352469211173087, 8.953103998512858652 ) ) ;
#48303 = DIRECTION ( 'NONE',  ( -1.000000000000000000, 0.000000000000000000, 0.000000000000000000 ) ) ;
#48304 = ORIENTED_EDGE ( 'NONE', *, *, #3111, .T. ) ;
#48305 = VERTEX_POINT ( 'NONE', #25692 ) ;
#48306 = ORIENTED_EDGE ( 'NONE', *, *, #23972, .T. ) ;
#48307 =( BOUNDED_CURVE ( )  B_SPLINE_CURVE ( 3, ( #38006, #37757, #10033, #50237 ),
 .UNSPECIFIED., .F., .F. ) 
 B_SPLINE_CURVE_WITH_KNOTS ( ( 4, 4 ),
 ( 0.000000000000000000, 1.570796326794896558 ),
 .UNSPECIFIED. ) 
 CURVE ( )  GEOMETRIC_REPRESENTATION_ITEM ( )  RATIONAL_B_SPLINE_CURVE ( ( 1.000000000000000000, 0.8047378541243649375, 0.8047378541243649375, 1.000000000000000000 ) ) 
 REPRESENTATION_ITEM ( '' )  );
#48308 = VECTOR ( 'NONE', #3726, 1000.000000000000000 ) ;
#48309 = DIRECTION ( 'NONE',  ( 0.000000000000000000, 1.000000000000000000, -0.000000000000000000 ) ) ;
#48310 = VECTOR ( 'NONE', #12421, 1000.000000000000000 ) ;
#48311 = CARTESIAN_POINT ( 'NONE',  ( 210.0000000000000568, 2.143131898507881856E-16, -80.93171244307202983 ) ) ;
#48312 = VECTOR ( 'NONE', #31372, 1000.000000000000000 ) ;
#48313 = VECTOR ( 'NONE', #26351, 1000.000000000000000 ) ;
#48314 = VERTEX_POINT ( 'NONE', #41085 ) ;
#48315 = EDGE_LOOP ( 'NONE', ( #48747, #46691, #6338, #17548, #22889, #3935 ) ) ;
#48316 = VECTOR ( 'NONE', #37409, 1000.000000000000000 ) ;
#48317 = DIRECTION ( 'NONE',  ( -1.000000000000000000, -0.000000000000000000, -0.000000000000000000 ) ) ;
#48318 = VECTOR ( 'NONE', #13589, 1000.000000000000000 ) ;
#48319 = CARTESIAN_POINT ( 'NONE',  ( 164.9999999999999716, -168.9999999999999432, -340.0000000000001137 ) ) ;
#48320 = ORIENTED_EDGE ( 'NONE', *, *, #47467, .F. ) ;
#48321 = ORIENTED_EDGE ( 'NONE', *, *, #2080, .F. ) ;
#48322 = CARTESIAN_POINT ( 'NONE',  ( 16.52264463346132572, -2.779753662172757878, 9.403735324607438884 ) ) ;
#48323 = VERTEX_POINT ( 'NONE', #44404 ) ;
#48324 = CARTESIAN_POINT ( 'NONE',  ( 164.9999999999999716, 174.9999999999999716, -340.0000000000001137 ) ) ;
#48325 = VECTOR ( 'NONE', #6625, 1000.000000000000000 ) ;
#48326 = LINE ( 'NONE', #9123, #26247 ) ;
#48327 = CARTESIAN_POINT ( 'NONE',  ( -0.2050626648094178439, 1.807624707194796843, 9.903764339332081335 ) ) ;
#48328 = CARTESIAN_POINT ( 'NONE',  ( 168.9999999999999716, -79.49999999999995737, -115.0000000000001563 ) ) ;
#48329 = CARTESIAN_POINT ( 'NONE',  ( -207.7210997126620384, 1.750000000000009548, -40.20683870891912193 ) ) ;
#48330 = ORIENTED_EDGE ( 'NONE', *, *, #34919, .F. ) ;
#48331 = EDGE_CURVE ( 'NONE', #17293, #30248, #11495, .T. ) ;
#48332 = FACE_OUTER_BOUND ( 'NONE', #20806, .T. ) ;
#48333 = FACE_OUTER_BOUND ( 'NONE', #45193, .T. ) ;
#48334 = CARTESIAN_POINT ( 'NONE',  ( -1.642172164747307761, 3.377809768366639828E-15, -27.58190990837850265 ) ) ;
#48335 = CARTESIAN_POINT ( 'NONE',  ( 168.9999999999999716, -184.9999999999999716, -340.0000000000001705 ) ) ;
#48336 = FACE_OUTER_BOUND ( 'NONE', #13815, .T. ) ;
#48337 = EDGE_CURVE ( 'NONE', #23318, #46337, #17233, .T. ) ;
#48338 = EDGE_CURVE ( 'NONE', #48435, #27161, #41333, .T. ) ;
#48339 = CARTESIAN_POINT ( 'NONE',  ( -164.4973046169135955, -61.66198943095990614, -18.45589678844777382 ) ) ;
#48340 = CYLINDRICAL_SURFACE ( 'NONE', #48392, 1.750000000000001554 ) ;
#48341 = AXIS2_PLACEMENT_3D ( 'NONE', #698, #27909, #43535 ) ;
#48342 = EDGE_CURVE ( 'NONE', #7126, #20602, #2330, .T. ) ;
#48343 = EDGE_LOOP ( 'NONE', ( #9198, #32378, #3768, #50134 ) ) ;
#48344 = CARTESIAN_POINT ( 'NONE',  ( -22.69295089195507487, -45.31600496604688999, 7.455576670931136185 ) ) ;
#48345 = VECTOR ( 'NONE', #40399, 1000.000000000000000 ) ;
#48346 = DIRECTION ( 'NONE',  ( 0.000000000000000000, -0.000000000000000000, -1.000000000000000000 ) ) ;
#48347 = DIRECTION ( 'NONE',  ( -1.000000000000000000, 0.000000000000000000, 0.000000000000000000 ) ) ;
#48348 = DIRECTION ( 'NONE',  ( -1.000000000000000000, -0.000000000000000000, -0.000000000000000000 ) ) ;
#48349 = LINE ( 'NONE', #33513, #27458 ) ;
#48350 =( GEOMETRIC_REPRESENTATION_CONTEXT ( 3 ) GLOBAL_UNCERTAINTY_ASSIGNED_CONTEXT ( ( #19173 ) ) GLOBAL_UNIT_ASSIGNED_CONTEXT ( ( #49131, #49631, #10178 ) ) REPRESENTATION_CONTEXT ( 'NONE', 'WORKASPACE' ) );
#48351 = ORIENTED_EDGE ( 'NONE', *, *, #18172, .F. ) ;
#48352 = DIRECTION ( 'NONE',  ( -1.000000000000000000, 0.000000000000000000, 0.000000000000000000 ) ) ;
#48353 = VECTOR ( 'NONE', #47901, 1000.000000000000000 ) ;
#48354 = EDGE_CURVE ( 'NONE', #15591, #36272, #48973, .T. ) ;
#48356 = VERTEX_POINT ( 'NONE', #38271 ) ;
#48355 = EDGE_CURVE ( 'NONE', #21998, #9239, #37268, .T. ) ;
#48357 = CARTESIAN_POINT ( 'NONE',  ( 1.250000000000000222, 0.000000000000000000, -3.333333333333333481 ) ) ;
#48358 = EDGE_CURVE ( 'NONE', #45714, #45821, #49868, .T. ) ;
#48359 = EDGE_CURVE ( 'NONE', #42474, #23347, #22084, .T. ) ;
#48360 = VERTEX_POINT ( 'NONE', #11559 ) ;
#48361 = DIRECTION ( 'NONE',  ( -1.586032892321652236E-16, -1.000000000000000000, -2.288264760618012091E-48 ) ) ;
#48362 = CARTESIAN_POINT ( 'NONE',  ( -167.7210997126620384, -1.750000000000009548, -0.2068387089191121020 ) ) ;
#48363 = ORIENTED_EDGE ( 'NONE', *, *, #28156, .F. ) ;
#48364 = ORIENTED_EDGE ( 'NONE', *, *, #33151, .T. ) ;
#48365 = EDGE_CURVE ( 'NONE', #18303, #1528, #23090, .T. ) ;
#48366 = CARTESIAN_POINT ( 'NONE',  ( 0.000000000000000000, -184.7999999999999545, -340.2000000000001592 ) ) ;
#48367 = CARTESIAN_POINT ( 'NONE',  ( -0.8285222815141961572, -1.889008401827320771, 9.886433018048073507 ) ) ;
#48368 = CARTESIAN_POINT ( 'NONE',  ( -6.695973446814940111, -1.750000000000023315, -159.1817124430720298 ) ) ;
#48369 = CARTESIAN_POINT ( 'NONE',  ( -15.73090589902298042, -29.60029367929041655, 1.847720168420772691 ) ) ;
#48370 = ORIENTED_EDGE ( 'NONE', *, *, #15235, .F. ) ;
#48371 = CARTESIAN_POINT ( 'NONE',  ( -177.4999999999999716, 112.5000000000000000, -10.00000000000000000 ) ) ;
#48372 =( NAMED_UNIT ( * ) SI_UNIT ( $, .STERADIAN. ) SOLID_ANGLE_UNIT ( ) );
#48373 = ORIENTED_EDGE ( 'NONE', *, *, #50014, .F. ) ;
#48374 = ORIENTED_EDGE ( 'NONE', *, *, #10521, .T. ) ;
#48375 = ORIENTED_EDGE ( 'NONE', *, *, #39961, .T. ) ;
#48376 = LINE ( 'NONE', #12509, #42598 ) ;
#48377 = DIRECTION ( 'NONE',  ( 0.000000000000000000, 0.000000000000000000, -1.000000000000000000 ) ) ;
#48378 = ORIENTED_EDGE ( 'NONE', *, *, #48191, .F. ) ;
#48379 = EDGE_CURVE ( 'NONE', #17305, #12755, #4397, .T. ) ;
#48380 = DIRECTION ( 'NONE',  ( 0.000000000000000000, 0.000000000000000000, -1.000000000000000000 ) ) ;
#48381 = CARTESIAN_POINT ( 'NONE',  ( 164.9999999999999716, 16.00000000000000000, 115.0000000000000142 ) ) ;
#48382 = EDGE_CURVE ( 'NONE', #405, #41804, #46146, .T. ) ;
#48383 = CARTESIAN_POINT ( 'NONE',  ( 112.2789002873379758, -1.749999999999996669, -158.1565861772249377 ) ) ;
#48384 = CARTESIAN_POINT ( 'NONE',  ( -88.44597344681497475, 0.000000000000000000, -157.4317124430720014 ) ) ;
#48385 = ADVANCED_FACE ( 'NONE', ( #15145 ), #18720, .F. ) ;
#48386 = DIRECTION ( 'NONE',  ( 0.000000000000000000, 0.000000000000000000, 1.000000000000000000 ) ) ;
#48387 = CARTESIAN_POINT ( 'NONE',  ( 8.843309649387377291, -14.11631751497145792, -2.870787844569587133 ) ) ;
#48388 = ADVANCED_FACE ( 'NONE', ( #50238 ), #37758, .T. ) ;
#48389 = VECTOR ( 'NONE', #28131, 1000.000000000000000 ) ;
#48390 = CARTESIAN_POINT ( 'NONE',  ( -64.99999999999846523, 17.00000000000000000, 35.00000000000000000 ) ) ;
#48391 = CARTESIAN_POINT ( 'NONE',  ( -88.44597344681494633, -1.025126265847089435, -157.4317124430720582 ) ) ;
#48392 = AXIS2_PLACEMENT_3D ( 'NONE', #20422, #24540, #1947 ) ;
#48393 = DIRECTION ( 'NONE',  ( 0.000000000000000000, 0.000000000000000000, 1.000000000000000000 ) ) ;
#48394 = EDGE_CURVE ( 'NONE', #23844, #15960, #21759, .T. ) ;
#48395 = CYLINDRICAL_SURFACE ( 'NONE', #15057, 1.750000000000010214 ) ;
#48396 = PLANE ( 'NONE',  #13438 ) ;
#48397 = ORIENTED_EDGE ( 'NONE', *, *, #482, .F. ) ;
#48398 = CARTESIAN_POINT ( 'NONE',  ( -567.5000000000000000, 57.49999999999996447, -183.5999999999997954 ) ) ;
#48399 = FACE_OUTER_BOUND ( 'NONE', #32327, .T. ) ;
#48400 = LINE ( 'NONE', #24362, #43042 ) ;
#48401 = DIRECTION ( 'NONE',  ( 0.000000000000000000, 0.000000000000000000, 1.000000000000000000 ) ) ;
#48402 = EDGE_LOOP ( 'NONE', ( #37533, #42834 ) ) ;
#48403 = CYLINDRICAL_SURFACE ( 'NONE', #22377, 1.750000000000015543 ) ;
#48404 = CARTESIAN_POINT ( 'NONE',  ( -208.4459734468149463, 0.000000000000000000, 165.0000000000000000 ) ) ;
#48405 = EDGE_CURVE ( 'NONE', #48120, #30382, #46947, .T. ) ;
#48406 = EDGE_LOOP ( 'NONE', ( #3411, #7767, #37318, #50454, #47348 ) ) ;
#48407 = CARTESIAN_POINT ( 'NONE',  ( -10.92344319659207663, -12.63397777816690315, -9.458680755252684591 ) ) ;
#48408 = LINE ( 'NONE', #44334, #39921 ) ;
#48409 = AXIS2_PLACEMENT_3D ( 'NONE', #37987, #21463, #21974 ) ;
#48410 = VERTEX_POINT ( 'NONE', #26192 ) ;
#48411 = DIRECTION ( 'NONE',  ( -1.000000000000000000, -0.000000000000000000, -0.000000000000000000 ) ) ;
#48412 = ORIENTED_EDGE ( 'NONE', *, *, #23522, .T. ) ;
#48413 = ORIENTED_EDGE ( 'NONE', *, *, #43412, .F. ) ;
#48414 = VECTOR ( 'NONE', #33307, 1000.000000000000000 ) ;
#48415 = ADVANCED_FACE ( 'NONE', ( #46660 ), #38515, .T. ) ;
#48416 = ADVANCED_FACE ( 'NONE', ( #26435 ), #30052, .T. ) ;
#48417 = VERTEX_POINT ( 'NONE', #42079 ) ;
#48418 = DIRECTION ( 'NONE',  ( 0.000000000000000000, 0.000000000000000000, 1.000000000000000000 ) ) ;
#48419 = CYLINDRICAL_SURFACE ( 'NONE', #37203, 1.750000000000008438 ) ;
#48420 = VERTEX_POINT ( 'NONE', #50499 ) ;
#48421 = PLANE ( 'NONE',  #46685 ) ;
#48422 = EDGE_CURVE ( 'NONE', #22675, #13610, #22331, .T. ) ;
#48423 = DIRECTION ( 'NONE',  ( 0.000000000000000000, 0.000000000000000000, 1.000000000000000000 ) ) ;
#48424 = EDGE_CURVE ( 'NONE', #2839, #2472, #6942, .T. ) ;
#48425 = VECTOR ( 'NONE', #44213, 1000.000000000000000 ) ;
#48426 = CARTESIAN_POINT ( 'NONE',  ( 1.011271242968683648, 0.7347315653655930312, -10.00000000000000000 ) ) ;
#48427 = ORIENTED_EDGE ( 'NONE', *, *, #43976, .F. ) ;
#48428 = EDGE_CURVE ( 'NONE', #1177, #19922, #34660, .T. ) ;
#48429 = FACE_OUTER_BOUND ( 'NONE', #36369, .T. ) ;
#48430 = ORIENTED_EDGE ( 'NONE', *, *, #12158, .T. ) ;
#48431 = CARTESIAN_POINT ( 'NONE',  ( 151.5540265531850537, 0.000000000000000000, 165.0000000000000000 ) ) ;
#48432 = DIRECTION ( 'NONE',  ( -1.000000000000000000, -0.000000000000000000, -0.000000000000000000 ) ) ;
#48433 = VERTEX_POINT ( 'NONE', #46413 ) ;
#48434 = EDGE_LOOP ( 'NONE', ( #39409, #8009, #36601, #908, #36034, #36834, #35073, #14055, #11377, #44529, #3275, #41720, #224, #19044, #37031, #40667, #3614, #11489, #8671, #17373, #44525, #8797, #13874, #25423, #6524, #4931, #20404, #44540, #45208, #45052, #43373, #41765 ) ) ;
#48435 = VERTEX_POINT ( 'NONE', #11300 ) ;
#48436 = DIRECTION ( 'NONE',  ( -0.000000000000000000, -0.000000000000000000, -1.000000000000000000 ) ) ;
#48437 = CARTESIAN_POINT ( 'NONE',  ( 30.00000000000062172, 17.00000000000000000, -30.00000000000000000 ) ) ;
#48438 = ORIENTED_EDGE ( 'NONE', *, *, #25288, .F. ) ;
#48439 = DIRECTION ( 'NONE',  ( -0.000000000000000000, -0.000000000000000000, 1.000000000000000000 ) ) ;
#48440 = LINE ( 'NONE', #28988, #7431 ) ;
#48441 =( BOUNDED_CURVE ( )  B_SPLINE_CURVE ( 3, ( #16415, #40778, #32079, #47423 ),
 .UNSPECIFIED., .F., .F. ) 
 B_SPLINE_CURVE_WITH_KNOTS ( ( 4, 4 ),
 ( 4.712388980384689674, 6.283185307179586232 ),
 .UNSPECIFIED. ) 
 CURVE ( )  GEOMETRIC_REPRESENTATION_ITEM ( )  RATIONAL_B_SPLINE_CURVE ( ( 1.000000000000000000, 0.8047378541243649375, 0.8047378541243649375, 1.000000000000000000 ) ) 
 REPRESENTATION_ITEM ( '' )  );
#48443 = B_SPLINE_CURVE_WITH_KNOTS ( 'NONE', 3,
 ( #7395, #23021, #20957, #28648 ),
 .UNSPECIFIED., .F., .F.,
 ( 4, 4 ),
 ( 6.459821870315384563E-06, 0.0003472038099299140732 ),
 .UNSPECIFIED. ) ;
#48442 = CARTESIAN_POINT ( 'NONE',  ( -208.4459734468149463, 0.000000000000000000, 165.0000000000000000 ) ) ;
#48444 = ADVANCED_FACE ( 'NONE', ( #38763 ), #3589, .T. ) ;
#48445 = ORIENTED_EDGE ( 'NONE', *, *, #45717, .F. ) ;
#48446 = DIRECTION ( 'NONE',  ( 0.000000000000000000, -1.000000000000000000, 0.000000000000000000 ) ) ;
#48447 = CARTESIAN_POINT ( 'NONE',  ( 50.00000000000000000, -50.00000000000000000, 800.0000000000000000 ) ) ;
#48448 =( BOUNDED_CURVE ( )  B_SPLINE_CURVE ( 3, ( #3214, #18863, #34545, #50128 ),
 .UNSPECIFIED., .F., .F. ) 
 B_SPLINE_CURVE_WITH_KNOTS ( ( 4, 4 ),
 ( 0.000000000000000000, 1.570796326794896558 ),
 .UNSPECIFIED. ) 
 CURVE ( )  GEOMETRIC_REPRESENTATION_ITEM ( )  RATIONAL_B_SPLINE_CURVE ( ( 1.000000000000000000, 0.8047378541243649375, 0.8047378541243649375, 1.000000000000000000 ) ) 
 REPRESENTATION_ITEM ( '' )  );
#48449 = AXIS2_PLACEMENT_3D ( 'NONE', #6452, #22352, #14658 ) ;
#48450 = CARTESIAN_POINT ( 'NONE',  ( 74.32915281903215998, 1.750000000000010214, -118.1565861772249519 ) ) ;
#48451 = PRODUCT_DEFINITION ( 'UNKNOWN', '', #6196, #47257 ) ;
#48452 = ORIENTED_EDGE ( 'NONE', *, *, #2614, .T. ) ;
#48453 = ORIENTED_EDGE ( 'NONE', *, *, #44635, .F. ) ;
#48454 = ITEM_DEFINED_TRANSFORMATION ( 'NONE', 'NONE', #29921,  #45486 ) ;
#48455 = DIRECTION ( 'NONE',  ( 1.000000000000000000, 0.000000000000000000, 0.000000000000000000 ) ) ;
#48456 = CARTESIAN_POINT ( 'NONE',  ( 298.7932379171858770, 232.7719218785460953, 296.3011729072026128 ) ) ;
#48457 = VECTOR ( 'NONE', #46697, 1000.000000000000000 ) ;
#48458 = FACE_OUTER_BOUND ( 'NONE', #8151, .T. ) ;
#48459 = CARTESIAN_POINT ( 'NONE',  ( -15.98719783915689163, 4.501063718205989161, 3.266473740018926541 ) ) ;
#48460 = ORIENTED_EDGE ( 'NONE', *, *, #50402, .T. ) ;
#48461 = LINE ( 'NONE', #18199, #40297 ) ;
#48462 = EDGE_CURVE ( 'NONE', #33627, #40517, #39021, .T. ) ;
#48463 =( BOUNDED_CURVE ( )  B_SPLINE_CURVE ( 3, ( #1113, #8560, #39872, #4706 ),
 .UNSPECIFIED., .F., .F. ) 
 B_SPLINE_CURVE_WITH_KNOTS ( ( 4, 4 ),
 ( 1.570796326794896558, 3.141592653589793116 ),
 .UNSPECIFIED. ) 
 CURVE ( )  GEOMETRIC_REPRESENTATION_ITEM ( )  RATIONAL_B_SPLINE_CURVE ( ( 1.000000000000000000, 0.8047378541243649375, 0.8047378541243649375, 1.000000000000000000 ) ) 
 REPRESENTATION_ITEM ( '' )  );
#48464 = CARTESIAN_POINT ( 'NONE',  ( 210.0000000000000568, 0.000000000000000000, 40.81828755692798438 ) ) ;
#48465 = DIRECTION ( 'NONE',  ( 4.996003610813203446E-16, 1.000000000000000000, 0.000000000000000000 ) ) ;
#48466 = CARTESIAN_POINT ( 'NONE',  ( 7.500000000000000000, 224.9999999999999716, -224.9999999999999716 ) ) ;
#48467 = ORIENTED_EDGE ( 'NONE', *, *, #17860, .T. ) ;
#48468 = CARTESIAN_POINT ( 'NONE',  ( 0.1530804384059059886, -1.323112372395012448, 9.951893257060014264 ) ) ;
#48469 = ORIENTED_EDGE ( 'NONE', *, *, #47916, .F. ) ;
#48470 = VERTEX_POINT ( 'NONE', #4366 ) ;
#48471 = LINE ( 'NONE', #13360, #32002 ) ;
#48472 = LINE ( 'NONE', #36490, #47024 ) ;
#48473 = VERTEX_POINT ( 'NONE', #8218 ) ;
#48474 = EDGE_CURVE ( 'NONE', #28356, #3794, #47640, .T. ) ;
#48475 = CARTESIAN_POINT ( 'NONE',  ( 22.50630130403698459, -35.09254592550291818, -9.387872844313825738 ) ) ;
#48476 = EDGE_CURVE ( 'NONE', #3985, #30782, #42430, .T. ) ;
#48477 = ORIENTED_EDGE ( 'NONE', *, *, #13130, .T. ) ;
#48478 = LINE ( 'NONE', #13372, #41753 ) ;
#48479 = CARTESIAN_POINT ( 'NONE',  ( 21.23829395927641883, 7.611558401714507482, 230.0000000000000000 ) ) ;
#48480 = VECTOR ( 'NONE', #14792, 1000.000000000000000 ) ;
#48481 = DIRECTION ( 'NONE',  ( 0.000000000000000000, -0.2223603367690619725, -0.9749645535258958384 ) ) ;
#48482 = CARTESIAN_POINT ( 'NONE',  ( 357.9999999999999432, -174.9999999999999716, 355.9999999999998295 ) ) ;
#48483 = AXIS2_PLACEMENT_3D ( 'NONE', #11903, #30909, #38859 ) ;
#48484 = DIRECTION ( 'NONE',  ( -1.000000000000000000, -0.000000000000000000, -0.000000000000000000 ) ) ;
#48485 = VERTEX_POINT ( 'NONE', #23864 ) ;
#48486 = ADVANCED_FACE ( 'NONE', ( #24378 ), #31579, .T. ) ;
#48487 = ORIENTED_EDGE ( 'NONE', *, *, #38399, .T. ) ;
#48488 = PLANE ( 'NONE',  #9519 ) ;
#48489 = EDGE_CURVE ( 'NONE', #38537, #18600, #47920, .T. ) ;
#48490 = EDGE_CURVE ( 'NONE', #14175, #35777, #35688, .T. ) ;
#48491 = VERTEX_POINT ( 'NONE', #23349 ) ;
#48492 = AXIS2_PLACEMENT_3D ( 'NONE', #26573, #34802, #34533 ) ;
#48493 = PLANE ( 'NONE',  #16100 ) ;
#48494 = CARTESIAN_POINT ( 'NONE',  ( 31.55402655318503236, 0.000000000000000000, -157.4317124430720014 ) ) ;
#48495 = EDGE_LOOP ( 'NONE', ( #35784, #6843, #1782, #42581 ) ) ;
#48496 = CARTESIAN_POINT ( 'NONE',  ( -33.89193117067293315, 33.89193117067293315, 910.0000000000000000 ) ) ;
#48497 = EDGE_CURVE ( 'NONE', #47734, #27082, #28966, .T. ) ;
#48498 = DIRECTION ( 'NONE',  ( -1.000000000000000000, -0.000000000000000000, -0.000000000000000000 ) ) ;
#48499 = ORIENTED_EDGE ( 'NONE', *, *, #2946, .F. ) ;
#48500 = CYLINDRICAL_SURFACE ( 'NONE', #10414, 1.750000000000015543 ) ;
#48501 = CARTESIAN_POINT ( 'NONE',  ( -206.6959734468149463, -1.750000000000010658, 120.8182875569279702 ) ) ;
#48502 = CARTESIAN_POINT ( 'NONE',  ( 35.05402655318504657, -1.025126265847088991, 159.0682875569279418 ) ) ;
#48503 = FACE_OUTER_BOUND ( 'NONE', #22681, .T. ) ;
#48504 = ORIENTED_EDGE ( 'NONE', *, *, #28650, .F. ) ;
#48505 = ORIENTED_EDGE ( 'NONE', *, *, #7214, .F. ) ;
#48506 = ORIENTED_EDGE ( 'NONE', *, *, #8504, .T. ) ;
#48507 = CARTESIAN_POINT ( 'NONE',  ( -127.7210997126620242, 1.749999999999997113, 119.7931612910809065 ) ) ;
#48508 = LINE ( 'NONE', #29311, #25902 ) ;
#48509 = CARTESIAN_POINT ( 'NONE',  ( 168.9999999999999716, -9.999999999999953815, -350.0000000000001705 ) ) ;
#48510 = CIRCLE ( 'NONE', #21481, 0.5000000000000004441 ) ;
#48511 = DIRECTION ( 'NONE',  ( 1.156482317317870492E-16, -1.000000000000000000, 0.000000000000000000 ) ) ;
#48512 = ORIENTED_EDGE ( 'NONE', *, *, #17196, .F. ) ;
#48513 = CARTESIAN_POINT ( 'NONE',  ( -1.780619886013952602, -1.041246721325602920, 9.886433018048069954 ) ) ;
#48514 = ORIENTED_EDGE ( 'NONE', *, *, #41008, .T. ) ;
#48515 = CARTESIAN_POINT ( 'NONE',  ( -86.69597344681494633, 1.750000000000010658, -79.18171244307201562 ) ) ;
#48516 = CARTESIAN_POINT ( 'NONE',  ( -69.99999999999940314, 17.00000000000000000, -54.99999999999999289 ) ) ;
#48517 = CARTESIAN_POINT ( 'NONE',  ( 0.000000000000000000, 169.0000000000000000, 343.9999999999997726 ) ) ;
#48518 = DIRECTION ( 'NONE',  ( 0.000000000000000000, -1.000000000000000000, 0.000000000000000000 ) ) ;
#48519 = CARTESIAN_POINT ( 'NONE',  ( 35.00000000000091660, 17.00000000000000000, 0.000000000000000000 ) ) ;
#48520 = VECTOR ( 'NONE', #7042, 1000.000000000000000 ) ;
#48521 = CARTESIAN_POINT ( 'NONE',  ( 210.0000000000000568, 2.143131898507880377E-16, -0.9317124430720331585 ) ) ;
#48522 = ORIENTED_EDGE ( 'NONE', *, *, #10583, .T. ) ;
#48523 = FACE_OUTER_BOUND ( 'NONE', #5697, .T. ) ;
#48524 = AXIS2_PLACEMENT_3D ( 'NONE', #32554, #48137, #21737 ) ;
#48525 = PLANE ( 'NONE',  #45756 ) ;
#48526 = LINE ( 'NONE', #13413, #46242 ) ;
#48527 = EDGE_CURVE ( 'NONE', #41913, #9256, #47663, .T. ) ;
#48528 = CARTESIAN_POINT ( 'NONE',  ( -0.7601424845489993531, 1.297311920617006065, 9.927319414211224213 ) ) ;
#48530 = ORIENTED_EDGE ( 'NONE', *, *, #27439, .T. ) ;
#48529 = B_SPLINE_CURVE_WITH_KNOTS ( 'NONE', 3,
 ( #30958, #16743, #3470, #1356 ),
 .UNSPECIFIED., .F., .F.,
 ( 4, 4 ),
 ( 5.033378918613206543E-16, 0.009782300387714822770 ),
 .UNSPECIFIED. ) ;
#48531 = VECTOR ( 'NONE', #18257, 1000.000000000000000 ) ;
#48532 = CARTESIAN_POINT ( 'NONE',  ( -164.9999999999987779, 17.00000000000000000, 30.00000000000000000 ) ) ;
#48533 = EDGE_LOOP ( 'NONE', ( #12772, #38412, #1537, #26954, #18342, #33991 ) ) ;
#48534 = CARTESIAN_POINT ( 'NONE',  ( 1.962712821592840662, 1.022159834731142691, 9.881002359080275355 ) ) ;
#48535 = LINE ( 'NONE', #5982, #41384 ) ;
#48536 = CARTESIAN_POINT ( 'NONE',  ( 192.2789002873380184, 1.750000000000009326, 1.843413822775066269 ) ) ;
#48537 = ORIENTED_EDGE ( 'NONE', *, *, #30976, .T. ) ;
#48538 = ORIENTED_EDGE ( 'NONE', *, *, #32289, .F. ) ;
#48539 = EDGE_CURVE ( 'NONE', #38121, #21871, #7713, .T. ) ;
#48540 = DIRECTION ( 'NONE',  ( -1.000000000000000000, 0.000000000000000000, -0.000000000000000000 ) ) ;
#48541 = VECTOR ( 'NONE', #422, 1000.000000000000000 ) ;
#48542 = CARTESIAN_POINT ( 'NONE',  ( 35.00000000000091660, 17.00000000000000000, 0.000000000000000000 ) ) ;
#48543 =( BOUNDED_CURVE ( )  B_SPLINE_CURVE ( 3, ( #29621, #6285, #24837, #13958 ),
 .UNSPECIFIED., .F., .F. ) 
 B_SPLINE_CURVE_WITH_KNOTS ( ( 4, 4 ),
 ( 0.2242347511090958534, 1.570796326794895670 ),
 .UNSPECIFIED. ) 
 CURVE ( )  GEOMETRIC_REPRESENTATION_ITEM ( )  RATIONAL_B_SPLINE_CURVE ( ( 1.000000000000000000, 0.8545200852688803472, 0.8545200852688803472, 1.000000000000000000 ) ) 
 REPRESENTATION_ITEM ( '' )  );
#48544 = CARTESIAN_POINT ( 'NONE',  ( 356.0000000000000000, -165.0000000000001137, -340.0000000000002842 ) ) ;
#48545 = CARTESIAN_POINT ( 'NONE',  ( -19.99999999999908695, 16.00000000000000000, -24.99999999999999289 ) ) ;
#48546 = VERTEX_POINT ( 'NONE', #16168 ) ;
#48547 = ORIENTED_EDGE ( 'NONE', *, *, #28133, .F. ) ;
#48548 = CARTESIAN_POINT ( 'NONE',  ( -0.6440276692615867216, -16.64212148744554298, -9.683996418299976483 ) ) ;
#48549 = CARTESIAN_POINT ( 'NONE',  ( -19.99999999999878142, 16.00000000000000000, 30.00000000000000000 ) ) ;
#48550 = EDGE_CURVE ( 'NONE', #48323, #16118, #37232, .T. ) ;
#48551 = EDGE_CURVE ( 'NONE', #29454, #28520, #47415, .T. ) ;
#48552 = ORIENTED_EDGE ( 'NONE', *, *, #16445, .F. ) ;
#48553 = VERTEX_POINT ( 'NONE', #12303 ) ;
#48554 = CARTESIAN_POINT ( 'NONE',  ( 185.0000000000000000, -168.9999999999999432, -350.0000000000001705 ) ) ;
#48555 = CARTESIAN_POINT ( 'NONE',  ( 1.589327968330908281, 0.05051906867692627923, 9.933337059263775970 ) ) ;
#48556 = CARTESIAN_POINT ( 'NONE',  ( 181.0000000000000000, -7.999999999999952038, -350.0000000000001705 ) ) ;
#48557 = AXIS2_PLACEMENT_3D ( 'NONE', #27647, #11236, #15585 ) ;
#48558 = DIRECTION ( 'NONE',  ( -0.000000000000000000, -1.544785076050074834E-48, -1.000000000000000000 ) ) ;
#48559 = APPLICATION_CONTEXT ( 'automotive_design' ) ;
#48560 = EDGE_LOOP ( 'NONE', ( #45778, #49480, #24113, #6481 ) ) ;
#48561 = ORIENTED_EDGE ( 'NONE', *, *, #20893, .F. ) ;
#48562 = EDGE_CURVE ( 'NONE', #40406, #27344, #7382, .T. ) ;
#48563 = VERTEX_POINT ( 'NONE', #15653 ) ;
#48564 = VECTOR ( 'NONE', #41249, 1000.000000000000000 ) ;
#48565 = FACE_OUTER_BOUND ( 'NONE', #27804, .T. ) ;
#48566 = CARTESIAN_POINT ( 'NONE',  ( -15.00000000000000000, -46.01315789473684248, -5.916985404131814619 ) ) ;
#48567 = VECTOR ( 'NONE', #27942, 1000.000000000000000 ) ;
#48568 = ORIENTED_EDGE ( 'NONE', *, *, #50528, .F. ) ;
#48569 = ORIENTED_EDGE ( 'NONE', *, *, #11722, .F. ) ;
#48570 = DIRECTION ( 'NONE',  ( -0.000000000000000000, -0.000000000000000000, -1.000000000000000000 ) ) ;
#48571 = CARTESIAN_POINT ( 'NONE',  ( 1.540662627795932105, -1.371465786296032441, 9.894754715216729224 ) ) ;
#48572 = ORIENTED_EDGE ( 'NONE', *, *, #21247, .F. ) ;
#48573 = VERTEX_POINT ( 'NONE', #24130 ) ;
#48574 = DIRECTION ( 'NONE',  ( 0.000000000000000000, 0.000000000000000000, 1.000000000000000000 ) ) ;
#48575 = DIRECTION ( 'NONE',  ( 2.220446049250312588E-16, 0.7071067811865475727, 0.7071067811865474617 ) ) ;
#48576 = ORIENTED_EDGE ( 'NONE', *, *, #48354, .F. ) ;
#48577 = DIRECTION ( 'NONE',  ( 0.000000000000000000, -1.000000000000000000, 2.969158215481698263E-48 ) ) ;
#48578 = CARTESIAN_POINT ( 'NONE',  ( 6.000000000000000888, 7.347880794884120722E-16, 15.00000000000000000 ) ) ;
#48579 = DIRECTION ( 'NONE',  ( 1.000000000000000000, 0.000000000000000000, 0.000000000000000000 ) ) ;
#48580 = DIRECTION ( 'NONE',  ( 1.000000000000000000, 0.000000000000000000, 0.000000000000000000 ) ) ;
#48581 = ORIENTED_EDGE ( 'NONE', *, *, #15235, .T. ) ;
#48582 = DIRECTION ( 'NONE',  ( 0.000000000000000000, 0.000000000000000000, 1.000000000000000000 ) ) ;
#48583 = DIRECTION ( 'NONE',  ( -1.000000000000000000, -0.000000000000000000, -0.000000000000000000 ) ) ;
#48584 = CARTESIAN_POINT ( 'NONE',  ( 115.0540265531850395, 2.143131898507847836E-16, 165.0000000000000000 ) ) ;
#48585 = CARTESIAN_POINT ( 'NONE',  ( 26.64049824243135234, -26.44234984024210178, 4.835783797351800750 ) ) ;
#48586 = EDGE_CURVE ( 'NONE', #44363, #4914, #39775, .T. ) ;
#48587 = CARTESIAN_POINT ( 'NONE',  ( -6.695973446814940111, 0.000000000000000000, 165.0000000000000000 ) ) ;
#48588 = VECTOR ( 'NONE', #4108, 1000.000000000000000 ) ;
#48589 = DIRECTION ( 'NONE',  ( -1.000000000000000000, 0.000000000000000000, 0.000000000000000000 ) ) ;
#48590 = VECTOR ( 'NONE', #13947, 1000.000000000000000 ) ;
#48591 = DIRECTION ( 'NONE',  ( 0.000000000000000000, 0.000000000000000000, -1.000000000000000000 ) ) ;
#48592 = CARTESIAN_POINT ( 'NONE',  ( 0.7547693905852842500, 1.149888081716854638, 9.972175347158394487 ) ) ;
#48593 = CIRCLE ( 'NONE', #1948, 1.750000000000008438 ) ;
#48594 = AXIS2_PLACEMENT_3D ( 'NONE', #9184, #20735, #4819 ) ;
#48595 = ORIENTED_EDGE ( 'NONE', *, *, #37164, .T. ) ;
#48596 = CARTESIAN_POINT ( 'NONE',  ( -84.94597344681494633, 2.143131898507880377E-16, -0.9317124430720247208 ) ) ;
#48597 =( BOUNDED_CURVE ( )  B_SPLINE_CURVE ( 3, ( #17982, #36768, #33656, #45414 ),
 .UNSPECIFIED., .F., .F. ) 
 B_SPLINE_CURVE_WITH_KNOTS ( ( 4, 4 ),
 ( 3.169317492284578310E-16, 1.570796326794938302 ),
 .UNSPECIFIED. ) 
 CURVE ( )  GEOMETRIC_REPRESENTATION_ITEM ( )  RATIONAL_B_SPLINE_CURVE ( ( 1.000000000000000000, 0.8047378541243551675, 0.8047378541243551675, 1.000000000000000000 ) ) 
 REPRESENTATION_ITEM ( '' )  );
#48598 = CARTESIAN_POINT ( 'NONE',  ( 167.5000000000000000, -102.5000000000000142, -10.00000000000000000 ) ) ;
#48599 = CARTESIAN_POINT ( 'NONE',  ( 9.999999999999998224, 8.486842105263161073, 18.34680996553531784 ) ) ;
#48600 = CARTESIAN_POINT ( 'NONE',  ( -0.3370904143228927730, -0.2449105217885335917, 10.00000000000000000 ) ) ;
#48601 = CARTESIAN_POINT ( 'NONE',  ( 31.55402655318503236, 0.000000000000000000, 39.06828755692798438 ) ) ;
#48602 =( BOUNDED_CURVE ( )  B_SPLINE_CURVE ( 3, ( #31286, #12030, #3295, #35397 ),
 .UNSPECIFIED., .F., .F. ) 
 B_SPLINE_CURVE_WITH_KNOTS ( ( 4, 4 ),
 ( 0.000000000000000000, 1.570796326794896558 ),
 .UNSPECIFIED. ) 
 CURVE ( )  GEOMETRIC_REPRESENTATION_ITEM ( )  RATIONAL_B_SPLINE_CURVE ( ( 1.000000000000000000, 0.8047378541243649375, 0.8047378541243649375, 1.000000000000000000 ) ) 
 REPRESENTATION_ITEM ( '' )  );
#48603 = ORIENTED_EDGE ( 'NONE', *, *, #27453, .T. ) ;
#48604 = LINE ( 'NONE', #9402, #44577 ) ;
#48605 = B_SPLINE_SURFACE_WITH_KNOTS ( 'NONE', 3, 3, ( 
 ( #23310, #16375, #490, #43311 ),
 ( #47377, #25273, #4582, #21167 ),
 ( #44992, #12032, #4330, #9370 ),
 ( #15876, #47129, #8437, #23832 ) ),
 .UNSPECIFIED., .F., .F., .F.,
 ( 4, 4 ),
 ( 4, 4 ),
 ( 0.000000000000000000, 1.000000000000000000 ),
 ( 0.000000000000000000, 1.000000000000000000 ),
 .UNSPECIFIED. ) ;
#48606 = ORIENTED_EDGE ( 'NONE', *, *, #5477, .F. ) ;
#48607 = LINE ( 'NONE', #29403, #14434 ) ;
#48608 = CARTESIAN_POINT ( 'NONE',  ( -64.99999999999909051, 17.00000000000000000, 0.000000000000000000 ) ) ;
#48609 = ORIENTED_EDGE ( 'NONE', *, *, #11626, .T. ) ;
#48610 = CARTESIAN_POINT ( 'NONE',  ( 135.0000000000019043, 17.00000000000000000, 65.00000000000000000 ) ) ;
#48611 = FACE_OUTER_BOUND ( 'NONE', #4688, .T. ) ;
#48612 = VERTEX_POINT ( 'NONE', #40028 ) ;
#48613 = EDGE_LOOP ( 'NONE', ( #40895, #27061, #39149, #14436 ) ) ;
#48614 = EDGE_CURVE ( 'NONE', #28535, #27142, #15859, .T. ) ;
#48615 = DIRECTION ( 'NONE',  ( -1.000000000000000000, -0.000000000000000000, -0.000000000000000000 ) ) ;
#48616 = CARTESIAN_POINT ( 'NONE',  ( -0.3862712429686729343, -1.188820645368946050, 10.00000000000000000 ) ) ;
#48617 = DIRECTION ( 'NONE',  ( -1.000000000000000000, -0.000000000000000000, -0.000000000000000000 ) ) ;
#48618 = EDGE_LOOP ( 'NONE', ( #658, #14844, #20451, #36427, #42222, #31103 ) ) ;
#48619 = CARTESIAN_POINT ( 'NONE',  ( 113.3040265531850537, 0.000000000000000000, -165.0000000000000000 ) ) ;
#48620 = AXIS2_PLACEMENT_3D ( 'NONE', #42584, #14640, #26704 ) ;
#48621 = CARTESIAN_POINT ( 'NONE',  ( 75.05402655318509630, -1.025126265847089435, 82.56828755692798438 ) ) ;
#48622 = SURFACE_STYLE_FILL_AREA ( #41218 ) ;
#48623 = VECTOR ( 'NONE', #34534, 1000.000000000000000 ) ;
#48624 = VERTEX_POINT ( 'NONE', #27207 ) ;
#48625 = EDGE_LOOP ( 'NONE', ( #21808, #37274, #31403 ) ) ;
#48626 = EDGE_LOOP ( 'NONE', ( #21348, #44794, #7135, #40266 ) ) ;
#48627 = CARTESIAN_POINT ( 'NONE',  ( 155.0540265531850537, 2.143131898507880377E-16, 159.0682875569279702 ) ) ;
#48628 = CARTESIAN_POINT ( 'NONE',  ( 341.9999999999999432, -181.0000000000001705, -356.0000000000003411 ) ) ;
#48629 = ORIENTED_EDGE ( 'NONE', *, *, #12687, .T. ) ;
#48630 = EDGE_CURVE ( 'NONE', #29600, #20835, #32835, .T. ) ;
#48631 = CARTESIAN_POINT ( 'NONE',  ( -1.011271242968683426, -0.7347315653655928092, -10.00000000000000000 ) ) ;
#48632 = CARTESIAN_POINT ( 'NONE',  ( -86.69597344681494633, -1.750000000000009992, 160.8182875569279702 ) ) ;
#48633 = LINE ( 'NONE', #33306, #7196 ) ;
#48634 = DIRECTION ( 'NONE',  ( -1.000000000000000000, 0.000000000000000000, 0.000000000000000000 ) ) ;
#48635 = CARTESIAN_POINT ( 'NONE',  ( 14.49999999999999822, 12.98684210526315930, -19.37312575500900280 ) ) ;
#48636 = PLANE ( 'NONE',  #46369 ) ;
#48637 = DIRECTION ( 'NONE',  ( -1.000000000000000000, 0.000000000000000000, 0.000000000000000000 ) ) ;
#48638 = FACE_OUTER_BOUND ( 'NONE', #39873, .T. ) ;
#48639 = ADVANCED_FACE ( 'NONE', ( #21772 ), #48419, .T. ) ;
#48640 = CARTESIAN_POINT ( 'NONE',  ( 0.3862712429686978033, -1.188820645368937834, 3.333333333333333481 ) ) ;
#48641 = CARTESIAN_POINT ( 'NONE',  ( -26.18032376592659105, 21.95228666728381128, 7.455576670931136185 ) ) ;
#48642 = AXIS2_PLACEMENT_3D ( 'NONE', #41110, #21606, #38486 ) ;
#48643 = CARTESIAN_POINT ( 'NONE',  ( -20.00000000000003197, 17.00000000000000000, -114.9999999999999858 ) ) ;
#48644 = ORIENTED_EDGE ( 'NONE', *, *, #15287, .F. ) ;
#48645 = LINE ( 'NONE', #41750, #1602 ) ;
#48646 = CARTESIAN_POINT ( 'NONE',  ( 115.0540265531850395, 2.143131898507847836E-16, -0.9317124430719969652 ) ) ;
#48647 = CARTESIAN_POINT ( 'NONE',  ( -166.6959734468149463, -1.750000000000009992, 0.8182875569279768335 ) ) ;
#48648 = CARTESIAN_POINT ( 'NONE',  ( 195.0540265531851105, 2.143131898507880377E-16, -0.9317124430720247208 ) ) ;
#48649 = ORIENTED_EDGE ( 'NONE', *, *, #42744, .T. ) ;
#48650 = CARTESIAN_POINT ( 'NONE',  ( 73.30402655318508209, 0.000000000000000000, 165.0000000000000000 ) ) ;
#48651 = CARTESIAN_POINT ( 'NONE',  ( -2.920962725444330221, -37.39284056564468983, -9.011255500499645521 ) ) ;
#48652 = CIRCLE ( 'NONE', #34816, 4.000000000000003553 ) ;
#48653 = ORIENTED_EDGE ( 'NONE', *, *, #1354, .T. ) ;
#48654 = CARTESIAN_POINT ( 'NONE',  ( 17.23491422248386584, -0.5912720620000816441, 8.727788335465566760 ) ) ;
#48655 = AXIS2_PLACEMENT_3D ( 'NONE', #10111, #28860, #25769 ) ;
#48656 = DIRECTION ( 'NONE',  ( 0.000000000000000000, -4.687818848539279227E-49, 1.000000000000000000 ) ) ;
#48657 = CARTESIAN_POINT ( 'NONE',  ( 35.00000000000216716, 17.00000000000000000, 115.0000000000000142 ) ) ;
#48658 = ORIENTED_EDGE ( 'NONE', *, *, #23710, .F. ) ;
#48659 = CARTESIAN_POINT ( 'NONE',  ( -0.4400426740873942810, 2.015233077865125733, 9.886433018048068178 ) ) ;
#48660 = VERTEX_POINT ( 'NONE', #13803 ) ;
#48661 = ORIENTED_EDGE ( 'NONE', *, *, #18608, .F. ) ;
#48662 = VECTOR ( 'NONE', #30830, 1000.000000000000000 ) ;
#48663 = LINE ( 'NONE', #43167, #23825 ) ;
#48664 = EDGE_CURVE ( 'NONE', #7126, #42669, #24868, .T. ) ;
#48665 = EDGE_CURVE ( 'NONE', #39055, #19705, #33912, .T. ) ;
#48666 = ORIENTED_EDGE ( 'NONE', *, *, #8874, .T. ) ;
#48667 = CYLINDRICAL_SURFACE ( 'NONE', #8987, 4.000000000000003553 ) ;
#48668 = LINE ( 'NONE', #42026, #29005 ) ;
#48669 = ORIENTED_EDGE ( 'NONE', *, *, #43149, .F. ) ;
#48670 = DIRECTION ( 'NONE',  ( 0.8962124318248270161, -0.000000000000000000, 0.4436251537532894806 ) ) ;
#48671 = LINE ( 'NONE', #24872, #32447 ) ;
#48672 = EDGE_CURVE ( 'NONE', #387, #11195, #12614, .T. ) ;
#48673 = CARTESIAN_POINT ( 'NONE',  ( 340.0000000000000568, 165.0000000000000000, 355.9999999999997726 ) ) ;
#48674 = ORIENTED_EDGE ( 'NONE', *, *, #10325, .T. ) ;
#48675 = EDGE_CURVE ( 'NONE', #22379, #1434, #30309, .T. ) ;
#48676 = FACE_OUTER_BOUND ( 'NONE', #38163, .T. ) ;
#48677 = EDGE_CURVE ( 'NONE', #29337, #44889, #19810, .T. ) ;
#48678 = AXIS2_PLACEMENT_3D ( 'NONE', #10631, #41682, #33749 ) ;
#48679 = ORIENTED_EDGE ( 'NONE', *, *, #11217, .T. ) ;
#48680 = CARTESIAN_POINT ( 'NONE',  ( -6.695973446814940111, -1.750000000000023315, 0.8182875569279768335 ) ) ;
#48681 = DIRECTION ( 'NONE',  ( 0.000000000000000000, 1.000000000000000000, 0.000000000000000000 ) ) ;
#48682 = ORIENTED_EDGE ( 'NONE', *, *, #18472, .T. ) ;
#48683 = AXIS2_PLACEMENT_3D ( 'NONE', #26238, #2616, #42376 ) ;
#48684 = EDGE_LOOP ( 'NONE', ( #48330, #2335, #11960, #49982 ) ) ;
#48685 = ORIENTED_EDGE ( 'NONE', *, *, #32396, .T. ) ;
#48686 = DIRECTION ( 'NONE',  ( 1.000000000000000000, 0.000000000000000000, 0.000000000000000000 ) ) ;
#48687 = DIRECTION ( 'NONE',  ( -1.000000000000000000, -0.000000000000000000, -0.000000000000000000 ) ) ;
#48688 = ORIENTED_EDGE ( 'NONE', *, *, #4044, .F. ) ;
#48689 = CARTESIAN_POINT ( 'NONE',  ( 0.6679403265625496466, -1.504705676290996941, 9.936700280135882579 ) ) ;
#48690 = DIRECTION ( 'NONE',  ( 0.000000000000000000, 0.000000000000000000, -1.000000000000000000 ) ) ;
#48691 = CARTESIAN_POINT ( 'NONE',  ( -0.4183366619398694031, 10.00548002840395867, 6.429680520823656487 ) ) ;
#48692 = EDGE_LOOP ( 'NONE', ( #2662, #41545, #47323, #49847 ) ) ;
#48693 = VECTOR ( 'NONE', #30170, 1000.000000000000000 ) ;
#48694 = PLANE ( 'NONE',  #35499 ) ;
#48695 = CARTESIAN_POINT ( 'NONE',  ( 48.33712804702525290, 13.03701565032775456, -9.367992836599951190 ) ) ;
#48696 = FACE_OUTER_BOUND ( 'NONE', #50394, .T. ) ;
#48697 = ADVANCED_FACE ( 'NONE', ( #40272 ), #48918, .F. ) ;
#48698 = ADVANCED_FACE ( 'NONE', ( #5101 ), #2267, .T. ) ;
#48699 = VECTOR ( 'NONE', #4069, 1000.000000000000000 ) ;
#48700 = VERTEX_POINT ( 'NONE', #17905 ) ;
#48701 = ITEM_DEFINED_TRANSFORMATION ( 'NONE', 'NONE', #15200,  #45486 ) ;
#48702 = CARTESIAN_POINT ( 'NONE',  ( -14.49999999999999822, 12.98684210526315930, 20.00000000000000000 ) ) ;
#48703 = EDGE_CURVE ( 'NONE', #39370, #15868, #25628, .T. ) ;
#48704 = ADVANCED_FACE ( 'NONE', ( #28965 ), #12983, .T. ) ;
#48705 = CARTESIAN_POINT ( 'NONE',  ( 0.4402948852767718524, -2.015117899693914527, 9.894754715216725671 ) ) ;
#48706 = CARTESIAN_POINT ( 'NONE',  ( -46.11867747200562917, 19.86470446310265103, -8.016098858316199838 ) ) ;
#48707 = ORIENTED_EDGE ( 'NONE', *, *, #24245, .F. ) ;
#48708 = EDGE_CURVE ( 'NONE', #41095, #10553, #48668, .T. ) ;
#48709 = FACE_OUTER_BOUND ( 'NONE', #4356, .T. ) ;
#48710 = FACE_OUTER_BOUND ( 'NONE', #7325, .T. ) ;
#48711 = EDGE_CURVE ( 'NONE', #2212, #39326, #38453, .T. ) ;
#48712 = DIRECTION ( 'NONE',  ( -1.000000000000000000, -0.000000000000000000, -0.000000000000000000 ) ) ;
#48713 = FACE_OUTER_BOUND ( 'NONE', #22948, .T. ) ;
#48714 = DIRECTION ( 'NONE',  ( -1.000000000000000000, -0.000000000000000000, -0.000000000000000000 ) ) ;
#48715 = ORIENTED_EDGE ( 'NONE', *, *, #10479, .F. ) ;
#48716 = VECTOR ( 'NONE', #29463, 1000.000000000000000 ) ;
#48717 = CARTESIAN_POINT ( 'NONE',  ( -25.79500241909648395, 7.611558401714507482, 230.0000000000000000 ) ) ;
#48718 = VERTEX_POINT ( 'NONE', #34098 ) ;
#48719 = FACE_OUTER_BOUND ( 'NONE', #37084, .T. ) ;
#48720 = VECTOR ( 'NONE', #46397, 1000.000000000000000 ) ;
#48721 = ORIENTED_EDGE ( 'NONE', *, *, #49536, .F. ) ;
#48722 = CARTESIAN_POINT ( 'NONE',  ( -225.0000000000000568, 164.9999999999999716, 500.0000000000000000 ) ) ;
#48723 = DIRECTION ( 'NONE',  ( 1.000000000000000000, 0.000000000000000000, 0.000000000000000000 ) ) ;
#48724 = CARTESIAN_POINT ( 'NONE',  ( -166.6959734468149463, -1.750000000000009992, 160.8182875569279702 ) ) ;
#48725 = ADVANCED_FACE ( 'NONE', ( #49175 ), #49430, .T. ) ;
#48726 = ORIENTED_EDGE ( 'NONE', *, *, #2352, .F. ) ;
#48727 = AXIS2_PLACEMENT_3D ( 'NONE', #41118, #21882, #2609 ) ;
#48728 = ADVANCED_FACE ( 'NONE', ( #14827 ), #30482, .T. ) ;
#48729 = CARTESIAN_POINT ( 'NONE',  ( 35.05402655318504657, -1.025126265847089435, 39.06828755692797728 ) ) ;
#48730 = ADVANCED_FACE ( 'NONE', ( #14318 ), #23026, .F. ) ;
#48731 = ORIENTED_EDGE ( 'NONE', *, *, #8476, .F. ) ;
#48732 = DIRECTION ( 'NONE',  ( 1.000000000000000000, 0.000000000000000000, -1.860490536778032451E-50 ) ) ;
#48733 = VECTOR ( 'NONE', #48577, 1000.000000000000000 ) ;
#48734 = CARTESIAN_POINT ( 'NONE',  ( 340.0000000000000568, 169.0000000000000284, 343.9999999999998295 ) ) ;
#48735 = VECTOR ( 'NONE', #17923, 1000.000000000000000 ) ;
#48736 = CARTESIAN_POINT ( 'NONE',  ( 0.3370904143228947158, 0.2449105217885311492, 10.00000000000000000 ) ) ;
#48737 = DIRECTION ( 'NONE',  ( 0.000000000000000000, 0.000000000000000000, 1.000000000000000000 ) ) ;
#48738 = CARTESIAN_POINT ( 'NONE',  ( -9.174209336589896679, -3.979181203266159095, 9.646707543097347681 ) ) ;
#48739 = ORIENTED_EDGE ( 'NONE', *, *, #10848, .T. ) ;
#48740 = PRODUCT_DEFINITION_FORMATION_WITH_SPECIFIED_SOURCE ( 'ANY', '', #43383, .NOT_KNOWN. ) ;
#48741 = VERTEX_POINT ( 'NONE', #11248 ) ;
#48742 = FACE_OUTER_BOUND ( 'NONE', #16514, .T. ) ;
#48743 = AXIS2_PLACEMENT_3D ( 'NONE', #26534, #46495, #46247 ) ;
#48744 =( BOUNDED_CURVE ( )  B_SPLINE_CURVE ( 3, ( #18970, #34648, #15131, #19478 ),
 .UNSPECIFIED., .F., .F. ) 
 B_SPLINE_CURVE_WITH_KNOTS ( ( 4, 4 ),
 ( 4.712388980384689674, 6.283185307179586232 ),
 .UNSPECIFIED. ) 
 CURVE ( )  GEOMETRIC_REPRESENTATION_ITEM ( )  RATIONAL_B_SPLINE_CURVE ( ( 1.000000000000000000, 0.8047378541243649375, 0.8047378541243649375, 1.000000000000000000 ) ) 
 REPRESENTATION_ITEM ( '' )  );
#48745 = ORIENTED_EDGE ( 'NONE', *, *, #20548, .F. ) ;
#48746 = CARTESIAN_POINT ( 'NONE',  ( -25.40454589245989325, -27.58367357691681931, -8.192531242611266862 ) ) ;
#48747 = ORIENTED_EDGE ( 'NONE', *, *, #34837, .T. ) ;
#48748 = CARTESIAN_POINT ( 'NONE',  ( -22.69295089195507131, -45.31600496604688999, 7.455576670931136185 ) ) ;
#48749 = ADVANCED_FACE ( 'NONE', ( #45338 ), #22525, .T. ) ;
#48750 =( BOUNDED_CURVE ( )  B_SPLINE_CURVE ( 3, ( #8010, #23646, #7752, #3371 ),
 .UNSPECIFIED., .F., .F. ) 
 B_SPLINE_CURVE_WITH_KNOTS ( ( 4, 4 ),
 ( 3.141592653589793116, 4.712388980384689674 ),
 .UNSPECIFIED. ) 
 CURVE ( )  GEOMETRIC_REPRESENTATION_ITEM ( )  RATIONAL_B_SPLINE_CURVE ( ( 1.000000000000000000, 0.8047378541243649375, 0.8047378541243649375, 1.000000000000000000 ) ) 
 REPRESENTATION_ITEM ( '' )  );
#48751 = CARTESIAN_POINT ( 'NONE',  ( 340.0000000000000568, 169.0000000000000000, 343.9999999999998295 ) ) ;
#48752 = ORIENTED_EDGE ( 'NONE', *, *, #47001, .T. ) ;
#48753 = CARTESIAN_POINT ( 'NONE',  ( -4.945973446814903696, 2.143131898507912917E-16, -160.9317124430720582 ) ) ;
#48754 = FACE_OUTER_BOUND ( 'NONE', #37733, .T. ) ;
#48755 = DIRECTION ( 'NONE',  ( 1.000000000000000000, 0.000000000000000000, 0.000000000000000000 ) ) ;
#48756 = CARTESIAN_POINT ( 'NONE',  ( 1.578643388466006714, -1.550786058692517511, 9.881002359080275355 ) ) ;
#48757 = ORIENTED_EDGE ( 'NONE', *, *, #5194, .T. ) ;
#48758 = ORIENTED_EDGE ( 'NONE', *, *, #13944, .F. ) ;
#48759 = ADVANCED_FACE ( 'NONE', ( #2523 ), #7399, .T. ) ;
#48760 = CARTESIAN_POINT ( 'NONE',  ( 33.30402655318503946, 0.000000000000000000, 165.0000000000000000 ) ) ;
#48761 = VECTOR ( 'NONE', #21156, 1000.000000000000000 ) ;
#48762 = CARTESIAN_POINT ( 'NONE',  ( 0.3965308786431460675, 0.1288406926356965576, 9.992737339167973687 ) ) ;
#48763 = CARTESIAN_POINT ( 'NONE',  ( -0.3862712429686729343, -1.188820645368946050, 3.333333333333333481 ) ) ;
#48764 = CARTESIAN_POINT ( 'NONE',  ( -164.9999999999981526, 17.00000000000000000, 65.00000000000000000 ) ) ;
#48765 = VECTOR ( 'NONE', #48946, 1000.000000000000000 ) ;
#48766 =( BOUNDED_CURVE ( )  B_SPLINE_CURVE ( 3, ( #39133, #47018, #8078, #19354 ),
 .UNSPECIFIED., .F., .F. ) 
 B_SPLINE_CURVE_WITH_KNOTS ( ( 4, 4 ),
 ( 3.141592653589793116, 4.712388980384689674 ),
 .UNSPECIFIED. ) 
 CURVE ( )  GEOMETRIC_REPRESENTATION_ITEM ( )  RATIONAL_B_SPLINE_CURVE ( ( 1.000000000000000000, 0.8047378541243649375, 0.8047378541243649375, 1.000000000000000000 ) ) 
 REPRESENTATION_ITEM ( '' )  );
#48767 = CARTESIAN_POINT ( 'NONE',  ( -1.249999999999999778, 0.000000000000000000, -10.00000000000000000 ) ) ;
#48768 = EDGE_LOOP ( 'NONE', ( #31211, #31165, #35955, #19116, #50263, #18718 ) ) ;
#48769 = LINE ( 'NONE', #10328, #2099 ) ;
#48770 = VERTEX_POINT ( 'NONE', #42521 ) ;
#48771 = CARTESIAN_POINT ( 'NONE',  ( -31.71344115042995426, 23.18201308416445272, -1.383675951444951480 ) ) ;
#48772 = LINE ( 'NONE', #26226, #1565 ) ;
#48773 = CIRCLE ( 'NONE', #46326, 1.750000000000008438 ) ;
#48774 = FACE_OUTER_BOUND ( 'NONE', #19640, .T. ) ;
#48775 = CARTESIAN_POINT ( 'NONE',  ( -114.9999999999981526, 17.00000000000000000, 90.00000000000000000 ) ) ;
#48776 = ADVANCED_FACE ( 'NONE', ( #41525 ), #45774, .T. ) ;
#48777 = EDGE_CURVE ( 'NONE', #48433, #22911, #18149, .T. ) ;
#48778 = CARTESIAN_POINT ( 'NONE',  ( 195.9526953830863079, 159.2880105690400399, 23.74256005001722158 ) ) ;
#48779 = CARTESIAN_POINT ( 'NONE',  ( -168.4459734468149463, 0.000000000000000000, 165.0000000000000000 ) ) ;
#48780=STYLED_ITEM('',(#50747),#21477);
#48781 = CARTESIAN_POINT ( 'NONE',  ( 35.05402655318504657, 2.143131898507880377E-16, 79.06828755692797017 ) ) ;
#48782 = ORIENTED_EDGE ( 'NONE', *, *, #29922, .F. ) ;
#48783 = CARTESIAN_POINT ( 'NONE',  ( -8.445973446814964092, -1.025126265847097207, 39.06828755692796307 ) ) ;
#48784 = ADVANCED_FACE ( 'NONE', ( #14572 ), #26885, .F. ) ;
#48785 = DIRECTION ( 'NONE',  ( 0.000000000000000000, 1.000000000000000000, 0.000000000000000000 ) ) ;
#48786 = LINE ( 'NONE', #37312, #25890 ) ;
#48787 = VECTOR ( 'NONE', #7362, 1000.000000000000000 ) ;
#48788 = ADVANCED_FACE ( 'NONE', ( #3518 ), #30227, .T. ) ;
#48789 = EDGE_CURVE ( 'NONE', #21707, #218, #701, .T. ) ;
#48790 = ORIENTED_EDGE ( 'NONE', *, *, #49385, .T. ) ;
#48791 = CYLINDRICAL_SURFACE ( 'NONE', #30269, 4.000000000000003553 ) ;
#48792 = ORIENTED_EDGE ( 'NONE', *, *, #32682, .T. ) ;
#48793 = LINE ( 'NONE', #32953, #19641 ) ;
#48794 = PLANE ( 'NONE',  #2052 ) ;
#48795 = EDGE_CURVE ( 'NONE', #21143, #13147, #46597, .T. ) ;
#48796 = CARTESIAN_POINT ( 'NONE',  ( 185.0000000000000000, -164.9999999999999432, 343.9999999999998863 ) ) ;
#48797 = VECTOR ( 'NONE', #5871, 1000.000000000000000 ) ;
#48798 = DIRECTION ( 'NONE',  ( -0.000000000000000000, -1.000000000000000000, -0.000000000000000000 ) ) ;
#48799 = LINE ( 'NONE', #49038, #45899 ) ;
#48800 = VECTOR ( 'NONE', #6584, 1000.000000000000000 ) ;
#48801 = PLANE ( 'NONE',  #45042 ) ;
#48802 = CARTESIAN_POINT ( 'NONE',  ( 18.38319608353691947, -32.68498281710168385, -8.192531242611265085 ) ) ;
#48803 = ORIENTED_EDGE ( 'NONE', *, *, #23078, .F. ) ;
#48804 = ORIENTED_EDGE ( 'NONE', *, *, #46939, .T. ) ;
#48805 = CARTESIAN_POINT ( 'NONE',  ( -3.940019464150765760, -33.28272320232423453, -8.466730184410787174 ) ) ;
#48806 = CARTESIAN_POINT ( 'NONE',  ( 0.000000000000000000, 50.00000000000000000, 900.0000000000000000 ) ) ;
#48807 = VERTEX_POINT ( 'NONE', #43288 ) ;
#48808 = ORIENTED_EDGE ( 'NONE', *, *, #18331, .F. ) ;
#48809 = LINE ( 'NONE', #10101, #32997 ) ;
#48810 = DIRECTION ( 'NONE',  ( -1.000000000000000000, -0.000000000000000000, -0.000000000000000000 ) ) ;
#48811 = ORIENTED_EDGE ( 'NONE', *, *, #31504, .F. ) ;
#48812 = ORIENTED_EDGE ( 'NONE', *, *, #39367, .F. ) ;
#48813 = EDGE_CURVE ( 'NONE', #34969, #11740, #30611, .T. ) ;
#48814 = VECTOR ( 'NONE', #18728, 1000.000000000000000 ) ;
#48815 = CARTESIAN_POINT ( 'NONE',  ( 15.00000000000000000, -3.557843729863133575, 15.59977635401528673 ) ) ;
#48816 = CARTESIAN_POINT ( 'NONE',  ( 0.7831114743371334619, 7.934214588790045042, -2.805373121306242723E-15 ) ) ;
#48817 = VERTEX_POINT ( 'NONE', #12004 ) ;
#48818 = VERTEX_POINT ( 'NONE', #4789 ) ;
#48819 = FACE_OUTER_BOUND ( 'NONE', #50602, .T. ) ;
#48820 = CARTESIAN_POINT ( 'NONE',  ( -15.00099850811941948, -7.462898891544107016, 9.403735324607438884 ) ) ;
#48821 = VERTEX_POINT ( 'NONE', #12246 ) ;
#48822 = ORIENTED_EDGE ( 'NONE', *, *, #38720, .F. ) ;
#48823 = DIRECTION ( 'NONE',  ( 1.000000000000000000, 0.000000000000000000, 0.000000000000000000 ) ) ;
#48824 = CARTESIAN_POINT ( 'NONE',  ( 339.9999999999998863, -181.0000000000001421, -349.9999999999998863 ) ) ;
#48825 = ORIENTED_EDGE ( 'NONE', *, *, #37313, .T. ) ;
#48826 = LINE ( 'NONE', #21670, #14386 ) ;
#48827 = DIRECTION ( 'NONE',  ( 1.000000000000000000, 0.000000000000000000, 0.000000000000000000 ) ) ;
#48828 = CARTESIAN_POINT ( 'NONE',  ( 113.3040265531850537, -1.749999999999997335, -79.18171244307201562 ) ) ;
#48829 = CARTESIAN_POINT ( 'NONE',  ( -114.9999999999994031, 17.00000000000000000, -54.99999999999999289 ) ) ;
#48830 = EDGE_CURVE ( 'NONE', #34173, #20578, #4047, .T. ) ;
#48831 = ADVANCED_FACE ( 'NONE', ( #42771 ), #35623, .T. ) ;
#48832 = VECTOR ( 'NONE', #8041, 1000.000000000000000 ) ;
#48833 = CARTESIAN_POINT ( 'NONE',  ( 153.2026953830863647, -66.40178110878292728, -93.79675437945473959 ) ) ;
#48834 = VECTOR ( 'NONE', #27101, 1000.000000000000000 ) ;
#48835 = ORIENTED_EDGE ( 'NONE', *, *, #26843, .F. ) ;
#48836 = CARTESIAN_POINT ( 'NONE',  ( -44.25629667545849344, 43.33333333333339255, 790.0000000000000000 ) ) ;
#48837 = CARTESIAN_POINT ( 'NONE',  ( 0.3862712429686727678, 1.188820645368945605, -10.00000000000000000 ) ) ;
#48838 = EDGE_CURVE ( 'NONE', #7277, #40406, #37521, .T. ) ;
#48839 = CARTESIAN_POINT ( 'NONE',  ( -7.241383964640739634, -3.469446951953614189E-15, 5.000000000000000000 ) ) ;
#48840 = CARTESIAN_POINT ( 'NONE',  ( 183.0000000000000000, -180.9999999999999716, -350.0000000000001705 ) ) ;
#48841 = EDGE_CURVE ( 'NONE', #49685, #47734, #462, .T. ) ;
#48842 = EDGE_CURVE ( 'NONE', #18457, #32184, #16103, .T. ) ;
#48843 = CYLINDRICAL_SURFACE ( 'NONE', #10112, 1.750000000000008438 ) ;
#48844 = CARTESIAN_POINT ( 'NONE',  ( 151.5540265531850537, 0.000000000000000000, -0.9317124430720247208 ) ) ;
#48845 = EDGE_CURVE ( 'NONE', #24077, #8523, #37667, .T. ) ;
#48846 = PLANE ( 'NONE',  #27822 ) ;
#48847 = CARTESIAN_POINT ( 'NONE',  ( -10.00000000000000000, 0.000000000000000000, 10.00000000000000000 ) ) ;
#48848 = FACE_BOUND ( 'NONE', #12064, .T. ) ;
#48849 = AXIS2_PLACEMENT_3D ( 'NONE', #21025, #20270, #5616 ) ;
#48850 = ORIENTED_EDGE ( 'NONE', *, *, #22162, .T. ) ;
#48851 = CARTESIAN_POINT ( 'NONE',  ( -47.72109971266203132, 1.750000000000009548, 121.8434138227750623 ) ) ;
#48852 = DIRECTION ( 'NONE',  ( -0.000000000000000000, -0.000000000000000000, -1.000000000000000000 ) ) ;
#48853 = DIRECTION ( 'NONE',  ( -0.000000000000000000, -0.000000000000000000, -1.000000000000000000 ) ) ;
#48854 = CARTESIAN_POINT ( 'NONE',  ( 36.08557433729230723, -35.58569447144768105, 7.455576670931136185 ) ) ;
#48855 = DIRECTION ( 'NONE',  ( -1.586032880504786307E-16, 1.654361225106055350E-24, -1.000000000000000000 ) ) ;
#48856 = ORIENTED_EDGE ( 'NONE', *, *, #19907, .T. ) ;
#48857 = CARTESIAN_POINT ( 'NONE',  ( -208.4459734468148611, -1.025126265847089435, 2.568287556927986159 ) ) ;
#48858 = EDGE_LOOP ( 'NONE', ( #35380, #21021, #43390, #8746 ) ) ;
#48859 = CARTESIAN_POINT ( 'NONE',  ( 355.9999999999999432, -183.0000000000001421, -358.0000000000003411 ) ) ;
#48860 = CARTESIAN_POINT ( 'NONE',  ( -48.44597344681492501, 2.143131898507880377E-16, -160.9317124430720298 ) ) ;
#48861 = AXIS2_PLACEMENT_3D ( 'NONE', #33854, #22536, #18928 ) ;
#48862 = ORIENTED_EDGE ( 'NONE', *, *, #18598, .T. ) ;
#48863 = CYLINDRICAL_SURFACE ( 'NONE', #8224, 1.749999999999987566 ) ;
#48864 = DIRECTION ( 'NONE',  ( 0.000000000000000000, 1.000000000000000000, -0.000000000000000000 ) ) ;
#48865 = VERTEX_POINT ( 'NONE', #43541 ) ;
#48866 = ORIENTED_EDGE ( 'NONE', *, *, #49404, .F. ) ;
#48867 = EDGE_CURVE ( 'NONE', #23523, #20193, #11748, .T. ) ;
#48868 = EDGE_CURVE ( 'NONE', #11426, #48770, #25751, .T. ) ;
#48869 = DIRECTION ( 'NONE',  ( -0.000000000000000000, -0.000000000000000000, -1.000000000000000000 ) ) ;
#48870 = CARTESIAN_POINT ( 'NONE',  ( 359.9999999999999432, -180.9999999999999716, 355.9999999999998295 ) ) ;
#48871 = FACE_OUTER_BOUND ( 'NONE', #25024, .T. ) ;
#48872 = ORIENTED_EDGE ( 'NONE', *, *, #24859, .F. ) ;
#48873 = CARTESIAN_POINT ( 'NONE',  ( 37.90972275097263378, -14.83505920947803780, 901.8832493327278144 ) ) ;
#48874 = DIRECTION ( 'NONE',  ( -1.000000000000000000, 0.000000000000000000, -7.793956916774525800E-48 ) ) ;
#48875 = CYLINDRICAL_SURFACE ( 'NONE', #32732, 1.750000000000015543 ) ;
#48876 = ORIENTED_EDGE ( 'NONE', *, *, #735, .F. ) ;
#48877 = VERTEX_POINT ( 'NONE', #23806 ) ;
#48878 = CARTESIAN_POINT ( 'NONE',  ( 154.3291528190321458, -1.750000000000009326, 159.7931612910809065 ) ) ;
#48879 = DIRECTION ( 'NONE',  ( -1.000000000000000000, 0.000000000000000000, 0.000000000000000000 ) ) ;
#48880 = CARTESIAN_POINT ( 'NONE',  ( 357.1715728752538439, -183.0000000000001421, 358.0000000000000568 ) ) ;
#48881 = ORIENTED_EDGE ( 'NONE', *, *, #32894, .F. ) ;
#48882 = CARTESIAN_POINT ( 'NONE',  ( -84.94597344681494633, 2.143131898507880377E-16, 165.0000000000000000 ) ) ;
#48883 = CARTESIAN_POINT ( 'NONE',  ( -206.6959734468149463, -1.750000000000010214, 40.81828755692798438 ) ) ;
#48884 = CARTESIAN_POINT ( 'NONE',  ( -1.320835335343009787, 0.01943189458965158267, 9.943883492372876276 ) ) ;
#48885 = LINE ( 'NONE', #44308, #4231 ) ;
#48886 = LINE ( 'NONE', #24840, #41296 ) ;
#48887 = CARTESIAN_POINT ( 'NONE',  ( -48.44597344681496054, -1.025126265847089213, 162.5682875569279133 ) ) ;
#48888 = CARTESIAN_POINT ( 'NONE',  ( -22.82242230425432439, 2.683863964738837371, 229.0000000000000000 ) ) ;
#48889 = CARTESIAN_POINT ( 'NONE',  ( -208.4459734468149179, 2.143131898507880377E-16, -160.9317124430720298 ) ) ;
#48890 = CARTESIAN_POINT ( 'NONE',  ( -34.30563531518998133, -15.23322832906865543, 6.057468652304066836 ) ) ;
#48891 = CARTESIAN_POINT ( 'NONE',  ( 0.000000000000000000, -250.0000000000000000, 225.0000000000000000 ) ) ;
#48892 =( BOUNDED_CURVE ( )  B_SPLINE_CURVE ( 3, ( #46250, #22429, #49329, #2430 ),
 .UNSPECIFIED., .F., .F. ) 
 B_SPLINE_CURVE_WITH_KNOTS ( ( 4, 4 ),
 ( 0.000000000000000000, 1.570796326794896558 ),
 .UNSPECIFIED. ) 
 CURVE ( )  GEOMETRIC_REPRESENTATION_ITEM ( )  RATIONAL_B_SPLINE_CURVE ( ( 1.000000000000000000, 0.8047378541243649375, 0.8047378541243649375, 1.000000000000000000 ) ) 
 REPRESENTATION_ITEM ( '' )  );
#48893 = AXIS2_PLACEMENT_3D ( 'NONE', #7936, #19719, #988 ) ;
#48894 = CARTESIAN_POINT ( 'NONE',  ( 0.000000000000000000, 169.0000000000000000, 359.9999999999997726 ) ) ;
#48895 = ORIENTED_EDGE ( 'NONE', *, *, #37159, .F. ) ;
#48896 = EDGE_CURVE ( 'NONE', #3284, #37192, #3791, .T. ) ;
#48897 = DIRECTION ( 'NONE',  ( -1.000000000000000000, 0.000000000000000000, -1.612977847700450206E-50 ) ) ;
#48898 =( BOUNDED_CURVE ( )  B_SPLINE_CURVE ( 3, ( #14344, #37976, #10500, #26399 ),
 .UNSPECIFIED., .F., .F. ) 
 B_SPLINE_CURVE_WITH_KNOTS ( ( 4, 4 ),
 ( 0.000000000000000000, 1.570796326794896558 ),
 .UNSPECIFIED. ) 
 CURVE ( )  GEOMETRIC_REPRESENTATION_ITEM ( )  RATIONAL_B_SPLINE_CURVE ( ( 1.000000000000000000, 0.8047378541243649375, 0.8047378541243649375, 1.000000000000000000 ) ) 
 REPRESENTATION_ITEM ( '' )  );
#48899 = CYLINDRICAL_SURFACE ( 'NONE', #14375, 4.000000000000003553 ) ;
#48900 = B_SPLINE_CURVE_WITH_KNOTS ( 'NONE', 3,
 ( #10543, #50251, #30308, #38531 ),
 .UNSPECIFIED., .F., .F.,
 ( 4, 4 ),
 ( 7.818293051731877089E-18, 0.0004072981213141015620 ),
 .UNSPECIFIED. ) ;
#48901 = CARTESIAN_POINT ( 'NONE',  ( 195.0540265531851105, 1.025126265847089213, -0.9317124430720324924 ) ) ;
#48902 = ORIENTED_EDGE ( 'NONE', *, *, #37344, .F. ) ;
#48903 = DIRECTION ( 'NONE',  ( 1.000000000000000000, 1.156482317317870492E-16, -0.000000000000000000 ) ) ;
#48904 = CARTESIAN_POINT ( 'NONE',  ( 135.0000000000012790, 16.00000000000000000, 5.000000000000004441 ) ) ;
#48905 = ORIENTED_EDGE ( 'NONE', *, *, #12633, .F. ) ;
#48906 = CYLINDRICAL_SURFACE ( 'NONE', #13229, 1.750000000000015543 ) ;
#48907 = CARTESIAN_POINT ( 'NONE',  ( -214.9999999999999432, 173.0000000000000000, 252.0000000000000000 ) ) ;
#48908 = CARTESIAN_POINT ( 'NONE',  ( 153.3040265531850537, 1.750000000000010658, -119.1817124430720440 ) ) ;
#48909 = DIRECTION ( 'NONE',  ( -1.000000000000000000, 0.000000000000000000, 0.000000000000000000 ) ) ;
#48910 = ORIENTED_EDGE ( 'NONE', *, *, #9890, .F. ) ;
#48911 = CARTESIAN_POINT ( 'NONE',  ( 72.27890028733797578, -1.750000000000010214, -80.20683870891910772 ) ) ;
#48912 = B_SPLINE_SURFACE_WITH_KNOTS ( 'NONE', 3, 3, ( 
 ( #16842, #48087, #13230, #43775 ),
 ( #8644, #38371, #9891, #21947 ),
 ( #26054, #13737, #29898, #37622 ),
 ( #2935, #33266, #26309, #49352 ) ),
 .UNSPECIFIED., .F., .F., .F.,
 ( 4, 4 ),
 ( 4, 4 ),
 ( 0.000000000000000000, 1.000000000000000000 ),
 ( 0.000000000000000000, 1.000000000000000000 ),
 .UNSPECIFIED. ) ;
#48913 = EDGE_LOOP ( 'NONE', ( #14943, #15743, #9619, #35361, #46649, #1258 ) ) ;
#48914 = VERTEX_POINT ( 'NONE', #35121 ) ;
#48915 = DIRECTION ( 'NONE',  ( 0.000000000000000000, 0.000000000000000000, 1.000000000000000000 ) ) ;
#48916 = ORIENTED_EDGE ( 'NONE', *, *, #2270, .F. ) ;
#48917 = DIRECTION ( 'NONE',  ( 1.000000000000000000, -0.000000000000000000, 0.000000000000000000 ) ) ;
#48918 = PLANE ( 'NONE',  #11797 ) ;
#48919 = ORIENTED_EDGE ( 'NONE', *, *, #31182, .T. ) ;
#48920 = CARTESIAN_POINT ( 'NONE',  ( -165.0000000000000284, 16.00000000000000000, 115.0000000000000142 ) ) ;
#48921 = CYLINDRICAL_SURFACE ( 'NONE', #10980, 4.000000000000003553 ) ;
#48922 = CARTESIAN_POINT ( 'NONE',  ( -165.0000000000000284, 15.00000000000000000, -114.9999999999999858 ) ) ;
#48923 = ORIENTED_EDGE ( 'NONE', *, *, #42554, .F. ) ;
#48925 = ADVANCED_FACE ( 'NONE', ( #39212 ), #15598, .T. ) ;
#48924 = LINE ( 'NONE', #25383, #45248 ) ;
#48926 = DIRECTION ( 'NONE',  ( -1.000000000000000000, 0.000000000000000000, -7.793956916774525800E-48 ) ) ;
#48927 = EDGE_LOOP ( 'NONE', ( #656, #21372, #27840 ) ) ;
#48928 = VECTOR ( 'NONE', #21169, 1000.000000000000000 ) ;
#48929 = FACE_OUTER_BOUND ( 'NONE', #8213, .T. ) ;
#48930 = CARTESIAN_POINT ( 'NONE',  ( 181.0000000000000000, -272.4999999999999432, -341.9999999999999432 ) ) ;
#48931 = ORIENTED_EDGE ( 'NONE', *, *, #48703, .F. ) ;
#48932 = VERTEX_POINT ( 'NONE', #7913 ) ;
#48933 = ORIENTED_EDGE ( 'NONE', *, *, #17091, .T. ) ;
#48934 = LINE ( 'NONE', #36723, #13535 ) ;
#48935 = ORIENTED_EDGE ( 'NONE', *, *, #25262, .T. ) ;
#48936 = CARTESIAN_POINT ( 'NONE',  ( 0.8282505383454039638, 1.889063466747038289, 9.894754715216722118 ) ) ;
#48937 = CARTESIAN_POINT ( 'NONE',  ( 4.641001526964560142, 33.28196331604080171, -8.016098858316199838 ) ) ;
#48938 = CARTESIAN_POINT ( 'NONE',  ( 210.0000000000000568, 0.000000000000000000, -159.1817124430720298 ) ) ;
#48939 = FACE_OUTER_BOUND ( 'NONE', #14511, .T. ) ;
#48940 = ORIENTED_EDGE ( 'NONE', *, *, #39187, .T. ) ;
#48941 = CARTESIAN_POINT ( 'NONE',  ( 2.499999999999945377, -224.9999999999999716, -240.0000000000000000 ) ) ;
#48942 = CARTESIAN_POINT ( 'NONE',  ( 151.5540265531850537, -1.025126265847089657, -80.93171244307201562 ) ) ;
#48943 = DIRECTION ( 'NONE',  ( 1.333906992743555050E-23, -1.000000000000000000, 0.000000000000000000 ) ) ;
#48944 = EDGE_LOOP ( 'NONE', ( #21608, #5805, #1346, #27020 ) ) ;
#48945 = CARTESIAN_POINT ( 'NONE',  ( 80.00000000000061107, 17.00000000000000000, -54.99999999999999289 ) ) ;
#48946 = DIRECTION ( 'NONE',  ( -0.000000000000000000, -1.000000000000000000, -0.000000000000000000 ) ) ;
#48947 = CARTESIAN_POINT ( 'NONE',  ( -0.4400426740873942810, 2.015233077865125733, 9.886433018048068178 ) ) ;
#48948 = FACE_OUTER_BOUND ( 'NONE', #46625, .T. ) ;
#48949 = ORIENTED_EDGE ( 'NONE', *, *, #41354, .F. ) ;
#48950 = CARTESIAN_POINT ( 'NONE',  ( 30.64276258327256741, 34.28040101195701794, -8.016098858316205167 ) ) ;
#48951 = EDGE_CURVE ( 'NONE', #47413, #2629, #35377, .T. ) ;
#48952 = CARTESIAN_POINT ( 'NONE',  ( 1.011271242968694084, -0.7347315653655782652, 10.00000000000000000 ) ) ;
#48953 = CARTESIAN_POINT ( 'NONE',  ( 0.3862712429686894766, -1.188820645368940276, 10.00000000000000000 ) ) ;
#48954 = CARTESIAN_POINT ( 'NONE',  ( -1.249999999999999778, 0.000000000000000000, 10.00000000000000000 ) ) ;
#48955 = ADVANCED_FACE ( 'NONE', ( #20202 ), #47610, .F. ) ;
#48956 = CARTESIAN_POINT ( 'NONE',  ( -46.69597344681494633, 1.750000000000010658, 80.81828755692798438 ) ) ;
#48957 = EDGE_CURVE ( 'NONE', #38145, #10859, #9630, .T. ) ;
#48958 = VERTEX_POINT ( 'NONE', #40719 ) ;
#48959 = CARTESIAN_POINT ( 'NONE',  ( 358.0000000000001137, 181.0000000000000284, 355.9999999999998295 ) ) ;
#48961 = EDGE_LOOP ( 'NONE', ( #42018, #41854, #6315, #46842 ) ) ;
#48960 = AXIS2_PLACEMENT_3D ( 'NONE', #1995, #34069, #2992 ) ;
#48962 = CARTESIAN_POINT ( 'NONE',  ( -8.277096487746778308, 33.14818118907697198, 7.455576670931136185 ) ) ;
#48963 = ORIENTED_EDGE ( 'NONE', *, *, #5480, .F. ) ;
#48964 = LINE ( 'NONE', #22074, #16421 ) ;
#48966 = ADVANCED_FACE ( 'NONE', ( #17608 ), #965, .T. ) ;
#48965 = CARTESIAN_POINT ( 'NONE',  ( -8.001683061421429599, -5.997755262142646870, 9.282506307616484875 ) ) ;
#48967 = EDGE_CURVE ( 'NONE', #2042, #40520, #14869, .T. ) ;
#48968 = DIRECTION ( 'NONE',  ( 0.000000000000000000, 1.000000000000000000, 0.000000000000000000 ) ) ;
#48969 = ORIENTED_EDGE ( 'NONE', *, *, #15540, .F. ) ;
#48970 = ADVANCED_FACE ( 'NONE', ( #48611 ), #41204, .T. ) ;
#48971 = CARTESIAN_POINT ( 'NONE',  ( 210.0000000000000568, 2.143131898507880377E-16, -0.9317124430720331585 ) ) ;
#48972 = VERTEX_POINT ( 'NONE', #24815 ) ;
#48973 = LINE ( 'NONE', #48479, #33088 ) ;
#48974 =( BOUNDED_CURVE ( )  B_SPLINE_CURVE ( 3, ( #7165, #27424, #35145, #31029 ),
 .UNSPECIFIED., .F., .F. ) 
 B_SPLINE_CURVE_WITH_KNOTS ( ( 4, 4 ),
 ( 1.570796326794896558, 3.141592653589793116 ),
 .UNSPECIFIED. ) 
 CURVE ( )  GEOMETRIC_REPRESENTATION_ITEM ( )  RATIONAL_B_SPLINE_CURVE ( ( 1.000000000000000000, 0.8047378541243649375, 0.8047378541243649375, 1.000000000000000000 ) ) 
 REPRESENTATION_ITEM ( '' )  );
#48975 = DIRECTION ( 'NONE',  ( 0.000000000000000000, 1.000000000000000000, 0.000000000000000000 ) ) ;
#48976 = CARTESIAN_POINT ( 'NONE',  ( 343.9999999999999432, -185.0000000000001421, -349.9999999999999432 ) ) ;
#48977 = CARTESIAN_POINT ( 'NONE',  ( 72.27890028733797578, 1.750000000000009548, -40.20683870891912193 ) ) ;
#48978 = ORIENTED_EDGE ( 'NONE', *, *, #36405, .T. ) ;
#48980 = ORIENTED_EDGE ( 'NONE', *, *, #40595, .T. ) ;
#48979 = EDGE_CURVE ( 'NONE', #1426, #5304, #44527, .T. ) ;
#48981 = CARTESIAN_POINT ( 'NONE',  ( 0.1287570809895604018, 0.3962735484563146282, 10.00000000000000000 ) ) ;
#48982 = EDGE_CURVE ( 'NONE', #18302, #43286, #17106, .T. ) ;
#48983 = EDGE_CURVE ( 'NONE', #8311, #269, #32267, .T. ) ;
#48984 = EDGE_CURVE ( 'NONE', #8311, #4051, #13751, .T. ) ;
#48985 = EDGE_LOOP ( 'NONE', ( #3748, #15910, #24376, #28662, #43182, #46376 ) ) ;
#48986 = CARTESIAN_POINT ( 'NONE',  ( 193.3040265531851105, 1.750000000000009992, -159.1817124430720298 ) ) ;
#48987 = DIRECTION ( 'NONE',  ( 0.000000000000000000, -1.000000000000000000, 0.000000000000000000 ) ) ;
#48988 = ORIENTED_EDGE ( 'NONE', *, *, #24201, .T. ) ;
#48989 = CARTESIAN_POINT ( 'NONE',  ( -168.4459734468149747, -1.025126265847089657, -37.43171244307202272 ) ) ;
#48990 = ADVANCED_FACE ( 'NONE', ( #1472 ), #12753, .F. ) ;
#48991 = ADVANCED_FACE ( 'NONE', ( #8903 ), #44281, .F. ) ;
#48992 = CARTESIAN_POINT ( 'NONE',  ( 130.0000000000012221, 16.00000000000000000, 5.000000000000004441 ) ) ;
#48993 = ORIENTED_EDGE ( 'NONE', *, *, #35625, .F. ) ;
#48994 = FACE_OUTER_BOUND ( 'NONE', #38817, .T. ) ;
#48995 = FACE_OUTER_BOUND ( 'NONE', #26353, .T. ) ;
#48996 = DIRECTION ( 'NONE',  ( -1.586032880504786307E-16, 1.654361225106055350E-24, -1.000000000000000000 ) ) ;
#48997 = CARTESIAN_POINT ( 'NONE',  ( -1.424123654778022274, -0.3625862473323341328, 9.958264684458713489 ) ) ;
#48998 = ORIENTED_EDGE ( 'NONE', *, *, #38757, .F. ) ;
#48999 = AXIS2_PLACEMENT_3D ( 'NONE', #21680, #41437, #22437 ) ;
#49000 = B_SPLINE_CURVE_WITH_KNOTS ( 'NONE', 3,
 ( #15952, #31618, #12337, #24164 ),
 .UNSPECIFIED., .F., .F.,
 ( 4, 4 ),
 ( 0.01012863361515541766, 0.01015667504234211288 ),
 .UNSPECIFIED. ) ;
#49001 = EDGE_LOOP ( 'NONE', ( #49106, #50316, #26862, #37430, #13584 ) ) ;
#49002 = CARTESIAN_POINT ( 'NONE',  ( 151.5540265531850537, 0.000000000000000000, -37.43171244307205825 ) ) ;
#49003 = CARTESIAN_POINT ( 'NONE',  ( -44.94597344681493922, -1.025126265847089213, 42.56828755692799149 ) ) ;
#49004 = CARTESIAN_POINT ( 'NONE',  ( -120.0000000000000426, 17.00000000000000000, -114.9999999999999858 ) ) ;
#49005 = CARTESIAN_POINT ( 'NONE',  ( 71.55402655318505367, 0.000000000000000000, 2.568287556928006143 ) ) ;
#49006 = CIRCLE ( 'NONE', #41665, 2.000000000000001776 ) ;
#49007 = ORIENTED_EDGE ( 'NONE', *, *, #24252, .F. ) ;
#49008 = EDGE_CURVE ( 'NONE', #43597, #28550, #40209, .T. ) ;
#49009 = CARTESIAN_POINT ( 'NONE',  ( 34.99999999999997868, 17.00000000000000000, -114.9999999999999858 ) ) ;
#49010 = ORIENTED_EDGE ( 'NONE', *, *, #808, .F. ) ;
#49011 = CARTESIAN_POINT ( 'NONE',  ( 74.32915281903215998, -1.750000000000009548, -160.2068387089191219 ) ) ;
#49012 = PLANE ( 'NONE',  #41623 ) ;
#49013 = FACE_OUTER_BOUND ( 'NONE', #50165, .T. ) ;
#49014 = EDGE_CURVE ( 'NONE', #38360, #31812, #9408, .T. ) ;
#49015 = ADVANCED_FACE ( 'NONE', ( #5555 ), #36896, .F. ) ;
#49016 = CARTESIAN_POINT ( 'NONE',  ( 151.5540265531850537, 1.025126265847089213, -160.9317124430720014 ) ) ;
#49017 = DIRECTION ( 'NONE',  ( -1.000000000000000000, -0.000000000000000000, -0.000000000000000000 ) ) ;
#49018 = DIRECTION ( 'NONE',  ( -0.000000000000000000, -1.000000000000000000, -0.000000000000000000 ) ) ;
#49019 = ORIENTED_EDGE ( 'NONE', *, *, #20459, .F. ) ;
#49020 = CARTESIAN_POINT ( 'NONE',  ( 0.9983599181300923942, 1.124146016603553733, 9.953784399990620813 ) ) ;
#49021 = EDGE_CURVE ( 'NONE', #44903, #13654, #33285, .T. ) ;
#49022 = B_SPLINE_SURFACE_WITH_KNOTS ( 'NONE', 3, 3, ( 
 ( #21053, #33877, #17709, #45125 ),
 ( #2063, #17938, #9254, #33375 ),
 ( #37241, #29006, #5396, #36740 ),
 ( #25162, #25411, #22055, #40807 ) ),
 .UNSPECIFIED., .F., .F., .F.,
 ( 4, 4 ),
 ( 4, 4 ),
 ( 0.000000000000000000, 1.000000000000000000 ),
 ( 0.000000000000000000, 1.000000000000000000 ),
 .UNSPECIFIED. ) ;
#49023 = CARTESIAN_POINT ( 'NONE',  ( 71.55402655318505367, 1.025126265847088991, -157.4317124430720582 ) ) ;
#49024 = CARTESIAN_POINT ( 'NONE',  ( 71.55402655318505367, 0.000000000000000000, 2.568287556928006143 ) ) ;
#49025 = EDGE_CURVE ( 'NONE', #6936, #27632, #33026, .T. ) ;
#49026 = CARTESIAN_POINT ( 'NONE',  ( -124.9459734468149321, -1.025126265847081219, 2.568287556927973281 ) ) ;
#49027 = EDGE_LOOP ( 'NONE', ( #37200, #34724, #46488, #44294 ) ) ;
#49028 = DIRECTION ( 'NONE',  ( -0.000000000000000000, -0.000000000000000000, 1.000000000000000000 ) ) ;
#49029 = VERTEX_POINT ( 'NONE', #40967 ) ;
#49030 = DIRECTION ( 'NONE',  ( -0.000000000000000000, -0.000000000000000000, -1.000000000000000000 ) ) ;
#49031 = CARTESIAN_POINT ( 'NONE',  ( 349.9999999999999432, -168.9999999999999432, 341.9999999999997726 ) ) ;
#49032 = CARTESIAN_POINT ( 'NONE',  ( -1.011271242968677875, -0.7347315653656004697, -10.00000000000000000 ) ) ;
#49033 = ADVANCED_FACE ( 'NONE', ( #21448 ), #45283, .F. ) ;
#49034 =( BOUNDED_CURVE ( )  B_SPLINE_CURVE ( 3, ( #10538, #2098, #6439, #6198 ),
 .UNSPECIFIED., .F., .F. ) 
 B_SPLINE_CURVE_WITH_KNOTS ( ( 4, 4 ),
 ( 0.000000000000000000, 1.570796326794896558 ),
 .UNSPECIFIED. ) 
 CURVE ( )  GEOMETRIC_REPRESENTATION_ITEM ( )  RATIONAL_B_SPLINE_CURVE ( ( 1.000000000000000000, 0.8047378541243649375, 0.8047378541243649375, 1.000000000000000000 ) ) 
 REPRESENTATION_ITEM ( '' )  );
#49035 = VECTOR ( 'NONE', #7501, 1000.000000000000000 ) ;
#49036 = CARTESIAN_POINT ( 'NONE',  ( -0.1287570809895576818, -0.3962735484563154609, -10.00000000000000000 ) ) ;
#49037 = EDGE_LOOP ( 'NONE', ( #32885, #30689, #24686, #2284, #4310 ) ) ;
#49038 = CARTESIAN_POINT ( 'NONE',  ( -114.9999999999997158, 17.00000000000000000, -60.00000000000000000 ) ) ;
#49039 = EDGE_CURVE ( 'NONE', #24656, #10537, #10916, .T. ) ;
#49041 = VECTOR ( 'NONE', #34195, 1000.000000000000000 ) ;
#49040 = LINE ( 'NONE', #2637, #26216 ) ;
#49042 = VECTOR ( 'NONE', #4565, 1000.000000000000000 ) ;
#49043 = CARTESIAN_POINT ( 'NONE',  ( 210.0000000000000568, 0.000000000000000000, 80.81828755692798438 ) ) ;
#49044 = AXIS2_PLACEMENT_3D ( 'NONE', #12791, #35909, #24360 ) ;
#49045 =( BOUNDED_CURVE ( )  B_SPLINE_CURVE ( 3, ( #29466, #44574, #48911, #9456 ),
 .UNSPECIFIED., .F., .F. ) 
 B_SPLINE_CURVE_WITH_KNOTS ( ( 4, 4 ),
 ( 0.000000000000000000, 1.570796326794896558 ),
 .UNSPECIFIED. ) 
 CURVE ( )  GEOMETRIC_REPRESENTATION_ITEM ( )  RATIONAL_B_SPLINE_CURVE ( ( 1.000000000000000000, 0.8047378541243649375, 0.8047378541243649375, 1.000000000000000000 ) ) 
 REPRESENTATION_ITEM ( '' )  );
#49046 = ORIENTED_EDGE ( 'NONE', *, *, #35549, .T. ) ;
#49047 = ORIENTED_EDGE ( 'NONE', *, *, #12533, .T. ) ;
#49048 = DIRECTION ( 'NONE',  ( 1.000000000000000000, 0.000000000000000000, -0.000000000000000000 ) ) ;
#49049 = CARTESIAN_POINT ( 'NONE',  ( 14.49999999999999822, 13.48684210526315930, -19.37312575500899570 ) ) ;
#49050 = AXIS2_PLACEMENT_3D ( 'NONE', #27002, #35484, #27267 ) ;
#49051 = ADVANCED_FACE ( 'NONE', ( #2462 ), #49615, .F. ) ;
#49052 = EDGE_CURVE ( 'NONE', #46304, #6217, #10417, .T. ) ;
#49053 = ORIENTED_EDGE ( 'NONE', *, *, #27810, .T. ) ;
#49054 = EDGE_LOOP ( 'NONE', ( #49190, #1326, #6163, #44246 ) ) ;
#49055 = CARTESIAN_POINT ( 'NONE',  ( -85.67084718096784002, -1.750000000000009548, -40.20683870891912193 ) ) ;
#49056 = CARTESIAN_POINT ( 'NONE',  ( -64.99999999999783995, 17.00000000000000000, 95.00000000000000000 ) ) ;
#49057 = CARTESIAN_POINT ( 'NONE',  ( -47.72109971266203132, 1.750000000000010436, -120.2068387089191219 ) ) ;
#49058 = LINE ( 'NONE', #25012, #8388 ) ;
#49059 = EDGE_LOOP ( 'NONE', ( #34179, #13804, #25935, #18565, #30688, #40026 ) ) ;
#49060 = EDGE_CURVE ( 'NONE', #14979, #30626, #26830, .T. ) ;
#49061 = ORIENTED_EDGE ( 'NONE', *, *, #19343, .F. ) ;
#49062 = EDGE_CURVE ( 'NONE', #7227, #3886, #45537, .T. ) ;
#49063 =( BOUNDED_CURVE ( )  B_SPLINE_CURVE ( 3, ( #7545, #34238, #22673, #38348 ),
 .UNSPECIFIED., .F., .F. ) 
 B_SPLINE_CURVE_WITH_KNOTS ( ( 4, 4 ),
 ( 3.141592653589794004, 4.712388980384689674 ),
 .UNSPECIFIED. ) 
 CURVE ( )  GEOMETRIC_REPRESENTATION_ITEM ( )  RATIONAL_B_SPLINE_CURVE ( ( 1.000000000000000000, 0.8047378541243652705, 0.8047378541243652705, 1.000000000000000000 ) ) 
 REPRESENTATION_ITEM ( '' )  );
#49064 = ADVANCED_FACE ( 'NONE', ( #41465 ), #6322, .T. ) ;
#49065 = PLANE ( 'NONE',  #11975 ) ;
#49066 = FACE_OUTER_BOUND ( 'NONE', #32120, .T. ) ;
#49067 = ORIENTED_EDGE ( 'NONE', *, *, #40264, .T. ) ;
#49068 = ORIENTED_EDGE ( 'NONE', *, *, #1734, .T. ) ;
#49069 = CARTESIAN_POINT ( 'NONE',  ( -166.6959734468149463, -1.750000000000009992, 0.8182875569279768335 ) ) ;
#49070 = CARTESIAN_POINT ( 'NONE',  ( 194.9999999999999432, -172.9999999999999716, 232.0000000000000284 ) ) ;
#49071 = VERTEX_POINT ( 'NONE', #37637 ) ;
#49072 = LINE ( 'NONE', #45493, #43615 ) ;
#49074 = ORIENTED_EDGE ( 'NONE', *, *, #34056, .T. ) ;
#49073 = VECTOR ( 'NONE', #19232, 1000.000000000000000 ) ;
#49075 = DIRECTION ( 'NONE',  ( 0.000000000000000000, 0.9749645535258950613, -0.2223603367690656918 ) ) ;
#49076 = PLANE ( 'NONE',  #43611 ) ;
#49078 = ORIENTED_EDGE ( 'NONE', *, *, #7616, .T. ) ;
#49077 = AXIS2_PLACEMENT_3D ( 'NONE', #12469, #43516, #36355 ) ;
#49079 = CARTESIAN_POINT ( 'NONE',  ( 32.27890028733795447, -1.750000000000009548, 159.7931612910809065 ) ) ;
#49080 = CARTESIAN_POINT ( 'NONE',  ( -88.44597344681497475, 0.000000000000000000, 165.0000000000000000 ) ) ;
#49081 = DIRECTION ( 'NONE',  ( 0.000000000000000000, -0.000000000000000000, -1.000000000000000000 ) ) ;
#49082 = LINE ( 'NONE', #48328, #40884 ) ;
#49083 = AXIS2_PLACEMENT_3D ( 'NONE', #13421, #16273, #8329 ) ;
#49084 = EDGE_CURVE ( 'NONE', #23039, #44300, #20115, .T. ) ;
#49085 = CARTESIAN_POINT ( 'NONE',  ( 85.00000000000090949, 16.00000000000000000, 0.000000000000000000 ) ) ;
#49086 = ORIENTED_EDGE ( 'NONE', *, *, #38811, .F. ) ;
#49088 = VECTOR ( 'NONE', #14589, 1000.000000000000000 ) ;
#49087 = CARTESIAN_POINT ( 'NONE',  ( -207.7210997126620384, 1.750000000000009548, 41.84341382277508359 ) ) ;
#49089 = CARTESIAN_POINT ( 'NONE',  ( 185.0000000000000000, -5.999999999999950262, -350.0000000000001705 ) ) ;
#49090 = CARTESIAN_POINT ( 'NONE',  ( 154.1026953830863420, 103.9380105690400597, -17.65743994998277699 ) ) ;
#49091 = DIRECTION ( 'NONE',  ( 1.000000000000000000, 0.000000000000000000, -0.000000000000000000 ) ) ;
#49092 = AXIS2_PLACEMENT_3D ( 'NONE', #36882, #33272, #44774 ) ;
#49093 = CARTESIAN_POINT ( 'NONE',  ( 0.6126904405382156416, 1.085824959725723016, 9.981352469109932457 ) ) ;
#49094 = FACE_OUTER_BOUND ( 'NONE', #31377, .T. ) ;
#49095 = LINE ( 'NONE', #25797, #22894 ) ;
#49096 = EDGE_CURVE ( 'NONE', #21827, #7894, #18107, .T. ) ;
#49097 = LINE ( 'NONE', #36874, #47479 ) ;
#49098 = DIRECTION ( 'NONE',  ( 0.000000000000000000, 5.664403186863042467E-17, 1.000000000000000000 ) ) ;
#49099 = EDGE_LOOP ( 'NONE', ( #38037, #11018, #48881, #29272, #11549, #3864 ) ) ;
#49100 = DIRECTION ( 'NONE',  ( -9.251858538542979716E-16, 0.000000000000000000, -1.000000000000000000 ) ) ;
#49101 = CARTESIAN_POINT ( 'NONE',  ( -31.93002621080269421, -9.285431160462335853, -2.408242355805840784 ) ) ;
#49102 = CARTESIAN_POINT ( 'NONE',  ( 0.000000000000000000, 183.0000000000000284, 343.9999999999997726 ) ) ;
#49103 = CARTESIAN_POINT ( 'NONE',  ( -215.0000000000000568, -175.0000000000000000, 474.0000000000000000 ) ) ;
#49104 = LINE ( 'NONE', #6047, #434 ) ;
#49105 = VERTEX_POINT ( 'NONE', #14513 ) ;
#49106 = ORIENTED_EDGE ( 'NONE', *, *, #48154, .F. ) ;
#49107 = AXIS2_PLACEMENT_3D ( 'NONE', #528, #7712, #20004 ) ;
#49108 = DIRECTION ( 'NONE',  ( 0.000000000000000000, 0.000000000000000000, 1.000000000000000000 ) ) ;
#49109 = CARTESIAN_POINT ( 'NONE',  ( 75.05402655318509630, 2.143131898507880377E-16, 39.06828755692795596 ) ) ;
#49110 = VECTOR ( 'NONE', #16155, 1000.000000000000000 ) ;
#49111 = EDGE_CURVE ( 'NONE', #4629, #37476, #502, .T. ) ;
#49112 = AXIS2_PLACEMENT_3D ( 'NONE', #23205, #39631, #31176 ) ;
#49113 = EDGE_CURVE ( 'NONE', #7079, #9194, #17855, .T. ) ;
#49114 = EDGE_LOOP ( 'NONE', ( #42360, #39348, #38005, #1574, #36661, #45494 ) ) ;
#49115 = DIRECTION ( 'NONE',  ( -0.000000000000000000, -0.000000000000000000, -1.000000000000000000 ) ) ;
#49116 = ORIENTED_EDGE ( 'NONE', *, *, #29009, .F. ) ;
#49117 = ORIENTED_EDGE ( 'NONE', *, *, #7054, .F. ) ;
#49118 = CIRCLE ( 'NONE', #8233, 2.000000000000001776 ) ;
#49119 = VERTEX_POINT ( 'NONE', #18602 ) ;
#49120 = AXIS2_PLACEMENT_3D ( 'NONE', #43364, #12573, #28243 ) ;
#49121 = EDGE_CURVE ( 'NONE', #34539, #3215, #39167, .T. ) ;
#49123 = ADVANCED_FACE ( 'NONE', ( #18851 ), #41966, .F. ) ;
#49122 = DIRECTION ( 'NONE',  ( 0.000000000000000000, 0.000000000000000000, 1.000000000000000000 ) ) ;
#49124 = CARTESIAN_POINT ( 'NONE',  ( -88.44597344681494633, -1.025126265847089435, 2.568287556927986159 ) ) ;
#49125 = EDGE_CURVE ( 'NONE', #43903, #29160, #46142, .T. ) ;
#49126 = LINE ( 'NONE', #29669, #25093 ) ;
#49127 = VECTOR ( 'NONE', #20070, 1000.000000000000000 ) ;
#49128 = ORIENTED_EDGE ( 'NONE', *, *, #46263, .T. ) ;
#49129 = FACE_OUTER_BOUND ( 'NONE', #18127, .T. ) ;
#49130 = DIRECTION ( 'NONE',  ( 0.000000000000000000, 0.000000000000000000, 1.000000000000000000 ) ) ;
#49131 =( LENGTH_UNIT ( ) NAMED_UNIT ( * ) SI_UNIT ( .MILLI., .METRE. ) );
#49132 = ORIENTED_EDGE ( 'NONE', *, *, #21153, .F. ) ;
#49133 = ORIENTED_EDGE ( 'NONE', *, *, #30838, .F. ) ;
#49134 = FACE_OUTER_BOUND ( 'NONE', #21312, .T. ) ;
#49135 = CARTESIAN_POINT ( 'NONE',  ( -33.01266944765060174, 5.813986777101691317, 1.847720168420772691 ) ) ;
#49136 = EDGE_CURVE ( 'NONE', #24507, #50669, #41309, .T. ) ;
#49137 = CARTESIAN_POINT ( 'NONE',  ( -64.99999999999940314, 16.00000000000000000, -30.00000000000000000 ) ) ;
#49138 = ORIENTED_EDGE ( 'NONE', *, *, #36112, .F. ) ;
#49139 = DIRECTION ( 'NONE',  ( 0.000000000000000000, -1.000000000000000000, 0.000000000000000000 ) ) ;
#49140 = CARTESIAN_POINT ( 'NONE',  ( -14.99999999999970868, 17.00000000000000000, -84.99999999999998579 ) ) ;
#49141 = DIRECTION ( 'NONE',  ( 0.000000000000000000, 0.000000000000000000, 1.000000000000000000 ) ) ;
#49142 = CARTESIAN_POINT ( 'NONE',  ( 72.27890028733797578, 1.750000000000009548, 41.84341382277508359 ) ) ;
#49143 = LINE ( 'NONE', #37417, #1174 ) ;
#49144 = FACE_OUTER_BOUND ( 'NONE', #22222, .T. ) ;
#49145 = CARTESIAN_POINT ( 'NONE',  ( 17.43089236541784359, 28.36237856644539690, 3.199614146704519602 ) ) ;
#49146 = DIRECTION ( 'NONE',  ( 0.000000000000000000, 0.000000000000000000, 1.000000000000000000 ) ) ;
#49147 = CARTESIAN_POINT ( 'NONE',  ( -166.6959734468149463, 1.750000000000009992, 0.8182875569279768335 ) ) ;
#49148 = VECTOR ( 'NONE', #6254, 1000.000000000000000 ) ;
#49149 = DIRECTION ( 'NONE',  ( -1.000000000000000000, 0.000000000000000000, 0.000000000000000000 ) ) ;
#49150 = AXIS2_PLACEMENT_3D ( 'NONE', #4357, #11292, #26937 ) ;
#49151 = CARTESIAN_POINT ( 'NONE',  ( 75.05402655318509630, 2.143131898507880377E-16, 165.0000000000000000 ) ) ;
#49152 = ORIENTED_EDGE ( 'NONE', *, *, #7056, .T. ) ;
#49153 = VECTOR ( 'NONE', #46044, 1000.000000000000000 ) ;
#49154 = LINE ( 'NONE', #2744, #45798 ) ;
#49155 = LINE ( 'NONE', #29703, #38971 ) ;
#49156 = VECTOR ( 'NONE', #14810, 1000.000000000000000 ) ;
#49157 = LINE ( 'NONE', #18645, #32048 ) ;
#49158 = EDGE_CURVE ( 'NONE', #7906, #28175, #15779, .T. ) ;
#49159 = ORIENTED_EDGE ( 'NONE', *, *, #4469, .F. ) ;
#49160 = B_SPLINE_CURVE_WITH_KNOTS ( 'NONE', 3,
 ( #19183, #10240, #14584, #18427 ),
 .UNSPECIFIED., .F., .F.,
 ( 4, 4 ),
 ( 0.0001535465953326398310, 0.0005837444810855714180 ),
 .UNSPECIFIED. ) ;
#49161 = DIRECTION ( 'NONE',  ( 0.000000000000000000, 0.000000000000000000, 1.000000000000000000 ) ) ;
#49162 = ORIENTED_EDGE ( 'NONE', *, *, #25525, .F. ) ;
#49163 = LINE ( 'NONE', #14556, #7502 ) ;
#49164 = DIRECTION ( 'NONE',  ( 0.000000000000000000, 0.000000000000000000, -1.000000000000000000 ) ) ;
#49165 = CARTESIAN_POINT ( 'NONE',  ( -0.2131239213568527913, -1.205185050113740219, 9.966990753365125855 ) ) ;
#49166 = CYLINDRICAL_SURFACE ( 'NONE', #23344, 1.750000000000010214 ) ;
#49167 = ORIENTED_EDGE ( 'NONE', *, *, #27143, .F. ) ;
#49168 = LINE ( 'NONE', #37686, #15092 ) ;
#49169 = EDGE_LOOP ( 'NONE', ( #1622, #7320, #30908, #27863 ) ) ;
#49170 = ORIENTED_EDGE ( 'NONE', *, *, #10770, .T. ) ;
#49171 = CARTESIAN_POINT ( 'NONE',  ( -10.00419011302953187, 8.486842105263161073, 18.42339408367722697 ) ) ;
#49172 = B_SPLINE_CURVE_WITH_KNOTS ( 'NONE', 3,
 ( #29801, #41600, #8232, #31073 ),
 .UNSPECIFIED., .F., .F.,
 ( 4, 4 ),
 ( 0.0003908573106778929595, 0.0007316046291772774005 ),
 .UNSPECIFIED. ) ;
#49173 = ORIENTED_EDGE ( 'NONE', *, *, #17972, .F. ) ;
#49174 = DIRECTION ( 'NONE',  ( 0.000000000000000000, 0.000000000000000000, -1.000000000000000000 ) ) ;
#49175 = FACE_OUTER_BOUND ( 'NONE', #19770, .T. ) ;
#49176 = ORIENTED_EDGE ( 'NONE', *, *, #14690, .F. ) ;
#49177 = FACE_OUTER_BOUND ( 'NONE', #455, .T. ) ;
#49178 = CARTESIAN_POINT ( 'NONE',  ( -46.69597344681494633, 0.000000000000000000, 165.0000000000000000 ) ) ;
#49179 = PLANE ( 'NONE',  #3847 ) ;
#49180 = ORIENTED_EDGE ( 'NONE', *, *, #36731, .T. ) ;
#49181 = CARTESIAN_POINT ( 'NONE',  ( 181.0000000000000284, 2.775557561562891351E-14, -99.00000000000014211 ) ) ;
#49182 = CIRCLE ( 'NONE', #48341, 1.750000000000015543 ) ;
#49183 = DIRECTION ( 'NONE',  ( -1.000000000000000000, 0.000000000000000000, -0.000000000000000000 ) ) ;
#49184 = ADVANCED_FACE ( 'NONE', ( #35063 ), #5628, .T. ) ;
#49185 = CARTESIAN_POINT ( 'NONE',  ( 350.0000000000000000, -184.9999999999999716, -344.0000000000001705 ) ) ;
#49186 = AXIS2_PLACEMENT_3D ( 'NONE', #37819, #14176, #46463 ) ;
#49187 = ORIENTED_EDGE ( 'NONE', *, *, #18952, .T. ) ;
#49188 = CARTESIAN_POINT ( 'NONE',  ( -114.9999999999994031, 17.00000000000000000, -30.00000000000000000 ) ) ;
#49189 = DIRECTION ( 'NONE',  ( -1.000000000000000000, -0.000000000000000000, -0.000000000000000000 ) ) ;
#49190 = ORIENTED_EDGE ( 'NONE', *, *, #32827, .F. ) ;
#49191 = ORIENTED_EDGE ( 'NONE', *, *, #48896, .T. ) ;
#49192 = ORIENTED_EDGE ( 'NONE', *, *, #44584, .F. ) ;
#49193 = CARTESIAN_POINT ( 'NONE',  ( 343.9999999999999432, -167.0000000000000853, -342.0000000000002842 ) ) ;
#49194 = EDGE_CURVE ( 'NONE', #29500, #37204, #23424, .T. ) ;
#49195 = B_SPLINE_CURVE_WITH_KNOTS ( 'NONE', 3,
 ( #16435, #7732, #31602, #4132 ),
 .UNSPECIFIED., .F., .F.,
 ( 4, 4 ),
 ( 0.000000000000000000, 0.002466147708923237085 ),
 .UNSPECIFIED. ) ;
#49196 = CARTESIAN_POINT ( 'NONE',  ( 164.9999999999999716, 16.00000000000000000, 0.000000000000000000 ) ) ;
#49197 = VECTOR ( 'NONE', #36104, 1000.000000000000000 ) ;
#49198 = ORIENTED_EDGE ( 'NONE', *, *, #15905, .F. ) ;
#49199 = FACE_OUTER_BOUND ( 'NONE', #19747, .T. ) ;
#49200 = LINE ( 'NONE', #46617, #18856 ) ;
#49201 = FACE_BOUND ( 'NONE', #32950, .T. ) ;
#49202 = DIRECTION ( 'NONE',  ( 1.000000000000000000, 0.000000000000000000, -0.000000000000000000 ) ) ;
#49203 = ORIENTED_EDGE ( 'NONE', *, *, #28799, .T. ) ;
#49204 = CYLINDRICAL_SURFACE ( 'NONE', #9253, 2.000000000000001776 ) ;
#49205 = CARTESIAN_POINT ( 'NONE',  ( -0.9870575514055066613, -1.980598328282574316, 9.881002359080278907 ) ) ;
#49206 =( BOUNDED_CURVE ( )  B_SPLINE_CURVE ( 3, ( #10128, #25787, #46002, #3170 ),
 .UNSPECIFIED., .F., .F. ) 
 B_SPLINE_CURVE_WITH_KNOTS ( ( 4, 4 ),
 ( 4.712388980384689674, 6.283185307179586232 ),
 .UNSPECIFIED. ) 
 CURVE ( )  GEOMETRIC_REPRESENTATION_ITEM ( )  RATIONAL_B_SPLINE_CURVE ( ( 1.000000000000000000, 0.8047378541243649375, 0.8047378541243649375, 1.000000000000000000 ) ) 
 REPRESENTATION_ITEM ( '' )  );
#49207 = CARTESIAN_POINT ( 'NONE',  ( -44.99506233596265048, -23.32283626942287569, 7.455576670931136185 ) ) ;
#49208 = ORIENTED_EDGE ( 'NONE', *, *, #25508, .F. ) ;
#49209 = ITEM_DEFINED_TRANSFORMATION ( 'NONE', 'NONE', #17649,  #30773 ) ;
#49210 = CARTESIAN_POINT ( 'NONE',  ( 115.0540265531850395, 2.143131898507847836E-16, -117.4317124430720725 ) ) ;
#49211 = DIRECTION ( 'NONE',  ( 0.000000000000000000, 0.000000000000000000, -1.000000000000000000 ) ) ;
#49212 = CARTESIAN_POINT ( 'NONE',  ( -10.70590866674912967, 12.76446523155714985, -3.546734833711462365 ) ) ;
#49213 = LINE ( 'NONE', #45126, #19925 ) ;
#49214 = ORIENTED_EDGE ( 'NONE', *, *, #34452, .F. ) ;
#49215 = CARTESIAN_POINT ( 'NONE',  ( 111.5540265531850537, 1.025126265847081886, -80.93171244307201562 ) ) ;
#49216 = CARTESIAN_POINT ( 'NONE',  ( 23.82716369509147825, 44.49195112876006419, 8.356839323120299312 ) ) ;
#49217 = CARTESIAN_POINT ( 'NONE',  ( -47.22310614333779455, -16.46562252335923660, -3.760136334089591248 ) ) ;
#49218 = CARTESIAN_POINT ( 'NONE',  ( 0.8282505383454039638, 1.889063466747038289, 9.894754715216722118 ) ) ;
#49219 = CARTESIAN_POINT ( 'NONE',  ( -87.72109971266203843, 1.750000000000009548, 161.8434138227750907 ) ) ;
#49220 = ADVANCED_FACE ( 'NONE', ( #31448 ), #19880, .F. ) ;
#49221 = VECTOR ( 'NONE', #41654, 1000.000000000000000 ) ;
#49222 = VERTEX_POINT ( 'NONE', #38901 ) ;
#49223 = CARTESIAN_POINT ( 'NONE',  ( 355.9999999999999432, -185.0000000000000284, 359.9999999999998295 ) ) ;
#49224 = ORIENTED_EDGE ( 'NONE', *, *, #12159, .T. ) ;
#49225 = EDGE_LOOP ( 'NONE', ( #11690, #21379, #21912, #8219 ) ) ;
#49226 = DIRECTION ( 'NONE',  ( -0.000000000000000000, -1.000000000000000000, -0.000000000000000000 ) ) ;
#49227 = VECTOR ( 'NONE', #11465, 1000.000000000000000 ) ;
#49228 = CARTESIAN_POINT ( 'NONE',  ( 35.00000000000061107, 16.00000000000000000, -30.00000000000000000 ) ) ;
#49229 = VECTOR ( 'NONE', #4673, 1000.000000000000000 ) ;
#49230 = CARTESIAN_POINT ( 'NONE',  ( -165.6708471809677974, -1.750000000000009548, 161.8434138227750907 ) ) ;
#49231 = ORIENTED_EDGE ( 'NONE', *, *, #32170, .F. ) ;
#49232 = DIRECTION ( 'NONE',  ( 0.000000000000000000, 0.000000000000000000, -1.000000000000000000 ) ) ;
#49233 = ORIENTED_EDGE ( 'NONE', *, *, #9846, .F. ) ;
#49234 = DIRECTION ( 'NONE',  ( -0.000000000000000000, -1.000000000000000000, -0.000000000000000000 ) ) ;
#49235 = CARTESIAN_POINT ( 'NONE',  ( -124.9459734468149321, -1.025126265847081442, -0.9317124430720195027 ) ) ;
#49236 = CARTESIAN_POINT ( 'NONE',  ( 169.0000000000000284, 175.0000000000000284, 341.9999999999998863 ) ) ;
#49237 = DIRECTION ( 'NONE',  ( -0.000000000000000000, -0.000000000000000000, 1.000000000000000000 ) ) ;
#49238 = CARTESIAN_POINT ( 'NONE',  ( -36.08557433729204433, 35.58569447144795106, 7.455576670931136185 ) ) ;
#49239 = ORIENTED_EDGE ( 'NONE', *, *, #13923, .F. ) ;
#49240 = ORIENTED_EDGE ( 'NONE', *, *, #28567, .F. ) ;
#49241 = CARTESIAN_POINT ( 'NONE',  ( -49.89397392339119364, 8.245536726717011433, 7.906207997025717304 ) ) ;
#49242 = ORIENTED_EDGE ( 'NONE', *, *, #22109, .T. ) ;
#49243 = CARTESIAN_POINT ( 'NONE',  ( -210.0000000000000568, 0.000000000000000000, -79.18171244307201562 ) ) ;
#49244 = CARTESIAN_POINT ( 'NONE',  ( 164.9999999999999716, 16.00000000000000000, 115.0000000000000142 ) ) ;
#49245 = VERTEX_POINT ( 'NONE', #35826 ) ;
#49246 = CARTESIAN_POINT ( 'NONE',  ( 135.0000000000019043, 16.00000000000000000, 90.00000000000000000 ) ) ;
#49247 = EDGE_CURVE ( 'NONE', #14517, #11426, #11429, .T. ) ;
#49248 = VECTOR ( 'NONE', #15731, 1000.000000000000000 ) ;
#49249 = AXIS2_PLACEMENT_3D ( 'NONE', #46559, #47324, #35586 ) ;
#49250 = CARTESIAN_POINT ( 'NONE',  ( -167.7210997126620384, 1.750000000000010436, 79.79316129108087807 ) ) ;
#49251 = VERTEX_POINT ( 'NONE', #31958 ) ;
#49252 = DIRECTION ( 'NONE',  ( -4.758098676964954489E-16, -1.000000000000000000, -1.751623080406021339E-46 ) ) ;
#49253 = CARTESIAN_POINT ( 'NONE',  ( 0.3862712429686810944, 1.188820645368943607, 10.00000000000000000 ) ) ;
#49254 = LINE ( 'NONE', #30571, #37286 ) ;
#49255 = LINE ( 'NONE', #8855, #9075 ) ;
#49256 = CARTESIAN_POINT ( 'NONE',  ( -4.945973446814903696, 2.143131898507912917E-16, 82.56828755692801280 ) ) ;
#49257 = ORIENTED_EDGE ( 'NONE', *, *, #14454, .T. ) ;
#49258 = AXIS2_PLACEMENT_3D ( 'NONE', #24166, #39822, #4660 ) ;
#49259 = ORIENTED_EDGE ( 'NONE', *, *, #19335, .T. ) ;
#49260 = CARTESIAN_POINT ( 'NONE',  ( 85.00000000000123634, 16.00000000000000000, 5.000000000000004441 ) ) ;
#49261 = CARTESIAN_POINT ( 'NONE',  ( -20.00000000000003197, 17.00000000000000000, -114.9999999999999858 ) ) ;
#49262 = ADVANCED_FACE ( 'NONE', ( #4490 ), #40869, .T. ) ;
#49263 = DIRECTION ( 'NONE',  ( 0.000000000000000000, 1.000000000000000000, 0.000000000000000000 ) ) ;
#49264 = DIRECTION ( 'NONE',  ( 0.000000000000000000, 0.000000000000000000, 1.000000000000000000 ) ) ;
#49265 = ORIENTED_EDGE ( 'NONE', *, *, #43773, .F. ) ;
#49266 = ADVANCED_FACE ( 'NONE', ( #8097 ), #23742, .T. ) ;
#49267 = LINE ( 'NONE', #25722, #7824 ) ;
#49268 = ORIENTED_EDGE ( 'NONE', *, *, #34192, .T. ) ;
#49269 = EDGE_CURVE ( 'NONE', #1551, #6362, #34803, .T. ) ;
#49270 = CARTESIAN_POINT ( 'NONE',  ( 75.05402655318509630, 2.143131898507880377E-16, -120.9317124430720725 ) ) ;
#49271 = CARTESIAN_POINT ( 'NONE',  ( 0.1425549192113746144, -1.238581250503543618, 9.981352469109934233 ) ) ;
#49272 = CARTESIAN_POINT ( 'NONE',  ( 183.0000000000000000, -81.49999999999995737, -115.0000000000001563 ) ) ;
#49273 = CARTESIAN_POINT ( 'NONE',  ( 153.3040265531850537, 1.750000000000009992, -159.1817124430720298 ) ) ;
#49274 = DIRECTION ( 'NONE',  ( -1.000000000000000000, 0.000000000000000000, 0.000000000000000000 ) ) ;
#49275 = ORIENTED_EDGE ( 'NONE', *, *, #7121, .T. ) ;
#49276 = CYLINDRICAL_SURFACE ( 'NONE', #9164, 4.000000000000003553 ) ;
#49277 = PLANE ( 'NONE',  #44092 ) ;
#49278 = CARTESIAN_POINT ( 'NONE',  ( 33.30402655318503946, -1.750000000000009992, -159.1817124430720298 ) ) ;
#49279 = EDGE_CURVE ( 'NONE', #5910, #30190, #42709, .T. ) ;
#49280 = ADVANCED_FACE ( 'NONE', ( #43980 ), #5246, .F. ) ;
#49281 = EDGE_CURVE ( 'NONE', #46895, #28486, #27006, .T. ) ;
#49282 = DIRECTION ( 'NONE',  ( -0.000000000000000000, -1.000000000000000000, -0.000000000000000000 ) ) ;
#49283 = EDGE_LOOP ( 'NONE', ( #16191, #20194, #26590, #12409 ) ) ;
#49284 =( BOUNDED_CURVE ( )  B_SPLINE_CURVE ( 3, ( #40821, #13109, #5666, #24931 ),
 .UNSPECIFIED., .F., .F. ) 
 B_SPLINE_CURVE_WITH_KNOTS ( ( 4, 4 ),
 ( 0.000000000000000000, 1.570796326794896558 ),
 .UNSPECIFIED. ) 
 CURVE ( )  GEOMETRIC_REPRESENTATION_ITEM ( )  RATIONAL_B_SPLINE_CURVE ( ( 1.000000000000000000, 0.8047378541243649375, 0.8047378541243649375, 1.000000000000000000 ) ) 
 REPRESENTATION_ITEM ( '' )  );
#49285 = CARTESIAN_POINT ( 'NONE',  ( -204.9459734468149463, 2.143131898507880377E-16, 165.0000000000000000 ) ) ;
#49286 = VERTEX_POINT ( 'NONE', #44474 ) ;
#49287 = FACE_OUTER_BOUND ( 'NONE', #5267, .T. ) ;
#49288 = AXIS2_PLACEMENT_3D ( 'NONE', #33116, #1799, #13590 ) ;
#49289 = DIRECTION ( 'NONE',  ( -0.000000000000000000, -0.000000000000000000, -1.000000000000000000 ) ) ;
#49290 = VERTEX_POINT ( 'NONE', #24762 ) ;
#49291 = AXIS2_PLACEMENT_3D ( 'NONE', #24137, #23872, #19242 ) ;
#49292 = DIRECTION ( 'NONE',  ( -0.000000000000000000, -1.000000000000000000, -0.000000000000000000 ) ) ;
#49293 = ORIENTED_EDGE ( 'NONE', *, *, #30180, .F. ) ;
#49294 = CYLINDRICAL_SURFACE ( 'NONE', #7458, 1.750000000000008438 ) ;
#49295 = CARTESIAN_POINT ( 'NONE',  ( -1.553101183265242602, -0.2460239823947171223, 9.927288994922816912 ) ) ;
#49296 = CARTESIAN_POINT ( 'NONE',  ( 194.9999999999999432, 173.0000000000000000, 372.0000000000000000 ) ) ;
#49297 = VERTEX_POINT ( 'NONE', #12690 ) ;
#49298 = VERTEX_POINT ( 'NONE', #1907 ) ;
#49299 = EDGE_CURVE ( 'NONE', #40803, #49373, #46303, .T. ) ;
#49300 = CYLINDRICAL_SURFACE ( 'NONE', #4626, 0.5000000000000004441 ) ;
#49301 = CARTESIAN_POINT ( 'NONE',  ( 46.10908423965007330, 19.89422939639137766, 1.847720168420772691 ) ) ;
#49302 = ADVANCED_FACE ( 'NONE', ( #16801 ), #32205, .T. ) ;
#49303 = EDGE_LOOP ( 'NONE', ( #41595, #49132, #48320, #38977 ) ) ;
#49304 = EDGE_CURVE ( 'NONE', #40397, #715, #27844, .T. ) ;
#49305 = ORIENTED_EDGE ( 'NONE', *, *, #50285, .T. ) ;
#49306 = DIRECTION ( 'NONE',  ( -0.000000000000000000, -0.000000000000000000, -1.000000000000000000 ) ) ;
#49307 = LINE ( 'NONE', #44729, #35468 ) ;
#49308 = VERTEX_POINT ( 'NONE', #29107 ) ;
#49309 = CARTESIAN_POINT ( 'NONE',  ( 115.0540265531850395, -1.025126265847081219, -157.4317124430720582 ) ) ;
#49310 = EDGE_CURVE ( 'NONE', #7014, #17256, #41094, .T. ) ;
#49311 = ORIENTED_EDGE ( 'NONE', *, *, #28761, .F. ) ;
#49312 = AXIS2_PLACEMENT_3D ( 'NONE', #47553, #33723, #33472 ) ;
#49313 = EDGE_CURVE ( 'NONE', #19392, #49920, #20385, .T. ) ;
#49314 = CARTESIAN_POINT ( 'NONE',  ( 80.00000000000186162, 16.00000000000000000, 65.00000000000000000 ) ) ;
#49315 = DIRECTION ( 'NONE',  ( 0.000000000000000000, 0.000000000000000000, 1.000000000000000000 ) ) ;
#49316 = ORIENTED_EDGE ( 'NONE', *, *, #11822, .F. ) ;
#49317 = VECTOR ( 'NONE', #50654, 1000.000000000000000 ) ;
#49318 = ORIENTED_EDGE ( 'NONE', *, *, #16445, .T. ) ;
#49319 = PLANE ( 'NONE',  #28414 ) ;
#49320 = VECTOR ( 'NONE', #22358, 1000.000000000000000 ) ;
#49321 = DIRECTION ( 'NONE',  ( 0.000000000000000000, 0.000000000000000000, 1.000000000000000000 ) ) ;
#49322 = EDGE_LOOP ( 'NONE', ( #24364, #25387, #47450, #8450 ) ) ;
#49323 = CARTESIAN_POINT ( 'NONE',  ( 50.00000000000000000, -50.00000000000000000, 900.0000000000000000 ) ) ;
#49324 = ORIENTED_EDGE ( 'NONE', *, *, #5550, .F. ) ;
#49325 = VECTOR ( 'NONE', #31366, 1000.000000000000000 ) ;
#49326 = CYLINDRICAL_SURFACE ( 'NONE', #34006, 1.750000000000036193 ) ;
#49327 = ORIENTED_EDGE ( 'NONE', *, *, #44797, .T. ) ;
#49328 = DIRECTION ( 'NONE',  ( -0.000000000000000000, -0.000000000000000000, -1.000000000000000000 ) ) ;
#49329 = CARTESIAN_POINT ( 'NONE',  ( -167.7210997126620384, -1.750000000000009548, -40.20683870891912193 ) ) ;
#49330 = FACE_OUTER_BOUND ( 'NONE', #1976, .T. ) ;
#49331 = LINE ( 'NONE', #25785, #48202 ) ;
#49332 = LINE ( 'NONE', #37366, #32337 ) ;
#49333 = VERTEX_POINT ( 'NONE', #9353 ) ;
#49334 = CARTESIAN_POINT ( 'NONE',  ( 181.0000000000000284, -174.9999999999999716, -111.0000000000001563 ) ) ;
#49335 = CYLINDRICAL_SURFACE ( 'NONE', #34709, 1.750000000000008438 ) ;
#49336 = B_SPLINE_SURFACE_WITH_KNOTS ( 'NONE', 3, 3, ( 
 ( #43252, #35843, #37361, #44248 ),
 ( #21165, #24782, #9869, #13716 ),
 ( #17067, #17818, #25033, #1433 ),
 ( #40429, #1928, #8863, #36851 ) ),
 .UNSPECIFIED., .F., .F., .F.,
 ( 4, 4 ),
 ( 4, 4 ),
 ( 0.000000000000000000, 1.000000000000000000 ),
 ( 0.000000000000000000, 1.000000000000000000 ),
 .UNSPECIFIED. ) ;
#49337 = CARTESIAN_POINT ( 'NONE',  ( -168.4459734468149463, 0.000000000000000000, -157.4317124430720582 ) ) ;
#49338 = CARTESIAN_POINT ( 'NONE',  ( 154.1026953830863420, -98.56198943095992604, 22.84256005001721945 ) ) ;
#49339 = ADVANCED_FACE ( 'NONE', ( #5497 ), #48301, .T. ) ;
#49340 = EDGE_CURVE ( 'NONE', #18024, #20654, #32465, .T. ) ;
#49341 =( BOUNDED_CURVE ( )  B_SPLINE_CURVE ( 3, ( #31702, #42957, #136, #38890 ),
 .UNSPECIFIED., .F., .F. ) 
 B_SPLINE_CURVE_WITH_KNOTS ( ( 4, 4 ),
 ( 0.000000000000000000, 1.570796326794896558 ),
 .UNSPECIFIED. ) 
 CURVE ( )  GEOMETRIC_REPRESENTATION_ITEM ( )  RATIONAL_B_SPLINE_CURVE ( ( 1.000000000000000000, 0.8047378541243649375, 0.8047378541243649375, 1.000000000000000000 ) ) 
 REPRESENTATION_ITEM ( '' )  );
#49342 = EDGE_CURVE ( 'NONE', #19122, #8719, #1163, .T. ) ;
#49343 = EDGE_CURVE ( 'NONE', #43927, #31351, #41272, .T. ) ;
#49344 = DIRECTION ( 'NONE',  ( -0.000000000000000000, -0.000000000000000000, -1.000000000000000000 ) ) ;
#49345 = CARTESIAN_POINT ( 'NONE',  ( 191.5540265531851105, 0.000000000000000000, 79.06828755692797017 ) ) ;
#49346 = EDGE_CURVE ( 'NONE', #29552, #39659, #21147, .T. ) ;
#49347 = DIRECTION ( 'NONE',  ( 2.958228394578793832E-31, 0.000000000000000000, 1.000000000000000000 ) ) ;
#49348 = CARTESIAN_POINT ( 'NONE',  ( -194.9999999999999432, -172.9999999999999716, 232.0000000000000284 ) ) ;
#49349 =( BOUNDED_CURVE ( )  B_SPLINE_CURVE ( 3, ( #12599, #46958, #43899, #27510 ),
 .UNSPECIFIED., .F., .F. ) 
 B_SPLINE_CURVE_WITH_KNOTS ( ( 4, 4 ),
 ( 4.712388980384689674, 6.283185307179586232 ),
 .UNSPECIFIED. ) 
 CURVE ( )  GEOMETRIC_REPRESENTATION_ITEM ( )  RATIONAL_B_SPLINE_CURVE ( ( 1.000000000000000000, 0.8047378541243649375, 0.8047378541243649375, 1.000000000000000000 ) ) 
 REPRESENTATION_ITEM ( '' )  );
#49350 = VECTOR ( 'NONE', #13135, 1000.000000000000000 ) ;
#49351 = EDGE_CURVE ( 'NONE', #22127, #5410, #44727, .T. ) ;
#49352 = CARTESIAN_POINT ( 'NONE',  ( 0.3862712429686978033, -1.188820645368937834, 10.00000000000000000 ) ) ;
#49353 = ORIENTED_EDGE ( 'NONE', *, *, #12405, .T. ) ;
#49354 = PLANE ( 'NONE',  #2703 ) ;
#49355 = LINE ( 'NONE', #33510, #13946 ) ;
#49356 = CARTESIAN_POINT ( 'NONE',  ( 152.2789002873379900, -1.750000000000009548, 41.84341382277508359 ) ) ;
#49357 = LINE ( 'NONE', #39089, #14190 ) ;
#49358 = CARTESIAN_POINT ( 'NONE',  ( 37.09740935455766220, -5.526036232978249529, 8.506357886886739550 ) ) ;
#49359 = VECTOR ( 'NONE', #32800, 1000.000000000000000 ) ;
#49360 = EDGE_LOOP ( 'NONE', ( #1555, #39808, #43041, #49788 ) ) ;
#49361 = VERTEX_POINT ( 'NONE', #17301 ) ;
#49362 = CARTESIAN_POINT ( 'NONE',  ( 0.5000000000000000000, -0.5000000000000000000, 1000.000000000000000 ) ) ;
#49363 =( GEOMETRIC_REPRESENTATION_CONTEXT ( 3 ) GLOBAL_UNCERTAINTY_ASSIGNED_CONTEXT ( ( #11700 ) ) GLOBAL_UNIT_ASSIGNED_CONTEXT ( ( #951, #8143, #42750 ) ) REPRESENTATION_CONTEXT ( 'NONE', 'WORKASPACE' ) );
#49364 = DIRECTION ( 'NONE',  ( -1.000000000000000000, 0.000000000000000000, 0.000000000000000000 ) ) ;
#49365 = EDGE_CURVE ( 'NONE', #19154, #48435, #32972, .T. ) ;
#49366 = ORIENTED_EDGE ( 'NONE', *, *, #11809, .T. ) ;
#49367 = ADVANCED_FACE ( 'NONE', ( #40905 ), #6270, .F. ) ;
#49368 = AXIS2_PLACEMENT_3D ( 'NONE', #6303, #49344, #40942 ) ;
#49369 = CARTESIAN_POINT ( 'NONE',  ( 2.462075149652696027, -16.57295996686994499, 9.403735324607438884 ) ) ;
#49370 = DIRECTION ( 'NONE',  ( 1.000000000000000000, 0.000000000000000000, 0.000000000000000000 ) ) ;
#49371 = ORIENTED_EDGE ( 'NONE', *, *, #7400, .T. ) ;
#49372 = ORIENTED_EDGE ( 'NONE', *, *, #8408, .T. ) ;
#49373 = VERTEX_POINT ( 'NONE', #2885 ) ;
#49374 = PRODUCT_RELATED_PRODUCT_CATEGORY ( 'part', '', ( #14677 ) ) ;
#49375 = FACE_OUTER_BOUND ( 'NONE', #29350, .T. ) ;
#49376 = FACE_OUTER_BOUND ( 'NONE', #10850, .T. ) ;
#49377 = LINE ( 'NONE', #45789, #20987 ) ;
#49378 = ORIENTED_EDGE ( 'NONE', *, *, #3670, .F. ) ;
#49379 = CARTESIAN_POINT ( 'NONE',  ( 8.277096487746778308, -33.14818118907697198, 7.455576670931136185 ) ) ;
#49380 = CARTESIAN_POINT ( 'NONE',  ( 73.30402655318508209, -1.750000000000010658, 80.81828755692798438 ) ) ;
#49381 = FACE_OUTER_BOUND ( 'NONE', #10274, .T. ) ;
#49382 = ORIENTED_EDGE ( 'NONE', *, *, #6688, .T. ) ;
#49383 = ORIENTED_EDGE ( 'NONE', *, *, #37617, .F. ) ;
#49384 = CYLINDRICAL_SURFACE ( 'NONE', #45867, 1.750000000000001554 ) ;
#49385 = EDGE_CURVE ( 'NONE', #19838, #21347, #37832, .T. ) ;
#49386 = CARTESIAN_POINT ( 'NONE',  ( 30.00000000000123279, 17.00000000000000000, 5.000000000000004441 ) ) ;
#49387 = LINE ( 'NONE', #49137, #16850 ) ;
#49388 = ORIENTED_EDGE ( 'NONE', *, *, #3828, .T. ) ;
#49389 = CARTESIAN_POINT ( 'NONE',  ( -1.424123654778022274, -0.3625862473323341328, 9.958264684458713489 ) ) ;
#49390 = DIRECTION ( 'NONE',  ( 0.000000000000000000, 0.000000000000000000, -1.000000000000000000 ) ) ;
#49391 = CARTESIAN_POINT ( 'NONE',  ( 33.30402655318503946, 1.750000000000010658, -119.1817124430720440 ) ) ;
#49392 = CARTESIAN_POINT ( 'NONE',  ( 153.3040265531850537, 0.000000000000000000, 165.0000000000000000 ) ) ;
#49393 = VECTOR ( 'NONE', #44085, 1000.000000000000000 ) ;
#49394 = EDGE_CURVE ( 'NONE', #6937, #20029, #45974, .T. ) ;
#49395 = DIRECTION ( 'NONE',  ( 0.000000000000000000, 1.000000000000000000, 0.000000000000000000 ) ) ;
#49396 = VERTEX_POINT ( 'NONE', #21914 ) ;
#49397 =( NAMED_UNIT ( * ) SI_UNIT ( $, .STERADIAN. ) SOLID_ANGLE_UNIT ( ) );
#49398 = VECTOR ( 'NONE', #28508, 1000.000000000000000 ) ;
#49399 = CARTESIAN_POINT ( 'NONE',  ( 115.0540265531850395, -1.025126265847081219, 2.568287556927973281 ) ) ;
#49400 = CARTESIAN_POINT ( 'NONE',  ( -44.94597344681493922, 1.025126265847089213, -160.9317124430720014 ) ) ;
#49401 = FACE_OUTER_BOUND ( 'NONE', #25265, .T. ) ;
#49402 = PRESENTATION_LAYER_ASSIGNMENT (  '', '', ( #6856 ) ) ;
#49403 = CARTESIAN_POINT ( 'NONE',  ( -12.15085308559838317, 11.68662139125813226, 2.590526750877053086 ) ) ;
#49404 = EDGE_CURVE ( 'NONE', #45594, #27492, #38868, .T. ) ;
#49405 = EDGE_CURVE ( 'NONE', #1663, #35301, #33966, .T. ) ;
#49406 = COLOUR_RGB ( '',0.7921568627450980005, 0.8196078431372548767, 0.9333333333333333481 ) ;
#49407 = CARTESIAN_POINT ( 'NONE',  ( -6.695973446814940111, 0.000000000000000000, 165.0000000000000000 ) ) ;
#49408 = ORIENTED_EDGE ( 'NONE', *, *, #18666, .F. ) ;
#49409 = CARTESIAN_POINT ( 'NONE',  ( 0.000000000000000000, 0.000000000000000000, 800.0000000000000000 ) ) ;
#49410 = ADVANCED_FACE ( 'NONE', ( #14710 ), #13696, .T. ) ;
#49411 = FACE_OUTER_BOUND ( 'NONE', #46302, .T. ) ;
#49412 = FACE_OUTER_BOUND ( 'NONE', #5350, .T. ) ;
#49413 = EDGE_CURVE ( 'NONE', #37687, #21893, #25382, .T. ) ;
#49414 = ADVANCED_FACE ( 'NONE', ( #34479 ), #29359, .T. ) ;
#49415 = ORIENTED_EDGE ( 'NONE', *, *, #16489, .T. ) ;
#49416 = CARTESIAN_POINT ( 'NONE',  ( -14.99999999999876366, 16.00000000000000000, 5.000000000000004441 ) ) ;
#49417 = ORIENTED_EDGE ( 'NONE', *, *, #50496, .F. ) ;
#49418 = CARTESIAN_POINT ( 'NONE',  ( 0.000000000000000000, 23.48684210526316107, 0.000000000000000000 ) ) ;
#49419 = CARTESIAN_POINT ( 'NONE',  ( -14.99999999999876366, 17.00000000000000000, 30.00000000000000000 ) ) ;
#49420 = DIRECTION ( 'NONE',  ( 1.000000000000000000, 0.000000000000000000, -0.000000000000000000 ) ) ;
#49421 = CARTESIAN_POINT ( 'NONE',  ( 224.9999999999999716, -164.9999999999999716, 62.29650858650038003 ) ) ;
#49422 = EDGE_CURVE ( 'NONE', #37462, #4392, #14188, .T. ) ;
#49423 = EDGE_LOOP ( 'NONE', ( #43502, #34823, #48412, #18179, #9321, #42578 ) ) ;
#49424 = CARTESIAN_POINT ( 'NONE',  ( -225.0000000000000284, -174.9999999999999716, 500.0000000000001137 ) ) ;
#49425 = ORIENTED_EDGE ( 'NONE', *, *, #16129, .F. ) ;
#49426 = EDGE_LOOP ( 'NONE', ( #7651, #45826, #21929, #7586, #19690, #36067 ) ) ;
#49427 = CARTESIAN_POINT ( 'NONE',  ( -87.72109971266203843, -1.750000000000009548, -38.15658617722494483 ) ) ;
#49428 = ORIENTED_EDGE ( 'NONE', *, *, #12796, .F. ) ;
#49429 = CARTESIAN_POINT ( 'NONE',  ( 210.0000000000000568, 0.000000000000000000, -77.43171244307200141 ) ) ;
#49430 = CYLINDRICAL_SURFACE ( 'NONE', #26552, 1.750000000000010214 ) ;
#49431 = VECTOR ( 'NONE', #25374, 1000.000000000000000 ) ;
#49432 = CARTESIAN_POINT ( 'NONE',  ( 0.5000000000000000000, 0.5000000000000000000, 1000.000000000000000 ) ) ;
#49433 = AXIS2_PLACEMENT_3D ( 'NONE', #49407, #2499, #6600 ) ;
#49434 = CARTESIAN_POINT ( 'NONE',  ( 75.05402655318509630, -1.025126265847089213, -0.9317124430720324924 ) ) ;
#49435 = DIRECTION ( 'NONE',  ( 0.000000000000000000, 1.000000000000000000, 1.544785076050074834E-48 ) ) ;
#49436 = ORIENTED_EDGE ( 'NONE', *, *, #17121, .T. ) ;
#49437 = AXIS2_PLACEMENT_3D ( 'NONE', #10713, #38693, #6874 ) ;
#49438 = CARTESIAN_POINT ( 'NONE',  ( 24.47767542868285062, -23.18653802921781448, 8.807470649214879543 ) ) ;
#49439 = VECTOR ( 'NONE', #18193, 1000.000000000000000 ) ;
#49440 = DIRECTION ( 'NONE',  ( 0.000000000000000000, 1.000000000000000000, 0.000000000000000000 ) ) ;
#49441 = EDGE_LOOP ( 'NONE', ( #39275, #6427, #30247, #5742, #19815 ) ) ;
#49442 = LINE ( 'NONE', #6636, #40716 ) ;
#49443 = DIRECTION ( 'NONE',  ( -0.000000000000000000, -0.000000000000000000, -1.000000000000000000 ) ) ;
#49444 = ORIENTED_EDGE ( 'NONE', *, *, #35287, .T. ) ;
#49445 = ORIENTED_EDGE ( 'NONE', *, *, #45095, .T. ) ;
#49446 = ORIENTED_EDGE ( 'NONE', *, *, #18899, .F. ) ;
#49447 = LINE ( 'NONE', #2538, #12284 ) ;
#49448 = DIRECTION ( 'NONE',  ( -1.000000000000000000, 0.000000000000000000, 0.000000000000000000 ) ) ;
#49449 = B_SPLINE_SURFACE_WITH_KNOTS ( 'NONE', 3, 3, ( 
 ( #28147, #12479, #13235, #25299 ),
 ( #43781, #44025, #36367, #48600 ),
 ( #24310, #20949, #28898, #1209 ),
 ( #5543, #39956, #36634, #4780 ) ),
 .UNSPECIFIED., .F., .F., .F.,
 ( 4, 4 ),
 ( 4, 4 ),
 ( 0.000000000000000000, 1.000000000000000000 ),
 ( 0.000000000000000000, 1.000000000000000000 ),
 .UNSPECIFIED. ) ;
#49450 = EDGE_LOOP ( 'NONE', ( #36279, #47252, #25313, #9741 ) ) ;
#49451 = EDGE_CURVE ( 'NONE', #375, #39210, #41147, .T. ) ;
#49452 = DIRECTION ( 'NONE',  ( -1.000000000000000000, -0.000000000000000000, -0.000000000000000000 ) ) ;
#49453 = FACE_BOUND ( 'NONE', #26689, .T. ) ;
#49454 = VECTOR ( 'NONE', #7614, 1000.000000000000000 ) ;
#49455 = CARTESIAN_POINT ( 'NONE',  ( -128.4459734468149179, 0.000000000000000000, 42.56828755692794175 ) ) ;
#49456 = EDGE_LOOP ( 'NONE', ( #46178, #43304, #13953, #24359 ) ) ;
#49457 = CARTESIAN_POINT ( 'NONE',  ( 5.320787806771834383, -8.466948512617054945, 0.000000000000000000 ) ) ;
#49458 = PRESENTATION_STYLE_ASSIGNMENT (( #37980 ) ) ;
#49459 = CARTESIAN_POINT ( 'NONE',  ( 1.011271242968688311, -0.7347315653655855927, 3.333333333333333481 ) ) ;
#49460 = ORIENTED_EDGE ( 'NONE', *, *, #46193, .T. ) ;
#49461 = CONTEXT_DEPENDENT_SHAPE_REPRESENTATION ( #24037, #19622 ) ;
#49462 = CARTESIAN_POINT ( 'NONE',  ( -165.0000000000000284, 17.00000000000000000, 115.0000000000000142 ) ) ;
#49463 = LINE ( 'NONE', #23580, #47046 ) ;
#49464 = EDGE_CURVE ( 'NONE', #1049, #20141, #26714, .T. ) ;
#49465 = EDGE_CURVE ( 'NONE', #49565, #41616, #10017, .T. ) ;
#49466 = VECTOR ( 'NONE', #33780, 1000.000000000000000 ) ;
#49467 = CARTESIAN_POINT ( 'NONE',  ( 80.00000000000217426, 16.00000000000000000, 115.0000000000000142 ) ) ;
#49468 = CARTESIAN_POINT ( 'NONE',  ( 31.55402655318503236, 0.000000000000000000, 79.06828755692797017 ) ) ;
#49469 = ORIENTED_EDGE ( 'NONE', *, *, #13464, .F. ) ;
#49470 = CYLINDRICAL_SURFACE ( 'NONE', #19778, 1.750000000000008438 ) ;
#49471 = CIRCLE ( 'NONE', #5275, 2.000000000000001776 ) ;
#49472 = CARTESIAN_POINT ( 'NONE',  ( 13.92102703536701114, 30.85732372859822803, 8.356839323120299312 ) ) ;
#49473 = CARTESIAN_POINT ( 'NONE',  ( 210.0000000000000568, 0.000000000000000000, 120.8182875569279702 ) ) ;
#49474 = CARTESIAN_POINT ( 'NONE',  ( -126.6959734468149321, 1.749999999999997335, 120.8182875569279702 ) ) ;
#49475 =( NAMED_UNIT ( * ) SI_UNIT ( $, .STERADIAN. ) SOLID_ANGLE_UNIT ( ) );
#49476 = EDGE_CURVE ( 'NONE', #45927, #43947, #35575, .T. ) ;
#49477 = ADVANCED_FACE ( 'NONE', ( #49556 ), #26512, .F. ) ;
#49478 = ORIENTED_EDGE ( 'NONE', *, *, #19699, .T. ) ;
#49479 = CARTESIAN_POINT ( 'NONE',  ( -166.6959734468149463, 0.000000000000000000, 165.0000000000000000 ) ) ;
#49480 = ORIENTED_EDGE ( 'NONE', *, *, #10202, .F. ) ;
#49481 = DIRECTION ( 'NONE',  ( 0.000000000000000000, 0.000000000000000000, 1.000000000000000000 ) ) ;
#49482 = ORIENTED_EDGE ( 'NONE', *, *, #6114, .T. ) ;
#49483 = EDGE_CURVE ( 'NONE', #29419, #5984, #41909, .T. ) ;
#49484 = CARTESIAN_POINT ( 'NONE',  ( -14.99999999999970868, 17.00000000000000000, -60.00000000000000000 ) ) ;
#49485 = CARTESIAN_POINT ( 'NONE',  ( 75.05402655318509630, -1.025126265847089213, -37.43171244307202272 ) ) ;
#49486 = ORIENTED_EDGE ( 'NONE', *, *, #40330, .F. ) ;
#49487 = DIRECTION ( 'NONE',  ( -1.000000000000000000, 0.000000000000000000, 0.000000000000000000 ) ) ;
#49488 = VERTEX_POINT ( 'NONE', #22404 ) ;
#49489 =( BOUNDED_CURVE ( )  B_SPLINE_CURVE ( 3, ( #564, #15182, #23385, #8005 ),
 .UNSPECIFIED., .F., .F. ) 
 B_SPLINE_CURVE_WITH_KNOTS ( ( 4, 4 ),
 ( 4.712388980384693227, 6.283185307179586232 ),
 .UNSPECIFIED. ) 
 CURVE ( )  GEOMETRIC_REPRESENTATION_ITEM ( )  RATIONAL_B_SPLINE_CURVE ( ( 1.000000000000000000, 0.8047378541243658256, 0.8047378541243658256, 1.000000000000000000 ) ) 
 REPRESENTATION_ITEM ( '' )  );
#49490 = LINE ( 'NONE', #48971, #13587 ) ;
#49491 = ORIENTED_EDGE ( 'NONE', *, *, #14042, .F. ) ;
#49492 = CARTESIAN_POINT ( 'NONE',  ( -165.0000000000000284, 16.00000000000000000, 115.0000000000000142 ) ) ;
#49493 = CARTESIAN_POINT ( 'NONE',  ( -164.9459734468149463, -1.025126265847089657, 119.0682875569279560 ) ) ;
#49494 = AXIS2_PLACEMENT_3D ( 'NONE', #41946, #27052, #34257 ) ;
#49495 = CARTESIAN_POINT ( 'NONE',  ( -46.69597344681494633, -1.750000000000009992, 0.8182875569279768335 ) ) ;
#49496 = DIRECTION ( 'NONE',  ( -1.000000000000000000, -0.000000000000000000, -0.000000000000000000 ) ) ;
#49497 = ORIENTED_EDGE ( 'NONE', *, *, #26959, .F. ) ;
#49498 = ORIENTED_EDGE ( 'NONE', *, *, #875, .F. ) ;
#49499 = CARTESIAN_POINT ( 'NONE',  ( 15.00000000000000000, 12.98684210526315930, 19.37312575500900280 ) ) ;
#49500 = VERTEX_POINT ( 'NONE', #7015 ) ;
#49501 = CARTESIAN_POINT ( 'NONE',  ( 7.241383964640743187, 3.469446951953614189E-15, 5.000000000000000000 ) ) ;
#49502 = CARTESIAN_POINT ( 'NONE',  ( 339.9999999999999432, 169.0000000000001705, -344.0000000000002842 ) ) ;
#49503 = EDGE_LOOP ( 'NONE', ( #505, #13913, #12183, #5185, #37598, #6638, #48378, #16470 ) ) ;
#49504 = CARTESIAN_POINT ( 'NONE',  ( -14.99999999999812594, 16.00000000000000000, 90.00000000000000000 ) ) ;
#49505 =( BOUNDED_CURVE ( )  B_SPLINE_CURVE ( 3, ( #21675, #41172, #2678, #49584 ),
 .UNSPECIFIED., .F., .F. ) 
 B_SPLINE_CURVE_WITH_KNOTS ( ( 4, 4 ),
 ( 4.712388980384689674, 6.283185307179586232 ),
 .UNSPECIFIED. ) 
 CURVE ( )  GEOMETRIC_REPRESENTATION_ITEM ( )  RATIONAL_B_SPLINE_CURVE ( ( 1.000000000000000000, 0.8047378541243649375, 0.8047378541243649375, 1.000000000000000000 ) ) 
 REPRESENTATION_ITEM ( '' )  );
#49506 = CARTESIAN_POINT ( 'NONE',  ( 183.0000000000000284, 2.775557561562891351E-14, -99.00000000000014211 ) ) ;
#49507 = ORIENTED_EDGE ( 'NONE', *, *, #40910, .T. ) ;
#49508 = VECTOR ( 'NONE', #7356, 1000.000000000000000 ) ;
#49509 = EDGE_CURVE ( 'NONE', #49806, #13126, #793, .T. ) ;
#49510 = CARTESIAN_POINT ( 'NONE',  ( -1.782521105131510186, 0.3635605703594341209, 9.903764339332088440 ) ) ;
#49511 = CARTESIAN_POINT ( 'NONE',  ( 339.9999999999999432, 181.0000000000002274, -356.0000000000003411 ) ) ;
#49512 = CARTESIAN_POINT ( 'NONE',  ( -86.69597344681494633, 1.750000000000010214, 40.81828755692798438 ) ) ;
#49513 = ORIENTED_EDGE ( 'NONE', *, *, #34064, .F. ) ;
#49514 = DIRECTION ( 'NONE',  ( 0.4436251537532894806, 0.000000000000000000, 0.8962124318248270161 ) ) ;
#49515 = CARTESIAN_POINT ( 'NONE',  ( -11.73320209285699889, 11.96063479729179768, 9.403735324607438884 ) ) ;
#49516 = CARTESIAN_POINT ( 'NONE',  ( -0.4400426740873942810, 2.015233077865125733, 9.886433018048068178 ) ) ;
#49517 = ORIENTED_EDGE ( 'NONE', *, *, #39420, .T. ) ;
#49518 = ORIENTED_EDGE ( 'NONE', *, *, #49663, .F. ) ;
#49519 = CARTESIAN_POINT ( 'NONE',  ( 195.0540265531851105, -1.025126265847089435, -117.4317124430720156 ) ) ;
#49520 = DIRECTION ( 'NONE',  ( 0.000000000000000000, 0.000000000000000000, 1.000000000000000000 ) ) ;
#49521 = CARTESIAN_POINT ( 'NONE',  ( -7.129058724845069861, -15.30620660340479766, 9.178419661560148768 ) ) ;
#49522 = VECTOR ( 'NONE', #25059, 1000.000000000000000 ) ;
#49523 = LINE ( 'NONE', #29325, #35696 ) ;
#49524 = FACE_OUTER_BOUND ( 'NONE', #45545, .T. ) ;
#49525 = AXIS2_PLACEMENT_3D ( 'NONE', #31363, #27252, #42877 ) ;
#49526 = PLANE ( 'NONE',  #24813 ) ;
#49527 = ORIENTED_EDGE ( 'NONE', *, *, #36260, .T. ) ;
#49528 = DIRECTION ( 'NONE',  ( 0.000000000000000000, -0.000000000000000000, -1.000000000000000000 ) ) ;
#49529 = CARTESIAN_POINT ( 'NONE',  ( 356.0000000000000000, -174.9999999999999147, 343.9999999999998295 ) ) ;
#49530 = DIRECTION ( 'NONE',  ( 1.000000000000000000, -3.172065784643302499E-16, -1.942330104924128867E-32 ) ) ;
#49531 = CARTESIAN_POINT ( 'NONE',  ( 0.3862712429686727678, 1.188820645368945605, 10.00000000000000000 ) ) ;
#49532 = ORIENTED_EDGE ( 'NONE', *, *, #3700, .T. ) ;
#49533 = CIRCLE ( 'NONE', #30732, 0.4999999999999997224 ) ;
#49534 = CARTESIAN_POINT ( 'NONE',  ( 113.3040265531850537, 1.749999999999997335, 80.81828755692798438 ) ) ;
#49535 = EDGE_LOOP ( 'NONE', ( #44662, #8917, #11466, #34208, #37927, #17182 ) ) ;
#49536 = EDGE_CURVE ( 'NONE', #19269, #920, #27280, .T. ) ;
#49537 = CARTESIAN_POINT ( 'NONE',  ( 210.0000000000000568, 0.000000000000000000, 160.8182875569279702 ) ) ;
#49538 = CARTESIAN_POINT ( 'NONE',  ( 0.000000000000000000, 181.0000000000000284, 357.9999999999997726 ) ) ;
#49539 = PRODUCT_DEFINITION_FORMATION_WITH_SPECIFIED_SOURCE ( 'ANY', '', #14677, .NOT_KNOWN. ) ;
#49540 = B_SPLINE_CURVE_WITH_KNOTS ( 'NONE', 3,
 ( #4770, #47835, #12722, #678 ),
 .UNSPECIFIED., .F., .F.,
 ( 4, 4 ),
 ( 9.563268421171419053E-18, 0.009782300387714814097 ),
 .UNSPECIFIED. ) ;
#49541 = DIRECTION ( 'NONE',  ( -0.000000000000000000, -1.000000000000000000, -0.000000000000000000 ) ) ;
#49542 = VECTOR ( 'NONE', #47132, 1000.000000000000000 ) ;
#49543 = EDGE_LOOP ( 'NONE', ( #17957, #24827, #11358, #8613 ) ) ;
#49544 = CARTESIAN_POINT ( 'NONE',  ( 151.5540265531850537, 0.000000000000000000, -0.9317124430720247208 ) ) ;
#49545 = ORIENTED_EDGE ( 'NONE', *, *, #38424, .T. ) ;
#49546 = CARTESIAN_POINT ( 'NONE',  ( -45.67084718096785423, 1.750000000000009548, 39.79316129108089228 ) ) ;
#49547 = DIRECTION ( 'NONE',  ( -0.000000000000000000, -1.000000000000000000, 2.537652627714643577E-15 ) ) ;
#49548 = CARTESIAN_POINT ( 'NONE',  ( -4.945973446814917018, 1.025126265847096763, 162.5682875569279986 ) ) ;
#49549 = VERTEX_POINT ( 'NONE', #19055 ) ;
#49550 = ORIENTED_EDGE ( 'NONE', *, *, #47857, .T. ) ;
#49551 = CARTESIAN_POINT ( 'NONE',  ( 84.99999999999997158, 17.00000000000000000, -90.00000000000000000 ) ) ;
#49552 = CARTESIAN_POINT ( 'NONE',  ( -124.9459734468149321, 1.025126265847082108, -37.43171244307203693 ) ) ;
#49553 = VECTOR ( 'NONE', #24941, 1000.000000000000000 ) ;
#49554 = VERTEX_POINT ( 'NONE', #43420 ) ;
#49555 = ORIENTED_EDGE ( 'NONE', *, *, #39324, .T. ) ;
#49556 = FACE_OUTER_BOUND ( 'NONE', #26560, .T. ) ;
#49557 = CARTESIAN_POINT ( 'NONE',  ( 35.05402655318504657, 2.143131898507880377E-16, -77.43171244307198720 ) ) ;
#49558 = LINE ( 'NONE', #45724, #43604 ) ;
#49559 = ORIENTED_EDGE ( 'NONE', *, *, #14179, .T. ) ;
#49560 = CARTESIAN_POINT ( 'NONE',  ( 33.30402655318503946, 0.000000000000000000, 165.0000000000000000 ) ) ;
#49561 = ORIENTED_EDGE ( 'NONE', *, *, #45852, .T. ) ;
#49562 = AXIS2_PLACEMENT_3D ( 'NONE', #42369, #34443, #33439 ) ;
#49563 = DIRECTION ( 'NONE',  ( -1.156482317317870492E-16, 1.000000000000000000, 0.000000000000000000 ) ) ;
#49564 = CARTESIAN_POINT ( 'NONE',  ( -47.72109971266203132, -1.750000000000010214, -120.2068387089191219 ) ) ;
#49565 = VERTEX_POINT ( 'NONE', #15722 ) ;
#49566 = ORIENTED_EDGE ( 'NONE', *, *, #36402, .T. ) ;
#49567 = VECTOR ( 'NONE', #48687, 1000.000000000000000 ) ;
#49568 = VERTEX_POINT ( 'NONE', #19819 ) ;
#49569 = LINE ( 'NONE', #14471, #37434 ) ;
#49570 = DIRECTION ( 'NONE',  ( 0.000000000000000000, -1.000000000000000000, 0.000000000000000000 ) ) ;
#49571 = EDGE_LOOP ( 'NONE', ( #17742, #17184, #1375, #35364 ) ) ;
#49573 = B_SPLINE_CURVE_WITH_KNOTS ( 'NONE', 3,
 ( #32232, #31738, #47326, #12212 ),
 .UNSPECIFIED., .F., .F.,
 ( 4, 4 ),
 ( 0.7491799374948677759, 1.000000000000000000 ),
 .UNSPECIFIED. ) ;
#49572 = CARTESIAN_POINT ( 'NONE',  ( -4.945973446814917018, -1.025126265847096985, -0.9317124430720461481 ) ) ;
#49574 = EDGE_LOOP ( 'NONE', ( #23568, #13999, #28945, #26323, #11281, #20182 ) ) ;
#49575 = VECTOR ( 'NONE', #37920, 1000.000000000000000 ) ;
#49576 = CARTESIAN_POINT ( 'NONE',  ( 33.30402655318503946, 0.000000000000000000, 165.0000000000000000 ) ) ;
#49577 = CARTESIAN_POINT ( 'NONE',  ( 214.9999999999999432, 173.0000000000000000, 252.0000000000000000 ) ) ;
#49578 = VERTEX_POINT ( 'NONE', #7530 ) ;
#49579 = CARTESIAN_POINT ( 'NONE',  ( -48.44597344681495343, 0.000000000000000000, -77.43171244307198720 ) ) ;
#49580 = LINE ( 'NONE', #25783, #9557 ) ;
#49581 = CARTESIAN_POINT ( 'NONE',  ( 183.0000000000000000, -168.9999999999999432, -340.0000000000001705 ) ) ;
#49582 = CARTESIAN_POINT ( 'NONE',  ( -19.99999999999815969, 16.00000000000000000, 65.00000000000000000 ) ) ;
#49583 =( BOUNDED_CURVE ( )  B_SPLINE_CURVE ( 3, ( #11365, #46473, #27782, #8289 ),
 .UNSPECIFIED., .F., .F. ) 
 B_SPLINE_CURVE_WITH_KNOTS ( ( 4, 4 ),
 ( 3.141592653589793116, 4.712388980384689674 ),
 .UNSPECIFIED. ) 
 CURVE ( )  GEOMETRIC_REPRESENTATION_ITEM ( )  RATIONAL_B_SPLINE_CURVE ( ( 1.000000000000000000, 0.8047378541243649375, 0.8047378541243649375, 1.000000000000000000 ) ) 
 REPRESENTATION_ITEM ( '' )  );
#49584 = CARTESIAN_POINT ( 'NONE',  ( -164.9459734468149463, 2.143131898507880377E-16, 79.06828755692797017 ) ) ;
#49585 = EDGE_LOOP ( 'NONE', ( #11827, #208, #46310, #34528 ) ) ;
#49586 = FACE_OUTER_BOUND ( 'NONE', #22955, .T. ) ;
#49587 = PLANE ( 'NONE',  #37170 ) ;
#49588 = FACE_OUTER_BOUND ( 'NONE', #2735, .T. ) ;
#49589 = DIRECTION ( 'NONE',  ( 0.000000000000000000, 0.000000000000000000, -1.000000000000000000 ) ) ;
#49590 = VECTOR ( 'NONE', #1282, 1000.000000000000000 ) ;
#49591 = ADVANCED_FACE ( 'NONE', ( #42656 ), #15468, .T. ) ;
#49592 = CARTESIAN_POINT ( 'NONE',  ( 0.4500758073841586437, 0.7003689023519015233, 9.985686052694765280 ) ) ;
#49593 = CARTESIAN_POINT ( 'NONE',  ( 191.5540265531851105, 0.000000000000000000, -117.4317124430720725 ) ) ;
#49594 = CARTESIAN_POINT ( 'NONE',  ( 152.2789002873379900, -1.750000000000009548, -0.2068387089191121020 ) ) ;
#49595 = EDGE_CURVE ( 'NONE', #13512, #20319, #14967, .T. ) ;
#49596 = DIRECTION ( 'NONE',  ( 0.000000000000000000, 0.000000000000000000, 1.000000000000000000 ) ) ;
#49597 = VECTOR ( 'NONE', #35802, 999.9999999999998863 ) ;
#49598 = PLANE ( 'NONE',  #9112 ) ;
#49599 = EDGE_CURVE ( 'NONE', #26763, #8001, #47241, .T. ) ;
#49600 = ORIENTED_EDGE ( 'NONE', *, *, #12631, .T. ) ;
#49601 = EDGE_CURVE ( 'NONE', #42210, #14899, #19827, .T. ) ;
#49602 = VECTOR ( 'NONE', #32025, 1000.000000000000000 ) ;
#49603 = CARTESIAN_POINT ( 'NONE',  ( -16.02661358026017879, -4.530191650547607196, -9.683996418299976483 ) ) ;
#49604 = CARTESIAN_POINT ( 'NONE',  ( 75.05402655318509630, 2.143131898507873721E-16, 165.0000000000000000 ) ) ;
#49605 = CARTESIAN_POINT ( 'NONE',  ( 130.0000000000021032, 17.00000000000000000, 115.0000000000000142 ) ) ;
#49606 = LINE ( 'NONE', #22706, #38937 ) ;
#49607 = ADVANCED_FACE ( 'NONE', ( #35244 ), #31131, .F. ) ;
#49608 = EDGE_LOOP ( 'NONE', ( #13499, #37809, #40551, #25144, #14796, #41672 ) ) ;
#49609 = ORIENTED_EDGE ( 'NONE', *, *, #7311, .F. ) ;
#49610 = LINE ( 'NONE', #30161, #16900 ) ;
#49611 = AXIS2_PLACEMENT_3D ( 'NONE', #23871, #35438, #7469 ) ;
#49612 = CARTESIAN_POINT ( 'NONE',  ( 341.9999999999999432, -168.9999999999999147, 343.9999999999998295 ) ) ;
#49613 = ORIENTED_EDGE ( 'NONE', *, *, #44298, .T. ) ;
#49614 = CARTESIAN_POINT ( 'NONE',  ( 1.249999999999999778, 0.000000000000000000, 10.00000000000000000 ) ) ;
#49615 = PLANE ( 'NONE',  #19993 ) ;
#49616 = FACE_OUTER_BOUND ( 'NONE', #9420, .T. ) ;
#49617 = ORIENTED_EDGE ( 'NONE', *, *, #808, .T. ) ;
#49618 = VERTEX_POINT ( 'NONE', #31655 ) ;
#49619 = ORIENTED_EDGE ( 'NONE', *, *, #43586, .F. ) ;
#49620 = EDGE_CURVE ( 'NONE', #35947, #11473, #38841, .T. ) ;
#49621 = EDGE_CURVE ( 'NONE', #572, #34164, #8040, .T. ) ;
#49622 = DIRECTION ( 'NONE',  ( -1.000000000000000000, -1.156482317317870492E-16, 0.000000000000000000 ) ) ;
#49623 = CARTESIAN_POINT ( 'NONE',  ( 31.44259251615245887, 38.95901822126168668, -9.367992836599954742 ) ) ;
#49624 = EDGE_CURVE ( 'NONE', #47427, #17436, #42721, .T. ) ;
#49625 = VECTOR ( 'NONE', #29605, 1000.000000000000000 ) ;
#49626 = ORIENTED_EDGE ( 'NONE', *, *, #42556, .F. ) ;
#49627 = EDGE_CURVE ( 'NONE', #36951, #13485, #49583, .T. ) ;
#49628 = DIRECTION ( 'NONE',  ( -1.000000000000000000, -0.000000000000000000, -0.000000000000000000 ) ) ;
#49629 = CIRCLE ( 'NONE', #20199, 4.000000000000003553 ) ;
#49630 = CARTESIAN_POINT ( 'NONE',  ( -15.00000000000000000, 12.98684210526315930, -19.37312575500900280 ) ) ;
#49631 =( NAMED_UNIT ( * ) PLANE_ANGLE_UNIT ( ) SI_UNIT ( $, .RADIAN. ) );
#49632 = ORIENTED_EDGE ( 'NONE', *, *, #6753, .T. ) ;
#49633 = VECTOR ( 'NONE', #35252, 1000.000000000000000 ) ;
#49634 = ORIENTED_EDGE ( 'NONE', *, *, #45840, .T. ) ;
#49635 = DIRECTION ( 'NONE',  ( 0.000000000000000000, -1.000000000000000000, 0.000000000000000000 ) ) ;
#49636 = EDGE_CURVE ( 'NONE', #14002, #18060, #2434, .T. ) ;
#49637 = CARTESIAN_POINT ( 'NONE',  ( 0.000000000000000000, -184.7999999999999545, -340.2000000000001592 ) ) ;
#49638 = EDGE_CURVE ( 'NONE', #33796, #42641, #28656, .T. ) ;
#49639 = CARTESIAN_POINT ( 'NONE',  ( 114.3291528190321173, 1.749999999999996669, -38.15658617722495194 ) ) ;
#49640 = EDGE_LOOP ( 'NONE', ( #17892, #16937, #27463, #49991, #44006, #4195 ) ) ;
#49641 = CARTESIAN_POINT ( 'NONE',  ( 193.3040265531851105, 1.750000000000010214, 40.81828755692798438 ) ) ;
#49642 =( BOUNDED_CURVE ( )  B_SPLINE_CURVE ( 3, ( #22332, #45906, #41839, #49495 ),
 .UNSPECIFIED., .F., .F. ) 
 B_SPLINE_CURVE_WITH_KNOTS ( ( 4, 4 ),
 ( 3.141592653589793116, 4.712388980384689674 ),
 .UNSPECIFIED. ) 
 CURVE ( )  GEOMETRIC_REPRESENTATION_ITEM ( )  RATIONAL_B_SPLINE_CURVE ( ( 1.000000000000000000, 0.8047378541243649375, 0.8047378541243649375, 1.000000000000000000 ) ) 
 REPRESENTATION_ITEM ( '' )  );
#49643 = CARTESIAN_POINT ( 'NONE',  ( -6.695973446814940111, 1.750000000000024203, 120.8182875569279702 ) ) ;
#49644 = CARTESIAN_POINT ( 'NONE',  ( 360.0000000000000568, 183.3431457505076310, 358.3431457505075741 ) ) ;
#49645 = CARTESIAN_POINT ( 'NONE',  ( 2.462075149652696027, -16.57295996686994499, 9.403735324607438884 ) ) ;
#49646 = ORIENTED_EDGE ( 'NONE', *, *, #431, .F. ) ;
#49647 = CARTESIAN_POINT ( 'NONE',  ( 10.28825587112223161, -13.03847615613158517, 3.266473740018926541 ) ) ;
#49648 = LINE ( 'NONE', #22750, #1298 ) ;
#49649 =( BOUNDED_CURVE ( )  B_SPLINE_CURVE ( 3, ( #29148, #21685, #13483, #2199 ),
 .UNSPECIFIED., .F., .F. ) 
 B_SPLINE_CURVE_WITH_KNOTS ( ( 4, 4 ),
 ( 4.712388980384700332, 6.283185307179586232 ),
 .UNSPECIFIED. ) 
 CURVE ( )  GEOMETRIC_REPRESENTATION_ITEM ( )  RATIONAL_B_SPLINE_CURVE ( ( 1.000000000000000000, 0.8047378541243676020, 0.8047378541243676020, 1.000000000000000000 ) ) 
 REPRESENTATION_ITEM ( '' )  );
#49650 = CARTESIAN_POINT ( 'NONE',  ( -44.94597344681493922, 2.143131898507880377E-16, -160.9317124430720582 ) ) ;
#49651 = DIRECTION ( 'NONE',  ( 1.000000000000000000, 0.000000000000000000, 0.000000000000000000 ) ) ;
#49652 = ADVANCED_FACE ( 'NONE', ( #26770 ), #19314, .F. ) ;
#49653 = AXIS2_PLACEMENT_3D ( 'NONE', #9533, #17488, #29039 ) ;
#49654 = DIRECTION ( 'NONE',  ( 2.958228394578793832E-31, 0.000000000000000000, 1.000000000000000000 ) ) ;
#49655 = ADVANCED_FACE ( 'NONE', ( #40345 ), #36512, .F. ) ;
#49656 = EDGE_CURVE ( 'NONE', #9673, #2521, #40099, .T. ) ;
#49657 = PLANE ( 'NONE',  #2770 ) ;
#49658 = ORIENTED_EDGE ( 'NONE', *, *, #44751, .F. ) ;
#49659 = CARTESIAN_POINT ( 'NONE',  ( -6.695973446814940111, 1.750000000000024203, 80.81828755692798438 ) ) ;
#49660 = CARTESIAN_POINT ( 'NONE',  ( -45.42829307628559832, -21.98948915213271960, 8.356839323120299312 ) ) ;
#49661 = B_SPLINE_CURVE_WITH_KNOTS ( 'NONE', 3,
 ( #31850, #39043, #39548, #39800 ),
 .UNSPECIFIED., .F., .F.,
 ( 4, 4 ),
 ( 0.001403500796105012442, 0.001586656765099013966 ),
 .UNSPECIFIED. ) ;
#49662 = LINE ( 'NONE', #33565, #41078 ) ;
#49663 = EDGE_CURVE ( 'NONE', #21262, #7318, #4690, .T. ) ;
#49664 = VERTEX_POINT ( 'NONE', #6378 ) ;
#49665 = LINE ( 'NONE', #15069, #45277 ) ;
#49666 = VECTOR ( 'NONE', #13068, 1000.000000000000000 ) ;
#49667 = VERTEX_POINT ( 'NONE', #32645 ) ;
#49668 = CARTESIAN_POINT ( 'NONE',  ( 356.0000000000000568, 175.0000000000000284, -90.00000000000018474 ) ) ;
#49669 = DIRECTION ( 'NONE',  ( 9.251858538543084240E-16, -0.000000000000000000, 1.000000000000000000 ) ) ;
#49670 = CARTESIAN_POINT ( 'NONE',  ( 349.9999999999999432, -182.9999999999999716, 343.9999999999997726 ) ) ;
#49671 = DIRECTION ( 'NONE',  ( -0.000000000000000000, -1.000000000000000000, -0.000000000000000000 ) ) ;
#49672 = ORIENTED_EDGE ( 'NONE', *, *, #718, .F. ) ;
#49673 = CARTESIAN_POINT ( 'NONE',  ( 35.05402655318504657, -1.025126265847088991, 2.568287556927986159 ) ) ;
#49674 = EDGE_LOOP ( 'NONE', ( #41463, #41755, #47516, #7212 ) ) ;
#49675 = ORIENTED_EDGE ( 'NONE', *, *, #28495, .T. ) ;
#49676 = EDGE_CURVE ( 'NONE', #2527, #41220, #4928, .T. ) ;
#49677 = CARTESIAN_POINT ( 'NONE',  ( -165.3973046169136012, 54.43801056904003133, -17.65743994998275213 ) ) ;
#49678 = ORIENTED_EDGE ( 'NONE', *, *, #2908, .F. ) ;
#49679 = CARTESIAN_POINT ( 'NONE',  ( -168.4459734468149747, 1.025126265847089213, 42.56828755692799149 ) ) ;
#49680 = DIRECTION ( 'NONE',  ( 0.000000000000000000, 5.664403186863042467E-17, 1.000000000000000000 ) ) ;
#49681 = ADVANCED_FACE ( 'NONE', ( #32143 ), #9978, .T. ) ;
#49682 = CARTESIAN_POINT ( 'NONE',  ( 10.50000000000000178, -46.01315789473684248, 5.916985404131810178 ) ) ;
#49683 = DIRECTION ( 'NONE',  ( 0.000000000000000000, 0.000000000000000000, 1.000000000000000000 ) ) ;
#49684 = DIRECTION ( 'NONE',  ( 0.000000000000000000, -1.604368532695312981E-16, -1.000000000000000000 ) ) ;
#49685 = VERTEX_POINT ( 'NONE', #28539 ) ;
#49686 = AXIS2_PLACEMENT_3D ( 'NONE', #49807, #45978, #10860 ) ;
#49687 = CARTESIAN_POINT ( 'NONE',  ( 210.0000000000000568, 0.000000000000000000, 80.81828755692798438 ) ) ;
#49688 = CARTESIAN_POINT ( 'NONE',  ( 73.30402655318508209, 1.750000000000009992, 160.8182875569279702 ) ) ;
#49689 = CARTESIAN_POINT ( 'NONE',  ( -164.9999999999978400, 17.00000000000000000, 95.00000000000000000 ) ) ;
#49690 = EDGE_CURVE ( 'NONE', #7855, #25186, #42983, .T. ) ;
#49691 = ORIENTED_EDGE ( 'NONE', *, *, #46093, .F. ) ;
#49692 = EDGE_CURVE ( 'NONE', #46590, #574, #598, .T. ) ;
#49693 = DIRECTION ( 'NONE',  ( -0.000000000000000000, -0.000000000000000000, -1.000000000000000000 ) ) ;
#49694 = CARTESIAN_POINT ( 'NONE',  ( 0.9602803029231544718, -0.8490247040095941777, 9.976582533991681601 ) ) ;
#49695 = ORIENTED_EDGE ( 'NONE', *, *, #22745, .T. ) ;
#49696 = ORIENTED_EDGE ( 'NONE', *, *, #46790, .F. ) ;
#49697 = ORIENTED_EDGE ( 'NONE', *, *, #27580, .T. ) ;
#49698 = CARTESIAN_POINT ( 'NONE',  ( -1.249999999999999778, 0.000000000000000000, 9.972675548442463622 ) ) ;
#49699 = EDGE_CURVE ( 'NONE', #43553, #44231, #28246, .T. ) ;
#49700 = DIRECTION ( 'NONE',  ( -1.586032892321651989E-16, 3.736034562988530447E-32, -1.000000000000000000 ) ) ;
#49701 = ORIENTED_EDGE ( 'NONE', *, *, #42760, .F. ) ;
#49702 = ADVANCED_FACE ( 'NONE', ( #41533 ), #12376, .T. ) ;
#49703 = CARTESIAN_POINT ( 'NONE',  ( -208.4459734468148611, 1.025126265847089435, 82.56828755692798438 ) ) ;
#49704 = CARTESIAN_POINT ( 'NONE',  ( 0.000000000000000000, -184.7999999999999545, 340.1999999999997044 ) ) ;
#49705 = CARTESIAN_POINT ( 'NONE',  ( -86.69597344681494633, -1.750000000000010658, 120.8182875569279702 ) ) ;
#49706 = DIRECTION ( 'NONE',  ( -1.000000000000000000, -0.000000000000000000, -0.000000000000000000 ) ) ;
#49707 = CARTESIAN_POINT ( 'NONE',  ( -49.75871208702130133, -40.58472229863598102, 5.000000000000000000 ) ) ;
#49708 = AXIS2_PLACEMENT_3D ( 'NONE', #36918, #47375, #9177 ) ;
#49709 = VERTEX_POINT ( 'NONE', #44169 ) ;
#49710 = CARTESIAN_POINT ( 'NONE',  ( 10.28825587112223161, -13.03847615613158517, 3.266473740018926541 ) ) ;
#49711 = CARTESIAN_POINT ( 'NONE',  ( 155.0540265531850537, 2.143131898507880377E-16, 119.0682875569279702 ) ) ;
#49712 = ORIENTED_EDGE ( 'NONE', *, *, #44353, .T. ) ;
#49713 = CARTESIAN_POINT ( 'NONE',  ( 183.0000000000000000, -93.50000000000005684, -115.0000000000001563 ) ) ;
#49714 = CARTESIAN_POINT ( 'NONE',  ( -36.76598589393961447, -7.383243274241610088, -8.192531242611266862 ) ) ;
#49715 = EDGE_CURVE ( 'NONE', #55, #48047, #48652, .T. ) ;
#49716 = CARTESIAN_POINT ( 'NONE',  ( -64.99999999999877787, 16.00000000000000000, 5.000000000000004441 ) ) ;
#49717 = FACE_OUTER_BOUND ( 'NONE', #25119, .T. ) ;
#49718 = ORIENTED_EDGE ( 'NONE', *, *, #27130, .F. ) ;
#49719 = CARTESIAN_POINT ( 'NONE',  ( -1.011271242968688533, 0.7347315653655859258, -3.333333333333333481 ) ) ;
#49720 = CARTESIAN_POINT ( 'NONE',  ( 210.0000000000000568, 0.000000000000000000, 40.81828755692798438 ) ) ;
#49721 = CARTESIAN_POINT ( 'NONE',  ( 16.16402646813543242, -4.033894069732437693, -3.546734833711462365 ) ) ;
#49722 = FACE_OUTER_BOUND ( 'NONE', #30733, .T. ) ;
#49723 = CARTESIAN_POINT ( 'NONE',  ( -46.69597344681494633, 1.750000000000010658, -79.18171244307201562 ) ) ;
#49724 = ORIENTED_EDGE ( 'NONE', *, *, #14715, .T. ) ;
#49725 = CARTESIAN_POINT ( 'NONE',  ( 0.000000000000000000, 0.000000000000000000, 900.0000000000000000 ) ) ;
#49726 = VERTEX_POINT ( 'NONE', #28033 ) ;
#49727 = CARTESIAN_POINT ( 'NONE',  ( 75.05402655318509630, 2.143131898507880377E-16, 165.0000000000000000 ) ) ;
#49728 = ORIENTED_EDGE ( 'NONE', *, *, #15563, .T. ) ;
#49729 = DIRECTION ( 'NONE',  ( 0.000000000000000000, -0.2223603367690619725, -0.9749645535258958384 ) ) ;
#49730 = CARTESIAN_POINT ( 'NONE',  ( 210.0000000000000568, 0.000000000000000000, 122.5682875569279844 ) ) ;
#49731 = ORIENTED_EDGE ( 'NONE', *, *, #44643, .F. ) ;
#49732 = CARTESIAN_POINT ( 'NONE',  ( 168.9999999999999716, -174.9999999999999716, -342.0000000000001137 ) ) ;
#49733 = VERTEX_POINT ( 'NONE', #39858 ) ;
#49734 = CARTESIAN_POINT ( 'NONE',  ( -1.228394325311288560, 1.341866297401936636, 9.903764339332077782 ) ) ;
#49735 = VECTOR ( 'NONE', #33494, 1000.000000000000000 ) ;
#49736 = ORIENTED_EDGE ( 'NONE', *, *, #13313, .F. ) ;
#49737 = FACE_OUTER_BOUND ( 'NONE', #37783, .T. ) ;
#49738 = DIRECTION ( 'NONE',  ( 0.000000000000000000, 0.000000000000000000, 1.000000000000000000 ) ) ;
#49739 = CARTESIAN_POINT ( 'NONE',  ( -12.97493236725075683, 11.05939663307000664, 8.953103998512858652 ) ) ;
#49740 = CARTESIAN_POINT ( 'NONE',  ( 6.408332700304398166, 7.676800896350598258, 0.000000000000000000 ) ) ;
#49741 = CARTESIAN_POINT ( 'NONE',  ( -22.50630130403672524, 35.09254592550309582, -9.387872844313825738 ) ) ;
#49742 = ORIENTED_EDGE ( 'NONE', *, *, #37699, .F. ) ;
#49743 = VERTEX_POINT ( 'NONE', #6132 ) ;
#49744 = CARTESIAN_POINT ( 'NONE',  ( 0.3862712429686810944, 1.188820645368943607, 10.00000000000000000 ) ) ;
#49745 = EDGE_CURVE ( 'NONE', #44556, #22127, #47738, .T. ) ;
#49746 = ORIENTED_EDGE ( 'NONE', *, *, #30941, .T. ) ;
#49747 = ADVANCED_FACE ( 'NONE', ( #2275 ), #16731, .F. ) ;
#49748 = CARTESIAN_POINT ( 'NONE',  ( -42.51732812238059722, -47.49695244670218131, 5.000000000000000000 ) ) ;
#49749 = DIRECTION ( 'NONE',  ( -0.000000000000000000, -0.000000000000000000, -1.000000000000000000 ) ) ;
#49750 = ORIENTED_EDGE ( 'NONE', *, *, #17486, .T. ) ;
#49751 = LINE ( 'NONE', #38021, #24562 ) ;
#49752 = VECTOR ( 'NONE', #46751, 1000.000000000000000 ) ;
#49753 = EDGE_CURVE ( 'NONE', #30152, #38030, #10234, .T. ) ;
#49754 = CARTESIAN_POINT ( 'NONE',  ( 210.0000000000000568, 0.000000000000000000, 160.8182875569279702 ) ) ;
#49755 = ORIENTED_EDGE ( 'NONE', *, *, #12047, .F. ) ;
#49756 = EDGE_CURVE ( 'NONE', #49565, #47768, #44883, .T. ) ;
#49757 = DIRECTION ( 'NONE',  ( 0.000000000000000000, 0.000000000000000000, 1.000000000000000000 ) ) ;
#49758 = CARTESIAN_POINT ( 'NONE',  ( -64.99999999999971578, 17.00000000000000000, -84.99999999999998579 ) ) ;
#49759 = EDGE_CURVE ( 'NONE', #32394, #32969, #20831, .T. ) ;
#49760 = CARTESIAN_POINT ( 'NONE',  ( 75.05402655318508209, 0.000000000000000000, 162.5682875569279702 ) ) ;
#49761 = ORIENTED_EDGE ( 'NONE', *, *, #15768, .F. ) ;
#49762 = CARTESIAN_POINT ( 'NONE',  ( -84.94597344681493212, 1.025126265847089879, 82.56828755692798438 ) ) ;
#49763 = CARTESIAN_POINT ( 'NONE',  ( -25.04522487443065160, 22.77512090857326754, 8.356839323120299312 ) ) ;
#49764 = EDGE_CURVE ( 'NONE', #40720, #21347, #3026, .T. ) ;
#49765 = LINE ( 'NONE', #30840, #41159 ) ;
#49766 = VERTEX_POINT ( 'NONE', #37700 ) ;
#49767 = ORIENTED_EDGE ( 'NONE', *, *, #4065, .T. ) ;
#49768 = CARTESIAN_POINT ( 'NONE',  ( 73.30402655318508209, 1.750000000000010658, -119.1817124430720440 ) ) ;
#49769 = CARTESIAN_POINT ( 'NONE',  ( -44.94597344681497475, 0.000000000000000000, 162.5682875569279702 ) ) ;
#49770 = PLANE ( 'NONE',  #10282 ) ;
#49771 = VECTOR ( 'NONE', #38673, 1000.000000000000000 ) ;
#49772 = CARTESIAN_POINT ( 'NONE',  ( -125.6708471809678542, 1.749999999999996669, -158.1565861772249377 ) ) ;
#49773 = DIRECTION ( 'NONE',  ( 0.000000000000000000, 0.000000000000000000, 1.000000000000000000 ) ) ;
#49774 = LINE ( 'NONE', #14674, #2677 ) ;
#49775 = VERTEX_POINT ( 'NONE', #34105 ) ;
#49776 = CARTESIAN_POINT ( 'NONE',  ( -164.9459734468149463, 1.025126265847089435, 2.568287556927986159 ) ) ;
#49777 = CARTESIAN_POINT ( 'NONE',  ( -88.44597344681497475, 0.000000000000000000, 165.0000000000000000 ) ) ;
#49778 = CARTESIAN_POINT ( 'NONE',  ( -204.9459734468149463, 2.143131898507880377E-16, 165.0000000000000000 ) ) ;
#49779 =( BOUNDED_CURVE ( )  B_SPLINE_CURVE ( 3, ( #7261, #38838, #50309, #15462 ),
 .UNSPECIFIED., .F., .F. ) 
 B_SPLINE_CURVE_WITH_KNOTS ( ( 4, 4 ),
 ( 1.570796326794896558, 3.141592653589793116 ),
 .UNSPECIFIED. ) 
 CURVE ( )  GEOMETRIC_REPRESENTATION_ITEM ( )  RATIONAL_B_SPLINE_CURVE ( ( 1.000000000000000000, 0.8047378541243649375, 0.8047378541243649375, 1.000000000000000000 ) ) 
 REPRESENTATION_ITEM ( '' )  );
#49780 = CARTESIAN_POINT ( 'NONE',  ( -164.9459734468149463, 2.143131898507880377E-16, 2.568287556927978166 ) ) ;
#49781 = VERTEX_POINT ( 'NONE', #49929 ) ;
#49782 = PLANE ( 'NONE',  #5681 ) ;
#49783 = ORIENTED_EDGE ( 'NONE', *, *, #21728, .F. ) ;
#49784 = LINE ( 'NONE', #25744, #44268 ) ;
#49785 =( BOUNDED_CURVE ( )  B_SPLINE_CURVE ( 3, ( #19351, #35037, #46758, #12587 ),
 .UNSPECIFIED., .F., .F. ) 
 B_SPLINE_CURVE_WITH_KNOTS ( ( 4, 4 ),
 ( 1.570796326794896558, 3.141592653589793116 ),
 .UNSPECIFIED. ) 
 CURVE ( )  GEOMETRIC_REPRESENTATION_ITEM ( )  RATIONAL_B_SPLINE_CURVE ( ( 1.000000000000000000, 0.8047378541243649375, 0.8047378541243649375, 1.000000000000000000 ) ) 
 REPRESENTATION_ITEM ( '' )  );
#49786 = CARTESIAN_POINT ( 'NONE',  ( -88.44597344681497475, 0.000000000000000000, -80.93171244307204404 ) ) ;
#49787 = CARTESIAN_POINT ( 'NONE',  ( 16.37555114979290849, -29.24217402453064452, -8.466730184410787174 ) ) ;
#49788 = ORIENTED_EDGE ( 'NONE', *, *, #28725, .F. ) ;
#49789 = ADVANCED_FACE ( 'NONE', ( #10482 ), #10729, .T. ) ;
#49790 = CARTESIAN_POINT ( 'NONE',  ( 85.00000000000152056, 17.00000000000000000, 60.00000000000000000 ) ) ;
#49791 = ORIENTED_EDGE ( 'NONE', *, *, #50287, .T. ) ;
#49792 = CARTESIAN_POINT ( 'NONE',  ( -166.6959734468149463, -1.750000000000009992, 0.8182875569279768335 ) ) ;
#49793 = LINE ( 'NONE', #17796, #10602 ) ;
#49794 = CARTESIAN_POINT ( 'NONE',  ( -127.7210997126620242, -1.749999999999996669, 1.843413822775057609 ) ) ;
#49795 =( BOUNDED_CURVE ( )  B_SPLINE_CURVE ( 3, ( #25718, #17764, #33431, #44923 ),
 .UNSPECIFIED., .F., .F. ) 
 B_SPLINE_CURVE_WITH_KNOTS ( ( 4, 4 ),
 ( 0.000000000000000000, 1.570796326794896780 ),
 .UNSPECIFIED. ) 
 CURVE ( )  GEOMETRIC_REPRESENTATION_ITEM ( )  RATIONAL_B_SPLINE_CURVE ( ( 1.000000000000000000, 0.8047378541243649375, 0.8047378541243649375, 1.000000000000000000 ) ) 
 REPRESENTATION_ITEM ( '' )  );
#49796 = EDGE_LOOP ( 'NONE', ( #45238, #38635, #28489, #3149 ) ) ;
#49797 = VERTEX_POINT ( 'NONE', #3524 ) ;
#49798 = DIRECTION ( 'NONE',  ( 0.000000000000000000, -0.000000000000000000, 1.000000000000000000 ) ) ;
#49799 = CARTESIAN_POINT ( 'NONE',  ( 17.34922095635755568, 33.24536858281893359, 8.914903342594564961 ) ) ;
#49800 = VECTOR ( 'NONE', #40633, 1000.000000000000000 ) ;
#49801 = ORIENTED_EDGE ( 'NONE', *, *, #45375, .T. ) ;
#49802 = EDGE_LOOP ( 'NONE', ( #32697, #12490, #1483, #50372 ) ) ;
#49803 = CARTESIAN_POINT ( 'NONE',  ( 80.00000000000122213, 17.00000000000000000, 30.00000000000000000 ) ) ;
#49804 = PLANE ( 'NONE',  #23471 ) ;
#49805 = DIRECTION ( 'NONE',  ( 0.000000000000000000, 0.000000000000000000, 1.000000000000000000 ) ) ;
#49806 = VERTEX_POINT ( 'NONE', #22026 ) ;
#49807 = CARTESIAN_POINT ( 'NONE',  ( 169.0000000000000000, -174.9999999999999716, -95.00000000000014211 ) ) ;
#49808 = ORIENTED_EDGE ( 'NONE', *, *, #296, .T. ) ;
#49809 = CLOSED_SHELL ( 'NONE', ( #3234, #19972, #40269, #36879, #46165, #3042, #6405, #27408 ) ) ;
#49810 = FACE_OUTER_BOUND ( 'NONE', #40422, .T. ) ;
#49811 = CARTESIAN_POINT ( 'NONE',  ( 71.55402655318505367, 0.000000000000000000, -157.4317124430720014 ) ) ;
#49812 = ORIENTED_EDGE ( 'NONE', *, *, #32434, .T. ) ;
#49813 = VERTEX_POINT ( 'NONE', #11500 ) ;
#49814 = APPLICATION_CONTEXT ( 'automotive_design' ) ;
#49815 = ORIENTED_EDGE ( 'NONE', *, *, #43066, .T. ) ;
#49816 = EDGE_CURVE ( 'NONE', #9207, #1177, #10212, .T. ) ;
#49817 =( LENGTH_UNIT ( ) NAMED_UNIT ( * ) SI_UNIT ( .MILLI., .METRE. ) );
#49818 = CARTESIAN_POINT ( 'NONE',  ( 356.0000000000001137, -166.9999999999999432, 341.9999999999998295 ) ) ;
#49819 = ORIENTED_EDGE ( 'NONE', *, *, #46931, .F. ) ;
#49820 = CARTESIAN_POINT ( 'NONE',  ( -1.024768877994760130, 0.8112356146995477468, 9.945465957785112110 ) ) ;
#49821 = ORIENTED_EDGE ( 'NONE', *, *, #44516, .F. ) ;
#49822 = CARTESIAN_POINT ( 'NONE',  ( -7.721099712662037540, 1.750000000000023315, -160.2068387089191219 ) ) ;
#49823 = ORIENTED_EDGE ( 'NONE', *, *, #48379, .F. ) ;
#49824 = CARTESIAN_POINT ( 'NONE',  ( -35.51846793572368455, 35.99772139009146343, 7.906207997025717304 ) ) ;
#49825 = LINE ( 'NONE', #30137, #25130 ) ;
#49826 = CARTESIAN_POINT ( 'NONE',  ( -33.01266944765060174, 5.813986777101691317, 1.847720168420772691 ) ) ;
#49827 = CARTESIAN_POINT ( 'NONE',  ( 0.7606162131530698201, -1.296876929034913140, 9.953784399990620813 ) ) ;
#49828 = VERTEX_POINT ( 'NONE', #42529 ) ;
#49829 = LINE ( 'NONE', #18078, #29965 ) ;
#49830 = PLANE ( 'NONE',  #2355 ) ;
#49831 = CARTESIAN_POINT ( 'NONE',  ( 50.24128791297869867, -41.04536285977715693, 5.000000000000000000 ) ) ;
#49832 = CIRCLE ( 'NONE', #16317, 4.000000000000003553 ) ;
#49833 = CARTESIAN_POINT ( 'NONE',  ( -16.76006782980216059, 2.050259795448645228, 9.178419661560148768 ) ) ;
#49834 = DIRECTION ( 'NONE',  ( -0.000000000000000000, -0.000000000000000000, -1.000000000000000000 ) ) ;
#49835 = VECTOR ( 'NONE', #7230, 1000.000000000000000 ) ;
#49836 = VECTOR ( 'NONE', #27410, 1000.000000000000000 ) ;
#49837 = DIRECTION ( 'NONE',  ( -1.000000000000000000, 1.331116318405244905E-23, 4.755310728521421461E-16 ) ) ;
#49838 = VECTOR ( 'NONE', #41051, 1000.000000000000114 ) ;
#49839 = CARTESIAN_POINT ( 'NONE',  ( -167.7210997126620384, 1.750000000000009548, 121.8434138227750623 ) ) ;
#49840 = EDGE_CURVE ( 'NONE', #1605, #1551, #2775, .T. ) ;
#49841 = ORIENTED_EDGE ( 'NONE', *, *, #48129, .T. ) ;
#49842 = CARTESIAN_POINT ( 'NONE',  ( 177.5000000000000284, -112.5000000000000000, 0.000000000000000000 ) ) ;
#49843 = CARTESIAN_POINT ( 'NONE',  ( 1.011271242968677653, 0.7347315653656002477, -10.00000000000000000 ) ) ;
#49844 = CARTESIAN_POINT ( 'NONE',  ( -1.011271242968688533, 0.7347315653655859258, 10.00000000000000000 ) ) ;
#49845 = LINE ( 'NONE', #2452, #40443 ) ;
#49846 = DIRECTION ( 'NONE',  ( 3.172065745548403743E-16, 1.000000000000000000, 0.000000000000000000 ) ) ;
#49847 = ORIENTED_EDGE ( 'NONE', *, *, #24579, .T. ) ;
#49848 = PRODUCT ( 'solar panel', 'solar panel', '', ( #32100 ) ) ;
#49849 = EDGE_LOOP ( 'NONE', ( #45766, #44215, #21647, #30141, #50067, #4652 ) ) ;
#49850 = DIRECTION ( 'NONE',  ( 1.000000000000000000, 0.000000000000000000, 0.000000000000000000 ) ) ;
#49851 = CARTESIAN_POINT ( 'NONE',  ( 341.9999999999999432, -171.9999999999999147, -347.0000000000001137 ) ) ;
#49852 = ORIENTED_EDGE ( 'NONE', *, *, #40735, .F. ) ;
#49853 = CARTESIAN_POINT ( 'NONE',  ( -25.04522487443065160, 22.77512090857326754, 8.356839323120299312 ) ) ;
#49854 = DIRECTION ( 'NONE',  ( -1.000000000000000000, 0.000000000000000000, -0.000000000000000000 ) ) ;
#49855 = DIRECTION ( 'NONE',  ( 1.000000000000000000, 0.000000000000000000, 0.000000000000000000 ) ) ;
#49856 = EDGE_LOOP ( 'NONE', ( #2031, #23790, #32731, #11378, #32610, #24443 ) ) ;
#49857 = VERTEX_POINT ( 'NONE', #41777 ) ;
#49858 = VERTEX_POINT ( 'NONE', #6633 ) ;
#49859 = CARTESIAN_POINT ( 'NONE',  ( 80.00000000000186162, 16.00000000000000000, 90.00000000000000000 ) ) ;
#49860 = CARTESIAN_POINT ( 'NONE',  ( 165.0000000000000000, -174.9999999999999716, -99.00000000000014211 ) ) ;
#49861 = AXIS2_PLACEMENT_3D ( 'NONE', #42006, #38430, #26613 ) ;
#49862 = DIRECTION ( 'NONE',  ( -1.000000000000000000, -0.000000000000000000, -0.000000000000000000 ) ) ;
#49863 = ORIENTED_EDGE ( 'NONE', *, *, #44014, .F. ) ;
#49864 = AXIS2_PLACEMENT_3D ( 'NONE', #15007, #23721, #38368 ) ;
#49865 = DIRECTION ( 'NONE',  ( 0.000000000000000000, -1.000000000000000000, 0.000000000000000000 ) ) ;
#49866 = FILL_AREA_STYLE_COLOUR ( '', #41731 ) ;
#49867 = ORIENTED_EDGE ( 'NONE', *, *, #36978, .F. ) ;
#49868 =( BOUNDED_CURVE ( )  B_SPLINE_CURVE ( 3, ( #41587, #45904, #6434, #15405 ),
 .UNSPECIFIED., .F., .F. ) 
 B_SPLINE_CURVE_WITH_KNOTS ( ( 4, 4 ),
 ( 3.141592653589793116, 4.712388980384689674 ),
 .UNSPECIFIED. ) 
 CURVE ( )  GEOMETRIC_REPRESENTATION_ITEM ( )  RATIONAL_B_SPLINE_CURVE ( ( 1.000000000000000000, 0.8047378541243649375, 0.8047378541243649375, 1.000000000000000000 ) ) 
 REPRESENTATION_ITEM ( '' )  );
#49869 = VERTEX_POINT ( 'NONE', #19179 ) ;
#49870 = FACE_OUTER_BOUND ( 'NONE', #31125, .T. ) ;
#49871 = VECTOR ( 'NONE', #14013, 1000.000000000000000 ) ;
#49872 = EDGE_CURVE ( 'NONE', #37204, #16089, #44369, .T. ) ;
#49873 = AXIS2_PLACEMENT_3D ( 'NONE', #23585, #50481, #15631 ) ;
#49874 = DIRECTION ( 'NONE',  ( -1.000000000000000000, 0.000000000000000000, 0.000000000000000000 ) ) ;
#49875 = CARTESIAN_POINT ( 'NONE',  ( 50.00000000000000000, 50.00000000000000000, 800.0000000000000000 ) ) ;
#49876 = B_SPLINE_CURVE_WITH_KNOTS ( 'NONE', 3,
 ( #28437, #17131, #2236, #6081, #13521, #9427 ),
 .UNSPECIFIED., .F., .F.,
 ( 4, 2, 4 ),
 ( 4.906538933386796626E-18, 0.009877169331704831884, 0.01975433866340965683 ),
 .UNSPECIFIED. ) ;
#49877 = EDGE_LOOP ( 'NONE', ( #26078, #11572, #7512, #17152 ) ) ;
#49878 = ORIENTED_EDGE ( 'NONE', *, *, #38474, .T. ) ;
#49879 = PLANE ( 'NONE',  #38921 ) ;
#49880 = VECTOR ( 'NONE', #49547, 1000.000000000000000 ) ;
#49881 = CARTESIAN_POINT ( 'NONE',  ( -0.3618874479330241867, 1.945951947734487320, 9.897807938190496202 ) ) ;
#49882 = DIRECTION ( 'NONE',  ( -0.000000000000000000, 1.000000000000000000, 0.000000000000000000 ) ) ;
#49883 = CARTESIAN_POINT ( 'NONE',  ( 4.204997580903516941, -7.388441598285492518, 225.0000000000000000 ) ) ;
#49884 = ORIENTED_EDGE ( 'NONE', *, *, #36761, .T. ) ;
#49885 = CARTESIAN_POINT ( 'NONE',  ( 210.0000000000000568, 0.000000000000000000, -117.4317124430720298 ) ) ;
#49886 = EDGE_CURVE ( 'NONE', #9479, #34755, #7780, .T. ) ;
#49887 = DIRECTION ( 'NONE',  ( -0.000000000000000000, -0.000000000000000000, -1.000000000000000000 ) ) ;
#49888 = CARTESIAN_POINT ( 'NONE',  ( 183.0000000000000000, -272.4999999999999432, -356.0000000000001705 ) ) ;
#49889 = EDGE_CURVE ( 'NONE', #13738, #30975, #33851, .T. ) ;
#49890 = CARTESIAN_POINT ( 'NONE',  ( -165.6708471809677974, -1.750000000000009548, -160.2068387089191219 ) ) ;
#49891 = EDGE_CURVE ( 'NONE', #17971, #49361, #4084, .T. ) ;
#49892 = CARTESIAN_POINT ( 'NONE',  ( -88.44597344681494633, 1.025126265847089435, -77.43171244307200141 ) ) ;
#49893 = CARTESIAN_POINT ( 'NONE',  ( 35.00000000000216716, 16.00000000000000000, 95.00000000000000000 ) ) ;
#49894 = ORIENTED_EDGE ( 'NONE', *, *, #20811, .F. ) ;
#49895 = CARTESIAN_POINT ( 'NONE',  ( 6.875132362119187768, -50.00000000000000711, 8.356839323120299312 ) ) ;
#49896 = DIRECTION ( 'NONE',  ( 0.000000000000000000, 0.000000000000000000, 1.000000000000000000 ) ) ;
#49897 = ADVANCED_FACE ( 'NONE', ( #26642 ), #37957, .F. ) ;
#49898 = ADVANCED_FACE ( 'NONE', ( #14326 ), #34866, .F. ) ;
#49899 = VECTOR ( 'NONE', #49234, 1000.000000000000000 ) ;
#49900 = CARTESIAN_POINT ( 'NONE',  ( 339.9999999999999432, -165.0000000000001137, -94.00000000000019895 ) ) ;
#49901 = AXIS2_PLACEMENT_3D ( 'NONE', #38686, #15833, #39197 ) ;
#49903 = ORIENTED_EDGE ( 'NONE', *, *, #35057, .T. ) ;
#49902 = EDGE_CURVE ( 'NONE', #49105, #11132, #7145, .T. ) ;
#49904 = SURFACE_STYLE_USAGE ( .BOTH. , #25863 ) ;
#49905 = EDGE_CURVE ( 'NONE', #44210, #14142, #23104, .T. ) ;
#49906 = AXIS2_PLACEMENT_3D ( 'NONE', #16839, #13735, #28629 ) ;
#49907 = CARTESIAN_POINT ( 'NONE',  ( -164.9459734468149463, 1.025126265847089879, 122.5682875569280128 ) ) ;
#49908 = ORIENTED_EDGE ( 'NONE', *, *, #48984, .T. ) ;
#49909 = CARTESIAN_POINT ( 'NONE',  ( -54.99999999999997868, -52.50000000000000711, 5.000000000000000000 ) ) ;
#49910 = CARTESIAN_POINT ( 'NONE',  ( 130.0000000000015064, 16.00000000000000000, 35.00000000000000000 ) ) ;
#49911 = CARTESIAN_POINT ( 'NONE',  ( -126.6959734468149321, 1.749999999999997335, -79.18171244307201562 ) ) ;
#49912 = VECTOR ( 'NONE', #35948, 1000.000000000000000 ) ;
#49913 = DIRECTION ( 'NONE',  ( -1.000000000000000000, 0.000000000000000000, 0.000000000000000000 ) ) ;
#49914 = EDGE_CURVE ( 'NONE', #39676, #16604, #18424, .T. ) ;
#49915 = ORIENTED_EDGE ( 'NONE', *, *, #1231, .T. ) ;
#49916 = CARTESIAN_POINT ( 'NONE',  ( -17.43089236541806031, -28.36237856644526900, 3.199614146704519602 ) ) ;
#49917 = ORIENTED_EDGE ( 'NONE', *, *, #34728, .T. ) ;
#49918 = VERTEX_POINT ( 'NONE', #45842 ) ;
#49919 = CARTESIAN_POINT ( 'NONE',  ( -114.9999999999981526, 16.00000000000000000, 65.00000000000000000 ) ) ;
#49920 = VERTEX_POINT ( 'NONE', #15094 ) ;
#49921 = CARTESIAN_POINT ( 'NONE',  ( -126.6959734468149321, 1.749999999999997113, 40.81828755692798438 ) ) ;
#49922 = CARTESIAN_POINT ( 'NONE',  ( 210.0000000000000568, 0.000000000000000000, 0.8182875569279768335 ) ) ;
#49923 = DIRECTION ( 'NONE',  ( 0.7233555441435720601, -0.6904757466825007794, 0.000000000000000000 ) ) ;
#49924 = DIRECTION ( 'NONE',  ( -1.000000000000000000, 0.000000000000000000, -0.000000000000000000 ) ) ;
#49925 = CARTESIAN_POINT ( 'NONE',  ( -0.4266413953668892756, -1.250184266969579294, 9.943883492372849631 ) ) ;
#49926 = EDGE_CURVE ( 'NONE', #18303, #32019, #30752, .T. ) ;
#49927 = ORIENTED_EDGE ( 'NONE', *, *, #49021, .T. ) ;
#49928 = CARTESIAN_POINT ( 'NONE',  ( -164.9999999999984936, 17.00000000000000000, 35.00000000000000000 ) ) ;
#49929 = CARTESIAN_POINT ( 'NONE',  ( 343.9999999999996589, -165.0000000000001137, -108.0000000000002132 ) ) ;
#49930 = DIRECTION ( 'NONE',  ( 0.6904757466825006684, -0.7233555441435720601, 0.000000000000000000 ) ) ;
#49931 = CARTESIAN_POINT ( 'NONE',  ( -165.0000000000000284, 16.00000000000000000, -114.9999999999999858 ) ) ;
#49932 =( BOUNDED_CURVE ( )  B_SPLINE_CURVE ( 3, ( #20545, #13094, #47696, #5393 ),
 .UNSPECIFIED., .F., .F. ) 
 B_SPLINE_CURVE_WITH_KNOTS ( ( 4, 4 ),
 ( 3.141592653589793116, 4.712388980384689674 ),
 .UNSPECIFIED. ) 
 CURVE ( )  GEOMETRIC_REPRESENTATION_ITEM ( )  RATIONAL_B_SPLINE_CURVE ( ( 1.000000000000000000, 0.8047378541243649375, 0.8047378541243649375, 1.000000000000000000 ) ) 
 REPRESENTATION_ITEM ( '' )  );
#49933 = EDGE_CURVE ( 'NONE', #50534, #25569, #23810, .T. ) ;
#49934 = ORIENTED_EDGE ( 'NONE', *, *, #43537, .T. ) ;
#49935 = EDGE_CURVE ( 'NONE', #5052, #953, #23286, .T. ) ;
#49936 = CARTESIAN_POINT ( 'NONE',  ( -166.6959734468149463, -1.750000000000010214, 40.81828755692798438 ) ) ;
#49937 = DIRECTION ( 'NONE',  ( 0.000000000000000000, 0.000000000000000000, 1.000000000000000000 ) ) ;
#49938 = ORIENTED_EDGE ( 'NONE', *, *, #42565, .F. ) ;
#49939 = VERTEX_POINT ( 'NONE', #468 ) ;
#49940 = ORIENTED_EDGE ( 'NONE', *, *, #45859, .T. ) ;
#49941 = CARTESIAN_POINT ( 'NONE',  ( -1.962558162477761714, 3.366505435501197407, 9.741991644046970933 ) ) ;
#49942 = EDGE_CURVE ( 'NONE', #22449, #48410, #16610, .T. ) ;
#49943 =( BOUNDED_CURVE ( )  B_SPLINE_CURVE ( 3, ( #28334, #46077, #38439, #47787 ),
 .UNSPECIFIED., .F., .F. ) 
 B_SPLINE_CURVE_WITH_KNOTS ( ( 4, 4 ),
 ( 0.000000000000000000, 1.570796326794896558 ),
 .UNSPECIFIED. ) 
 CURVE ( )  GEOMETRIC_REPRESENTATION_ITEM ( )  RATIONAL_B_SPLINE_CURVE ( ( 1.000000000000000000, 0.8047378541243649375, 0.8047378541243649375, 1.000000000000000000 ) ) 
 REPRESENTATION_ITEM ( '' )  );
#49944 = CARTESIAN_POINT ( 'NONE',  ( 8.831420117243668599, 14.12636088103192655, -3.546734833711462365 ) ) ;
#49945 = ORIENTED_EDGE ( 'NONE', *, *, #47745, .F. ) ;
#49946 = AXIS2_PLACEMENT_3D ( 'NONE', #24558, #32017, #700 ) ;
#49947 = ADVANCED_FACE ( 'NONE', ( #36128 ), #43035, .T. ) ;
#49948 = VECTOR ( 'NONE', #50362, 1000.000000000000000 ) ;
#49949 = DIRECTION ( 'NONE',  ( -1.000000000000000000, 0.000000000000000000, 0.000000000000000000 ) ) ;
#49950 = DIRECTION ( 'NONE',  ( 1.000000000000000000, 0.000000000000000000, 0.000000000000000000 ) ) ;
#49951 = FACE_BOUND ( 'NONE', #1292, .T. ) ;
#49952 = VECTOR ( 'NONE', #35982, 1000.000000000000000 ) ;
#49953 = FACE_OUTER_BOUND ( 'NONE', #26869, .T. ) ;
#49954 = PLANE ( 'NONE',  #26347 ) ;
#49955 = LINE ( 'NONE', #19460, #3693 ) ;
#49956 = CARTESIAN_POINT ( 'NONE',  ( 25.63461350838963426, -43.17876197216376966, -8.016098858316199838 ) ) ;
#49957 = AXIS2_PLACEMENT_3D ( 'NONE', #34819, #50395, #3217 ) ;
#49958 = VECTOR ( 'NONE', #50462, 1000.000000000000114 ) ;
#49959 = CARTESIAN_POINT ( 'NONE',  ( -0.7606162131530730397, 1.296876929034918691, 9.953784399990622589 ) ) ;
#49960 = VERTEX_POINT ( 'NONE', #28420 ) ;
#49961 = LINE ( 'NONE', #14864, #3584 ) ;
#49962 = CARTESIAN_POINT ( 'NONE',  ( -125.6708471809678542, 1.749999999999996891, 119.7931612910809065 ) ) ;
#49963 = ADVANCED_FACE ( 'NONE', ( #39473 ), #4558, .T. ) ;
#49964 = CARTESIAN_POINT ( 'NONE',  ( -128.4459734468149463, -1.025126265847081886, -120.9317124430720440 ) ) ;
#49965 = DIRECTION ( 'NONE',  ( -1.000000000000000000, 0.000000000000000000, 0.000000000000000000 ) ) ;
#49966 = EDGE_LOOP ( 'NONE', ( #6491, #41054, #49316, #19308 ) ) ;
#49967 = CARTESIAN_POINT ( 'NONE',  ( -166.6959734468149463, 1.750000000000010658, 120.8182875569279702 ) ) ;
#49968 = DIRECTION ( 'NONE',  ( -0.000000000000000000, -1.000000000000000000, -0.000000000000000000 ) ) ;
#49969 = CARTESIAN_POINT ( 'NONE',  ( -0.3978397141392179814, -0.1292659590675163117, 9.992713367193013951 ) ) ;
#49970 = EDGE_CURVE ( 'NONE', #23499, #35246, #7652, .T. ) ;
#49971 = FILL_AREA_STYLE ('',( #3315 ) ) ;
#49973 = ORIENTED_EDGE ( 'NONE', *, *, #6548, .T. ) ;
#49972 = EDGE_CURVE ( 'NONE', #49549, #28356, #40797, .T. ) ;
#49974 = EDGE_CURVE ( 'NONE', #920, #2364, #46001, .T. ) ;
#49975 = ORIENTED_EDGE ( 'NONE', *, *, #36629, .F. ) ;
#49976 = CARTESIAN_POINT ( 'NONE',  ( -6.875132362119187768, 50.00000000000000711, 8.356839323120299312 ) ) ;
#49977 = ORIENTED_EDGE ( 'NONE', *, *, #40595, .F. ) ;
#49978 = EDGE_CURVE ( 'NONE', #19049, #27459, #5338, .T. ) ;
#49979 = DIRECTION ( 'NONE',  ( -0.000000000000000000, -0.000000000000000000, -1.000000000000000000 ) ) ;
#49980 = LINE ( 'NONE', #49730, #6074 ) ;
#49981 = EDGE_CURVE ( 'NONE', #39875, #32721, #2834, .T. ) ;
#49982 = ORIENTED_EDGE ( 'NONE', *, *, #43065, .F. ) ;
#49983 = SURFACE_STYLE_FILL_AREA ( #15400 ) ;
#49984 = EDGE_LOOP ( 'NONE', ( #10748, #19165, #48209, #38081 ) ) ;
#49985 = ADVANCED_FACE ( 'NONE', ( #4312 ), #27405, .T. ) ;
#49986 = AXIS2_PLACEMENT_3D ( 'NONE', #39713, #40463, #13241 ) ;
#49987 = VECTOR ( 'NONE', #35995, 1000.000000000000000 ) ;
#49988 = ORIENTED_EDGE ( 'NONE', *, *, #24112, .T. ) ;
#49989 = DIRECTION ( 'NONE',  ( 1.654361225106055350E-24, 1.654361225106055350E-24, -1.000000000000000000 ) ) ;
#49990 = DIRECTION ( 'NONE',  ( -0.000000000000000000, -0.000000000000000000, -1.000000000000000000 ) ) ;
#49991 = ORIENTED_EDGE ( 'NONE', *, *, #46296, .F. ) ;
#49992 = CARTESIAN_POINT ( 'NONE',  ( -164.9999999999978400, 17.00000000000000000, 95.00000000000000000 ) ) ;
#49993 = CARTESIAN_POINT ( 'NONE',  ( 111.5540265531850679, 0.000000000000000000, 165.0000000000000000 ) ) ;
#49994 = CYLINDRICAL_SURFACE ( 'NONE', #35589, 1.750000000000001554 ) ;
#49995 = ORIENTED_EDGE ( 'NONE', *, *, #48711, .F. ) ;
#49996 = VECTOR ( 'NONE', #33632, 1000.000000000000000 ) ;
#49997 = ORIENTED_EDGE ( 'NONE', *, *, #9629, .T. ) ;
#49998 = CARTESIAN_POINT ( 'NONE',  ( -49.46074318306826001, 9.578883844007169301, 8.807470649214879543 ) ) ;
#49999 = ORIENTED_EDGE ( 'NONE', *, *, #25600, .T. ) ;
#50000 = EDGE_CURVE ( 'NONE', #48420, #3658, #35381, .T. ) ;
#50001 = CARTESIAN_POINT ( 'NONE',  ( 35.00000000000216716, 16.00000000000000000, 95.00000000000000000 ) ) ;
#50002 = DIRECTION ( 'NONE',  ( 1.000000000000000000, -1.331116318405244905E-23, -4.755310728521421461E-16 ) ) ;
#50003 = ORIENTED_EDGE ( 'NONE', *, *, #42409, .F. ) ;
#50004 = DIRECTION ( 'NONE',  ( 0.000000000000000000, 5.664403186863042467E-17, 1.000000000000000000 ) ) ;
#50005 = CARTESIAN_POINT ( 'NONE',  ( 130.0000000000005684, 17.00000000000000000, -54.99999999999999289 ) ) ;
#50006 = ORIENTED_EDGE ( 'NONE', *, *, #43904, .T. ) ;
#50007 = FACE_OUTER_BOUND ( 'NONE', #39019, .T. ) ;
#50008 = CARTESIAN_POINT ( 'NONE',  ( -128.4459734468149463, -1.025126265847082108, -77.43171244307201562 ) ) ;
#50009 = CARTESIAN_POINT ( 'NONE',  ( 181.0000000000000000, -77.49999999999995737, -115.0000000000001563 ) ) ;
#50010 = CARTESIAN_POINT ( 'NONE',  ( -54.99999999999997868, 52.49999999999999289, -5.000000000000000000 ) ) ;
#50011 = ORIENTED_EDGE ( 'NONE', *, *, #16121, .F. ) ;
#50012 = CARTESIAN_POINT ( 'NONE',  ( -14.48769039275601145, -30.44468701195584970, 8.807470649214879543 ) ) ;
#50013 = DIRECTION ( 'NONE',  ( -0.000000000000000000, -1.000000000000000000, -0.000000000000000000 ) ) ;
#50014 = EDGE_CURVE ( 'NONE', #12862, #39919, #47104, .T. ) ;
#50015 = CARTESIAN_POINT ( 'NONE',  ( -0.4152287376637092131, 2.070986276654349201, 9.884520316594379352 ) ) ;
#50016 = ORIENTED_EDGE ( 'NONE', *, *, #45237, .F. ) ;
#50017 = ORIENTED_EDGE ( 'NONE', *, *, #24678, .T. ) ;
#50018 = CARTESIAN_POINT ( 'NONE',  ( 168.9999999999999716, -77.49999999999997158, -340.0000000000001137 ) ) ;
#50019 = CARTESIAN_POINT ( 'NONE',  ( 168.9999999999999716, -174.9999999999999716, -356.0000000000001705 ) ) ;
#50020 = CARTESIAN_POINT ( 'NONE',  ( -168.4459734468149463, 0.000000000000000000, -157.4317124430720582 ) ) ;
#50021 = CARTESIAN_POINT ( 'NONE',  ( 155.0540265531850537, 2.143131898507880377E-16, -120.9317124430720156 ) ) ;
#50022 = CARTESIAN_POINT ( 'NONE',  ( 0.000000000000000000, 17.00000000000000000, 0.000000000000000000 ) ) ;
#50023 = FACE_OUTER_BOUND ( 'NONE', #31901, .T. ) ;
#50024 = ORIENTED_EDGE ( 'NONE', *, *, #25353, .F. ) ;
#50025 = CARTESIAN_POINT ( 'NONE',  ( -115.0000000000000284, 17.00000000000000000, -90.00000000000000000 ) ) ;
#50026 = VECTOR ( 'NONE', #15728, 1000.000000000000000 ) ;
#50028 = VECTOR ( 'NONE', #15066, 1000.000000000000000 ) ;
#50027 = CARTESIAN_POINT ( 'NONE',  ( -119.9999999999978400, 17.00000000000000000, 115.0000000000000142 ) ) ;
#50029 = DIRECTION ( 'NONE',  ( 0.000000000000000000, 0.4027858274925601445, 0.9152942571496521795 ) ) ;
#50030 = ADVANCED_FACE ( 'NONE', ( #27659 ), #8419, .F. ) ;
#50031 =( NAMED_UNIT ( * ) SI_UNIT ( $, .STERADIAN. ) SOLID_ANGLE_UNIT ( ) );
#50032 = ADVANCED_FACE ( 'NONE', ( #19944 ), #39724, .T. ) ;
#50033 = VERTEX_POINT ( 'NONE', #43798 ) ;
#50034 = CARTESIAN_POINT ( 'NONE',  ( 12.78770032058947237, 31.68259716188277864, 7.455576670931136185 ) ) ;
#50035 = ORIENTED_EDGE ( 'NONE', *, *, #47467, .T. ) ;
#50036 = CARTESIAN_POINT ( 'NONE',  ( 0.000000000000000000, 28.48684210526315752, -5.000000000000000000 ) ) ;
#50037 = LINE ( 'NONE', #41638, #26555 ) ;
#50038 = EDGE_CURVE ( 'NONE', #38466, #17310, #9159, .T. ) ;
#50039 = DIRECTION ( 'NONE',  ( 1.000000000000000000, 0.000000000000000000, 0.000000000000000000 ) ) ;
#50040 = VERTEX_POINT ( 'NONE', #8909 ) ;
#50041 = EDGE_CURVE ( 'NONE', #17812, #6007, #35770, .T. ) ;
#50042 = EDGE_CURVE ( 'NONE', #36777, #8111, #44073, .T. ) ;
#50043 = DIRECTION ( 'NONE',  ( -1.000000000000000000, -0.000000000000000000, -0.000000000000000000 ) ) ;
#50044 = CARTESIAN_POINT ( 'NONE',  ( -124.9459734468149605, 0.000000000000000000, 162.5682875569279702 ) ) ;
#50045 = ORIENTED_EDGE ( 'NONE', *, *, #32504, .T. ) ;
#50046 = CARTESIAN_POINT ( 'NONE',  ( -0.3862712429686977478, 1.188820645368937390, -3.333333333333333481 ) ) ;
#50047 = CARTESIAN_POINT ( 'NONE',  ( -65.00000000000002842, 17.00000000000000000, -90.00000000000000000 ) ) ;
#50048 = DIRECTION ( 'NONE',  ( 1.000000000000000000, 0.000000000000000000, 0.000000000000000000 ) ) ;
#50049 = AXIS2_PLACEMENT_3D ( 'NONE', #22818, #38498, #22311 ) ;
#50050 = EDGE_CURVE ( 'NONE', #32019, #28645, #37399, .T. ) ;
#50051 = EDGE_LOOP ( 'NONE', ( #47984, #28977, #2366, #34817, #580, #35858 ) ) ;
#50052 = ORIENTED_EDGE ( 'NONE', *, *, #49404, .T. ) ;
#50053 = CARTESIAN_POINT ( 'NONE',  ( 168.9999999999999716, -79.49999999999997158, -340.0000000000001137 ) ) ;
#50054 = CARTESIAN_POINT ( 'NONE',  ( 16.71930270649943395, 33.57409379679891259, 8.506357886886741326 ) ) ;
#50055 = ORIENTED_EDGE ( 'NONE', *, *, #29937, .T. ) ;
#50056 = EDGE_LOOP ( 'NONE', ( #43330, #50446, #23865, #13378 ) ) ;
#50057 = DIRECTION ( 'NONE',  ( -0.000000000000000000, -0.000000000000000000, -1.000000000000000000 ) ) ;
#50058 = CARTESIAN_POINT ( 'NONE',  ( 15.00000000000000000, 12.98684210526315930, -19.37312575500900280 ) ) ;
#50059 = CARTESIAN_POINT ( 'NONE',  ( -225.0000000000000568, -175.0000000000000000, 500.0000000000000000 ) ) ;
#50060 = EDGE_LOOP ( 'NONE', ( #26695, #29458, #46470, #17046 ) ) ;
#50061 = DIRECTION ( 'NONE',  ( 0.000000000000000000, -1.580451535867971417E-48, 1.000000000000000000 ) ) ;
#50062 = ORIENTED_EDGE ( 'NONE', *, *, #18779, .T. ) ;
#50063 = CARTESIAN_POINT ( 'NONE',  ( 164.9999999999999716, 16.00000000000000000, -30.00000000000000000 ) ) ;
#50064 = CIRCLE ( 'NONE', #2570, 1.750000000000001554 ) ;
#50065 = CARTESIAN_POINT ( 'NONE',  ( -127.7210997126620242, -1.749999999999996669, -40.20683870891911482 ) ) ;
#50066 = CARTESIAN_POINT ( 'NONE',  ( -0.6440276692615888310, -16.64212148744554298, -9.683996418299976483 ) ) ;
#50067 = ORIENTED_EDGE ( 'NONE', *, *, #4360, .F. ) ;
#50068 = ORIENTED_EDGE ( 'NONE', *, *, #281, .T. ) ;
#50069 = EDGE_LOOP ( 'NONE', ( #15349, #36161, #9116, #22792 ) ) ;
#50070 = CARTESIAN_POINT ( 'NONE',  ( -44.94002984196466599, -9.722063056713757589, -8.016098858316205167 ) ) ;
#50071 = CARTESIAN_POINT ( 'NONE',  ( -210.0000000000000568, 2.143131898507876926E-16, 119.0682875569279560 ) ) ;
#50072 = ORIENTED_EDGE ( 'NONE', *, *, #6928, .F. ) ;
#50073 = DIRECTION ( 'NONE',  ( 1.000000000000000000, 0.000000000000000000, 0.000000000000000000 ) ) ;
#50074 = ORIENTED_EDGE ( 'NONE', *, *, #11821, .F. ) ;
#50075 = ADVANCED_FACE ( 'NONE', ( #21711 ), #25571, .T. ) ;
#50076 = CARTESIAN_POINT ( 'NONE',  ( -164.9459734468149463, 1.025126265847089657, 42.56828755692799149 ) ) ;
#50077 = ORIENTED_EDGE ( 'NONE', *, *, #38467, .T. ) ;
#50078 = FACE_OUTER_BOUND ( 'NONE', #8736, .T. ) ;
#50079 =( BOUNDED_CURVE ( )  B_SPLINE_CURVE ( 3, ( #2264, #49171, #6366, #26378 ),
 .UNSPECIFIED., .F., .F. ) 
 B_SPLINE_CURVE_WITH_KNOTS ( ( 4, 4 ),
 ( 1.346561575685801593, 1.570796326794899667 ),
 .UNSPECIFIED. ) 
 CURVE ( )  GEOMETRIC_REPRESENTATION_ITEM ( )  RATIONAL_B_SPLINE_CURVE ( ( 1.000000000000000000, 0.9958142854328206894, 0.9958142854328206894, 1.000000000000000000 ) ) 
 REPRESENTATION_ITEM ( '' )  );
#50080 = FACE_OUTER_BOUND ( 'NONE', #31611, .T. ) ;
#50081 = CARTESIAN_POINT ( 'NONE',  ( 75.05402655318509630, 2.143131898507880377E-16, -117.4317124430720156 ) ) ;
#50082 = CARTESIAN_POINT ( 'NONE',  ( 181.0000000000000000, -97.49999999999997158, -115.0000000000001563 ) ) ;
#50083 = DIRECTION ( 'NONE',  ( -1.000000000000000000, -0.000000000000000000, -0.000000000000000000 ) ) ;
#50084 = ORIENTED_EDGE ( 'NONE', *, *, #28681, .T. ) ;
#50085 = LINE ( 'NONE', #16021, #33758 ) ;
#50086 =( BOUNDED_CURVE ( )  B_SPLINE_CURVE ( 3, ( #41878, #13905, #22372, #41379 ),
 .UNSPECIFIED., .F., .F. ) 
 B_SPLINE_CURVE_WITH_KNOTS ( ( 4, 4 ),
 ( 4.712388980384689674, 6.283185307179586232 ),
 .UNSPECIFIED. ) 
 CURVE ( )  GEOMETRIC_REPRESENTATION_ITEM ( )  RATIONAL_B_SPLINE_CURVE ( ( 1.000000000000000000, 0.8047378541243649375, 0.8047378541243649375, 1.000000000000000000 ) ) 
 REPRESENTATION_ITEM ( '' )  );
#50087 = VECTOR ( 'NONE', #46935, 1000.000000000000000 ) ;
#50088 = CARTESIAN_POINT ( 'NONE',  ( 33.30402655318503946, 1.750000000000009992, -159.1817124430720298 ) ) ;
#50089 = CARTESIAN_POINT ( 'NONE',  ( 35.00000000000061107, 17.00000000000000000, -30.00000000000000000 ) ) ;
#50090 = CARTESIAN_POINT ( 'NONE',  ( -47.23269937569316568, 16.43609759007082616, -2.408242355805840784 ) ) ;
#50091 = EDGE_CURVE ( 'NONE', #39770, #15922, #13248, .T. ) ;
#50092 = CARTESIAN_POINT ( 'NONE',  ( -33.86622497129646092, 3.037805405905158462, 7.906207997025717304 ) ) ;
#50093 = ADVANCED_FACE ( 'NONE', ( #1478 ), #5218, .T. ) ;
#50094 = AXIS2_PLACEMENT_3D ( 'NONE', #41435, #25533, #46004 ) ;
#50095 = CARTESIAN_POINT ( 'NONE',  ( -0.1287570809895632329, 0.3962735484563137400, 10.00000000000000000 ) ) ;
#50096 = CARTESIAN_POINT ( 'NONE',  ( 0.000000000000000000, 28.48684210526315752, 0.000000000000000000 ) ) ;
#50097 =( BOUNDED_CURVE ( )  B_SPLINE_CURVE ( 3, ( #2232, #17869, #45800, #45299 ),
 .UNSPECIFIED., .F., .F. ) 
 B_SPLINE_CURVE_WITH_KNOTS ( ( 4, 4 ),
 ( 0.000000000000000000, 1.570796326794896558 ),
 .UNSPECIFIED. ) 
 CURVE ( )  GEOMETRIC_REPRESENTATION_ITEM ( )  RATIONAL_B_SPLINE_CURVE ( ( 1.000000000000000000, 0.8047378541243649375, 0.8047378541243649375, 1.000000000000000000 ) ) 
 REPRESENTATION_ITEM ( '' )  );
#50098 = CARTESIAN_POINT ( 'NONE',  ( 1.337801958641917199, 1.088266084286984015, 9.928159647716135794 ) ) ;
#50099 = B_SPLINE_CURVE_WITH_KNOTS ( 'NONE', 3,
 ( #26744, #14939, #46195, #42121 ),
 .UNSPECIFIED., .F., .F.,
 ( 4, 4 ),
 ( 0.0002936521407522628044, 0.0006663369986142421994 ),
 .UNSPECIFIED. ) ;
#50100 = ADVANCED_FACE ( 'NONE', ( #36387 ), #44287, .T. ) ;
#50101 = EDGE_CURVE ( 'NONE', #8304, #26571, #18543, .T. ) ;
#50102 = EDGE_LOOP ( 'NONE', ( #33475, #50613, #38914, #22835 ) ) ;
#50103 = CARTESIAN_POINT ( 'NONE',  ( 1.011271242968677653, 0.7347315653656002477, 10.00000000000000000 ) ) ;
#50104 = CARTESIAN_POINT ( 'NONE',  ( -7.129058724845069861, -15.30620660340479766, 9.178419661560148768 ) ) ;
#50105 = EDGE_CURVE ( 'NONE', #42389, #6937, #34847, .T. ) ;
#50106 = AXIS2_PLACEMENT_3D ( 'NONE', #49178, #14830, #45344 ) ;
#50107 = VERTEX_POINT ( 'NONE', #17112 ) ;
#50108 = B_SPLINE_CURVE_WITH_KNOTS ( 'NONE', 3,
 ( #11846, #27495, #9496, #17210 ),
 .UNSPECIFIED., .F., .F.,
 ( 4, 4 ),
 ( 0.9811748202683399089, 0.9878904167554126703 ),
 .UNSPECIFIED. ) ;
#50109 = ORIENTED_EDGE ( 'NONE', *, *, #32807, .T. ) ;
#50110 = CARTESIAN_POINT ( 'NONE',  ( -2.462075149652696027, 16.57295996686994499, 9.403735324607438884 ) ) ;
#50111 = CARTESIAN_POINT ( 'NONE',  ( 73.30402655318508209, 0.000000000000000000, 165.0000000000000000 ) ) ;
#50112 = VERTEX_POINT ( 'NONE', #33029 ) ;
#50113 = ORIENTED_EDGE ( 'NONE', *, *, #9952, .F. ) ;
#50114 = FACE_OUTER_BOUND ( 'NONE', #41590, .T. ) ;
#50115 = DIRECTION ( 'NONE',  ( 1.000000000000000000, 0.000000000000000000, 0.000000000000000000 ) ) ;
#50116 = CARTESIAN_POINT ( 'NONE',  ( 194.3291528190321742, -1.750000000000009548, -38.15658617722494483 ) ) ;
#50117 = VECTOR ( 'NONE', #20985, 1000.000000000000114 ) ;
#50118 = VERTEX_POINT ( 'NONE', #40971 ) ;
#50119 = ORIENTED_EDGE ( 'NONE', *, *, #26616, .T. ) ;
#50120 = VECTOR ( 'NONE', #47514, 1000.000000000000000 ) ;
#50121 = ORIENTED_EDGE ( 'NONE', *, *, #36593, .F. ) ;
#50122 = DIRECTION ( 'NONE',  ( -1.000000000000000000, -0.000000000000000000, -0.000000000000000000 ) ) ;
#50123 = DIRECTION ( 'NONE',  ( -1.000000000000000000, -0.000000000000000000, -0.000000000000000000 ) ) ;
#50124 = LINE ( 'NONE', #26836, #30847 ) ;
#50125 = ORIENTED_EDGE ( 'NONE', *, *, #5488, .F. ) ;
#50126 = CARTESIAN_POINT ( 'NONE',  ( -46.76852358249001895, 17.86468378716740801, -9.367992836599951190 ) ) ;
#50127 = CIRCLE ( 'NONE', #1847, 4.000000000000003553 ) ;
#50128 = CARTESIAN_POINT ( 'NONE',  ( 73.30402655318508209, 1.750000000000010214, -39.18171244307202983 ) ) ;
#50129 = LINE ( 'NONE', #34046, #38497 ) ;
#50130 = VERTEX_POINT ( 'NONE', #32775 ) ;
#50131 = ORIENTED_EDGE ( 'NONE', *, *, #10006, .F. ) ;
#50132 = CARTESIAN_POINT ( 'NONE',  ( 113.3040265531850537, 1.749999999999996891, 160.8182875569279702 ) ) ;
#50133 = DIRECTION ( 'NONE',  ( 0.000000000000000000, 0.000000000000000000, 1.000000000000000000 ) ) ;
#50134 = ORIENTED_EDGE ( 'NONE', *, *, #2395, .F. ) ;
#50135 = EDGE_LOOP ( 'NONE', ( #35940, #3590, #33916, #26149, #35836, #7587, #1238, #41105, #19597, #48919, #44143, #16463 ) ) ;
#50136 = B_SPLINE_CURVE_WITH_KNOTS ( 'NONE', 3,
 ( #48659, #25873, #13300, #5354 ),
 .UNSPECIFIED., .F., .F.,
 ( 4, 4 ),
 ( 0.01005345353272278641, 0.01006177981554799705 ),
 .UNSPECIFIED. ) ;
#50137 = ADVANCED_FACE ( 'NONE', ( #40724 ), #5560, .T. ) ;
#50138 = DIRECTION ( 'NONE',  ( 1.000000000000000000, 0.000000000000000000, 0.000000000000000000 ) ) ;
#50139 = CARTESIAN_POINT ( 'NONE',  ( 210.0000000000000568, 0.000000000000000000, -79.18171244307201562 ) ) ;
#50140 = FACE_OUTER_BOUND ( 'NONE', #14667, .T. ) ;
#50141 = CARTESIAN_POINT ( 'NONE',  ( 35.05402655318504657, -1.025126265847089213, -37.43171244307202272 ) ) ;
#50142 = CARTESIAN_POINT ( 'NONE',  ( 34.99999999999997868, 17.00000000000000000, -114.9999999999999858 ) ) ;
#50143 = ORIENTED_EDGE ( 'NONE', *, *, #12710, .T. ) ;
#50144 = CARTESIAN_POINT ( 'NONE',  ( 0.000000000000000000, 17.00000000000000000, 0.000000000000000000 ) ) ;
#50145 = CARTESIAN_POINT ( 'NONE',  ( -10.49999999999999467, -46.12433806312137108, 6.404467680894761372 ) ) ;
#50146 = CIRCLE ( 'NONE', #38756, 4.000000000000003553 ) ;
#50147 = CARTESIAN_POINT ( 'NONE',  ( -1.780432407520014415, -1.041450996408466612, 9.894754715216725671 ) ) ;
#50148 = FACE_OUTER_BOUND ( 'NONE', #47813, .T. ) ;
#50149 = DIRECTION ( 'NONE',  ( -0.000000000000000000, -0.000000000000000000, -1.000000000000000000 ) ) ;
#50150 = CARTESIAN_POINT ( 'NONE',  ( 169.0000000000000000, -9.999999999999953815, -113.0000000000001563 ) ) ;
#50151 = ORIENTED_EDGE ( 'NONE', *, *, #11722, .T. ) ;
#50152 = DIRECTION ( 'NONE',  ( 0.000000000000000000, 0.000000000000000000, 1.000000000000000000 ) ) ;
#50153 = TOROIDAL_SURFACE ( 'NONE', #42838, 4.250000000000000000, 0.5000000000000000000 ) ;
#50154 = DIRECTION ( 'NONE',  ( -1.156482317317871478E-16, -1.000000000000000000, 0.000000000000000000 ) ) ;
#50155 = ORIENTED_EDGE ( 'NONE', *, *, #3633, .F. ) ;
#50156 = DIRECTION ( 'NONE',  ( -0.000000000000000000, -0.000000000000000000, 1.000000000000000000 ) ) ;
#50157 = CIRCLE ( 'NONE', #17446, 4.000000000000003553 ) ;
#50158 = DIRECTION ( 'NONE',  ( 0.000000000000000000, 0.000000000000000000, 1.000000000000000000 ) ) ;
#50159 = VERTEX_POINT ( 'NONE', #29176 ) ;
#50160 = CARTESIAN_POINT ( 'NONE',  ( 168.9999999999999716, -79.49999999999995737, -115.0000000000001563 ) ) ;
#50161 = DIRECTION ( 'NONE',  ( -1.000000000000000000, 0.000000000000000000, -2.958228394578794270E-31 ) ) ;
#50162 = EDGE_CURVE ( 'NONE', #15972, #30725, #5815, .T. ) ;
#50163 = CARTESIAN_POINT ( 'NONE',  ( 6.619412807845094449, -7.495556955913033725, 9.646707543097347681 ) ) ;
#50164 = CARTESIAN_POINT ( 'NONE',  ( -0.2459519479914147599, -1.553112592393893099, 9.927288994922820464 ) ) ;
#50165 = EDGE_LOOP ( 'NONE', ( #48438, #10471, #7459 ) ) ;
#50166 =( NAMED_UNIT ( * ) PLANE_ANGLE_UNIT ( ) SI_UNIT ( $, .RADIAN. ) );
#50167 = B_SPLINE_SURFACE_WITH_KNOTS ( 'NONE', 3, 3, ( 
 ( #22123, #13900, #29567, #45185 ),
 ( #41873, #6230, #49521, #21881 ),
 ( #26228, #18006, #33685, #45437 ),
 ( #6718, #22366, #14154, #29826 ) ),
 .UNSPECIFIED., .F., .F., .F.,
 ( 4, 4 ),
 ( 4, 4 ),
 ( 0.000000000000000000, 1.000000000000000000 ),
 ( 0.000000000000000000, 1.000000000000000000 ),
 .UNSPECIFIED. ) ;
#50168 = EDGE_LOOP ( 'NONE', ( #1191, #20095, #13392, #42331 ) ) ;
#50169 = ORIENTED_EDGE ( 'NONE', *, *, #3410, .F. ) ;
#50170 = DIRECTION ( 'NONE',  ( 0.000000000000000000, 0.000000000000000000, 1.000000000000000000 ) ) ;
#50171 = EDGE_LOOP ( 'NONE', ( #23157, #48905, #22466, #22050 ) ) ;
#50172 = CARTESIAN_POINT ( 'NONE',  ( -22.69295089195507131, -45.31600496604688999, 7.455576670931136185 ) ) ;
#50173 = CARTESIAN_POINT ( 'NONE',  ( 358.3431457505075741, -185.0000000000001421, -360.0000000000003411 ) ) ;
#50174 =( BOUNDED_CURVE ( )  B_SPLINE_CURVE ( 3, ( #7363, #42001, #10444, #10692 ),
 .UNSPECIFIED., .F., .F. ) 
 B_SPLINE_CURVE_WITH_KNOTS ( ( 4, 4 ),
 ( 3.141592653589793116, 4.712388980384689674 ),
 .UNSPECIFIED. ) 
 CURVE ( )  GEOMETRIC_REPRESENTATION_ITEM ( )  RATIONAL_B_SPLINE_CURVE ( ( 1.000000000000000000, 0.8047378541243649375, 0.8047378541243649375, 1.000000000000000000 ) ) 
 REPRESENTATION_ITEM ( '' )  );
#50175 = CARTESIAN_POINT ( 'NONE',  ( 0.4426377647354858835, 1.666766018367784596, 9.928159647716132241 ) ) ;
#50176 = CARTESIAN_POINT ( 'NONE',  ( 75.05402655318509630, 2.143131898507880377E-16, 79.06828755692797017 ) ) ;
#50177 = ORIENTED_EDGE ( 'NONE', *, *, #11534, .T. ) ;
#50178 = ADVANCED_FACE ( 'NONE', ( #10670 ), #6825, .T. ) ;
#50179 = DIRECTION ( 'NONE',  ( -1.586032880504786307E-16, 1.654361225106055350E-24, -1.000000000000000000 ) ) ;
#50180 = PLANE ( 'NONE',  #25054 ) ;
#50181 = CARTESIAN_POINT ( 'NONE',  ( 113.3040265531850537, 1.749999999999996891, 160.8182875569279702 ) ) ;
#50182 = EDGE_LOOP ( 'NONE', ( #9458, #34103, #47153, #50188, #36632, #10817 ) ) ;
#50183 = DIRECTION ( 'NONE',  ( 0.000000000000000000, -0.000000000000000000, -1.000000000000000000 ) ) ;
#50184 = CARTESIAN_POINT ( 'NONE',  ( -3.451199890880296994, 1.973209715054570212, 3.247138655587490152 ) ) ;
#50185 = AXIS2_PLACEMENT_3D ( 'NONE', #47089, #4292, #19929 ) ;
#50186 = VERTEX_POINT ( 'NONE', #26332 ) ;
#50187 = ORIENTED_EDGE ( 'NONE', *, *, #24379, .T. ) ;
#50188 = ORIENTED_EDGE ( 'NONE', *, *, #20827, .T. ) ;
#50189 = DIRECTION ( 'NONE',  ( 0.000000000000000000, -1.000000000000000000, 0.000000000000000000 ) ) ;
#50190 = VECTOR ( 'NONE', #22993, 1000.000000000000000 ) ;
#50191 = CARTESIAN_POINT ( 'NONE',  ( 10.30302290646030627, 13.08520913973580058, -9.683996418299976483 ) ) ;
#50192 = VERTEX_POINT ( 'NONE', #49859 ) ;
#50193 = B_SPLINE_CURVE_WITH_KNOTS ( 'NONE', 3,
 ( #19012, #14671, #22365, #22874 ),
 .UNSPECIFIED., .F., .F.,
 ( 4, 4 ),
 ( 0.001937412222931638112, 0.003978261222106106373 ),
 .UNSPECIFIED. ) ;
#50194 = COLOUR_RGB ( '',0.7921568627450980005, 0.8196078431372548767, 0.9333333333333333481 ) ;
#50195 = CARTESIAN_POINT ( 'NONE',  ( -69.99999999999972999, 17.00000000000000000, -84.99999999999998579 ) ) ;
#50196 = FACE_BOUND ( 'NONE', #8460, .T. ) ;
#50197 = CARTESIAN_POINT ( 'NONE',  ( -0.4166666666666664631, 0.000000000000000000, 10.00000000000000000 ) ) ;
#50198 = CYLINDRICAL_SURFACE ( 'NONE', #13226, 1.750000000000015543 ) ;
#50199 = CIRCLE ( 'NONE', #42050, 0.5000000000000004441 ) ;
#50200 = DIRECTION ( 'NONE',  ( 0.000000000000000000, 0.000000000000000000, 1.000000000000000000 ) ) ;
#50201 = FACE_OUTER_BOUND ( 'NONE', #10225, .T. ) ;
#50202 = CARTESIAN_POINT ( 'NONE',  ( 164.9999999999999716, 17.00000000000000000, -55.00000000000000711 ) ) ;
#50203 = CARTESIAN_POINT ( 'NONE',  ( 135.0000000000021600, 17.00000000000000000, 95.00000000000000000 ) ) ;
#50204 = CARTESIAN_POINT ( 'NONE',  ( -28.52604530808686079, -41.07801380285659576, -3.760136334089591248 ) ) ;
#50205 = VERTEX_POINT ( 'NONE', #41972 ) ;
#50206 = LINE ( 'NONE', #26672, #1156 ) ;
#50207 = DIRECTION ( 'NONE',  ( -1.586032880504786307E-16, 1.654361225106055350E-24, -1.000000000000000000 ) ) ;
#50208 = AXIS2_PLACEMENT_3D ( 'NONE', #48258, #21101, #612 ) ;
#50209 = CARTESIAN_POINT ( 'NONE',  ( -5.505322767148756569, 37.09368438467003415, 8.914903342594564961 ) ) ;
#50210 = LINE ( 'NONE', #10757, #25689 ) ;
#50211 = ORIENTED_EDGE ( 'NONE', *, *, #22389, .T. ) ;
#50212 = CARTESIAN_POINT ( 'NONE',  ( -1.011271242968688533, 0.7347315653655859258, 10.00000000000000000 ) ) ;
#50213 = LINE ( 'NONE', #11788, #45001 ) ;
#50214 = CARTESIAN_POINT ( 'NONE',  ( 111.5540265531850537, 2.143131898507880377E-16, -160.9317124430720298 ) ) ;
#50215 = CARTESIAN_POINT ( 'NONE',  ( 153.3040265531850537, 0.000000000000000000, 165.0000000000000000 ) ) ;
#50216 =( NAMED_UNIT ( * ) PLANE_ANGLE_UNIT ( ) SI_UNIT ( $, .RADIAN. ) );
#50217 = EDGE_LOOP ( 'NONE', ( #3243, #41289, #49561, #4848 ) ) ;
#50218 = DIRECTION ( 'NONE',  ( -0.000000000000000000, -1.000000000000000000, -0.000000000000000000 ) ) ;
#50219 = EDGE_LOOP ( 'NONE', ( #15991, #41766, #1227, #33592, #47396 ) ) ;
#50220 = EDGE_CURVE ( 'NONE', #31254, #22853, #7085, .T. ) ;
#50221 = LINE ( 'NONE', #11796, #17190 ) ;
#50222 = VECTOR ( 'NONE', #16981, 1000.000000000000000 ) ;
#50223 = EDGE_LOOP ( 'NONE', ( #9358, #16053, #10608, #36136 ) ) ;
#50224 = DIRECTION ( 'NONE',  ( 6.203854594147707562E-25, -2.067951531382569187E-25, 1.000000000000000000 ) ) ;
#50225 = EDGE_CURVE ( 'NONE', #639, #2566, #42227, .T. ) ;
#50226 = VECTOR ( 'NONE', #15383, 1000.000000000000000 ) ;
#50227 = DIRECTION ( 'NONE',  ( 0.000000000000000000, 0.000000000000000000, 1.000000000000000000 ) ) ;
#50228 = ORIENTED_EDGE ( 'NONE', *, *, #49113, .T. ) ;
#50229 = FILL_AREA_STYLE ('',( #7194 ) ) ;
#50230 = ORIENTED_EDGE ( 'NONE', *, *, #29146, .F. ) ;
#50231 = VECTOR ( 'NONE', #32322, 1000.000000000000000 ) ;
#50232 = ADVANCED_FACE ( 'NONE', ( #22473 ), #18858, .T. ) ;
#50233 = AXIS2_PLACEMENT_3D ( 'NONE', #25920, #13832, #10004 ) ;
#50234 = EDGE_CURVE ( 'NONE', #24618, #22458, #45288, .T. ) ;
#50235 =( BOUNDED_CURVE ( )  B_SPLINE_CURVE ( 3, ( #19881, #12193, #12437, #40411 ),
 .UNSPECIFIED., .F., .F. ) 
 B_SPLINE_CURVE_WITH_KNOTS ( ( 4, 4 ),
 ( 4.712388980384689674, 6.283185307179586232 ),
 .UNSPECIFIED. ) 
 CURVE ( )  GEOMETRIC_REPRESENTATION_ITEM ( )  RATIONAL_B_SPLINE_CURVE ( ( 1.000000000000000000, 0.8047378541243649375, 0.8047378541243649375, 1.000000000000000000 ) ) 
 REPRESENTATION_ITEM ( '' )  );
#50236 = VERTEX_POINT ( 'NONE', #34540 ) ;
#50237 = CARTESIAN_POINT ( 'NONE',  ( 193.3040265531851105, -1.750000000000010658, -79.18171244307201562 ) ) ;
#50238 = FACE_OUTER_BOUND ( 'NONE', #14977, .T. ) ;
#50239 = VERTEX_POINT ( 'NONE', #30690 ) ;
#50240 = CARTESIAN_POINT ( 'NONE',  ( -166.6959734468149463, 0.000000000000000000, 165.0000000000000000 ) ) ;
#50241 = CARTESIAN_POINT ( 'NONE',  ( -15.00000000000001421, 17.00000000000000000, -114.9999999999999858 ) ) ;
#50242 = CARTESIAN_POINT ( 'NONE',  ( 166.9999999999999716, -168.9999999999999432, -350.0000000000001705 ) ) ;
#50243 =( BOUNDED_CURVE ( )  B_SPLINE_CURVE ( 3, ( #22030, #38221, #45846, #10993 ),
 .UNSPECIFIED., .F., .F. ) 
 B_SPLINE_CURVE_WITH_KNOTS ( ( 4, 4 ),
 ( 0.000000000000000000, 1.570796326794896558 ),
 .UNSPECIFIED. ) 
 CURVE ( )  GEOMETRIC_REPRESENTATION_ITEM ( )  RATIONAL_B_SPLINE_CURVE ( ( 1.000000000000000000, 0.8047378541243649375, 0.8047378541243649375, 1.000000000000000000 ) ) 
 REPRESENTATION_ITEM ( '' )  );
#50244 = ORIENTED_EDGE ( 'NONE', *, *, #22195, .F. ) ;
#50245 = ORIENTED_EDGE ( 'NONE', *, *, #16148, .T. ) ;
#50246 = PLANE ( 'NONE',  #31676 ) ;
#50247 = CARTESIAN_POINT ( 'NONE',  ( -86.69597344681494633, -1.750000000000010214, -39.18171244307202983 ) ) ;
#50248 = VECTOR ( 'NONE', #48133, 1000.000000000000000 ) ;
#50249 = VERTEX_POINT ( 'NONE', #14777 ) ;
#50250 = CARTESIAN_POINT ( 'NONE',  ( -88.44597344681491791, 0.000000000000000000, 162.5682875569279702 ) ) ;
#50251 = CARTESIAN_POINT ( 'NONE',  ( 0.3092340281093894361, -2.058543439737950731, 9.888808121373887872 ) ) ;
#50252 = ORIENTED_EDGE ( 'NONE', *, *, #41864, .T. ) ;
#50253 = CARTESIAN_POINT ( 'NONE',  ( 1.104609456715839766, 0.6504863887005235545, 9.948547179989622791 ) ) ;
#50254 = CARTESIAN_POINT ( 'NONE',  ( -114.9999999999984652, 17.00000000000000000, 60.00000000000000000 ) ) ;
#50255 = EDGE_CURVE ( 'NONE', #46979, #29314, #46293, .T. ) ;
#50256 = EDGE_LOOP ( 'NONE', ( #35776, #1905, #16341, #38446, #43128, #21559, #16409, #39118 ) ) ;
#50257 = EDGE_CURVE ( 'NONE', #44495, #29622, #10965, .T. ) ;
#50258 = CARTESIAN_POINT ( 'NONE',  ( 232.4999999999999716, -169.9999999999999716, 4.999999999999616307 ) ) ;
#50259 = FACE_OUTER_BOUND ( 'NONE', #12635, .T. ) ;
#50260 = EDGE_CURVE ( 'NONE', #297, #17433, #10921, .T. ) ;
#50261 = ADVANCED_FACE ( 'NONE', ( #41469 ), #3206, .F. ) ;
#50262 = AXIS2_PLACEMENT_3D ( 'NONE', #31835, #47420, #12307 ) ;
#50263 = ORIENTED_EDGE ( 'NONE', *, *, #28630, .F. ) ;
#50264 = AXIS2_PLACEMENT_3D ( 'NONE', #1221, #29170, #9152 ) ;
#50265 = PLANE ( 'NONE',  #40894 ) ;
#50266 = EDGE_CURVE ( 'NONE', #46387, #20835, #16228, .T. ) ;
#50267 = LINE ( 'NONE', #6710, #24260 ) ;
#50268 = CIRCLE ( 'NONE', #34786, 4.000000000000003553 ) ;
#50269 = ADVANCED_FACE ( 'NONE', ( #49375 ), #37897, .F. ) ;
#50270 = CARTESIAN_POINT ( 'NONE',  ( 1.011271242968677653, 0.7347315653656002477, -3.333333333333333481 ) ) ;
#50271 = ORIENTED_EDGE ( 'NONE', *, *, #48296, .T. ) ;
#50272 = VECTOR ( 'NONE', #25149, 1000.000000000000000 ) ;
#50273 = VERTEX_POINT ( 'NONE', #14518 ) ;
#50274 = CARTESIAN_POINT ( 'NONE',  ( 717.1787655628115772, 792.7343818612995392, 1344.137589624066550 ) ) ;
#50275 = CARTESIAN_POINT ( 'NONE',  ( -124.9459734468149463, 2.143131898507847836E-16, 82.56828755692797017 ) ) ;
#50276 = FACE_OUTER_BOUND ( 'NONE', #18778, .T. ) ;
#50277 = LINE ( 'NONE', #11847, #21743 ) ;
#50278 = DIRECTION ( 'NONE',  ( -1.000000000000000000, -0.000000000000000000, 4.625929269271584521E-16 ) ) ;
#50279 = CARTESIAN_POINT ( 'NONE',  ( 25.60949810002064098, 43.19700938445193827, 1.847720168420772691 ) ) ;
#50280 = ORIENTED_EDGE ( 'NONE', *, *, #33997, .F. ) ;
#50281 = CARTESIAN_POINT ( 'NONE',  ( -114.9999999999991047, 17.00000000000000000, -24.99999999999999289 ) ) ;
#50282 = PRODUCT_DEFINITION_SHAPE ( 'NONE', 'NONE',  #50724 ) ;
#50283 = CARTESIAN_POINT ( 'NONE',  ( -3.566525152643847285, 1.569997364305458776, 9.741991644046965604 ) ) ;
#50284 = CARTESIAN_POINT ( 'NONE',  ( -1.343171584780018746, 1.414327272009577641, 9.896382706792429929 ) ) ;
#50285 = EDGE_CURVE ( 'NONE', #15830, #17104, #33454, .T. ) ;
#50286 = AXIS2_PLACEMENT_3D ( 'NONE', #12161, #39377, #19595 ) ;
#50287 = EDGE_CURVE ( 'NONE', #11996, #40379, #22824, .T. ) ;
#50288 = SURFACE_SIDE_STYLE ('',( #34715 ) ) ;
#50289 = VERTEX_POINT ( 'NONE', #5474 ) ;
#50290 = EDGE_CURVE ( 'NONE', #21162, #38025, #33207, .T. ) ;
#50291 = CARTESIAN_POINT ( 'NONE',  ( 350.0000000000000000, 165.0000000000000000, -344.0000000000001705 ) ) ;
#50292 = CARTESIAN_POINT ( 'NONE',  ( 22.69295089195473736, 45.31600496604706052, 7.455576670931136185 ) ) ;
#50293 = EDGE_LOOP ( 'NONE', ( #45522, #20394, #105, #22495 ) ) ;
#50294 = DIRECTION ( 'NONE',  ( -0.000000000000000000, -1.000000000000000000, -0.000000000000000000 ) ) ;
#50295 = CARTESIAN_POINT ( 'NONE',  ( 33.30402655318503946, 1.750000000000010214, 40.81828755692798438 ) ) ;
#50296 = DIRECTION ( 'NONE',  ( -1.000000000000000000, 0.000000000000000000, 0.000000000000000000 ) ) ;
#50298 = ORIENTED_EDGE ( 'NONE', *, *, #18938, .T. ) ;
#50297 = B_SPLINE_CURVE_WITH_KNOTS ( 'NONE', 3,
 ( #34298, #49881, #3754, #7876 ),
 .UNSPECIFIED., .F., .F.,
 ( 4, 4 ),
 ( 6.527761501258140853E-19, 0.0003137973357029442208 ),
 .UNSPECIFIED. ) ;
#50299 = CARTESIAN_POINT ( 'NONE',  ( -164.9459734468149463, 2.143131898507880377E-16, -80.93171244307201562 ) ) ;
#50300 = DIRECTION ( 'NONE',  ( -0.000000000000000000, -0.000000000000000000, -1.000000000000000000 ) ) ;
#50301 = ORIENTED_EDGE ( 'NONE', *, *, #7691, .F. ) ;
#50302 = CARTESIAN_POINT ( 'NONE',  ( -44.94597344681493922, 1.025126265847089435, 39.06828755692797728 ) ) ;
#50303 = FACE_OUTER_BOUND ( 'NONE', #6708, .T. ) ;
#50304 = EDGE_CURVE ( 'NONE', #44732, #2449, #45198, .T. ) ;
#50305 = ORIENTED_EDGE ( 'NONE', *, *, #40896, .T. ) ;
#50306 = ORIENTED_EDGE ( 'NONE', *, *, #44607, .T. ) ;
#50307 = CARTESIAN_POINT ( 'NONE',  ( 153.3040265531850537, 1.750000000000010214, -39.18171244307202983 ) ) ;
#50308 = VECTOR ( 'NONE', #6587, 1000.000000000000000 ) ;
#50309 = CARTESIAN_POINT ( 'NONE',  ( 111.5540265531850537, -1.025126265847082108, -77.43171244307201562 ) ) ;
#50310 = ORIENTED_EDGE ( 'NONE', *, *, #24754, .T. ) ;
#50311 = EDGE_LOOP ( 'NONE', ( #3477, #25907, #36639, #11673, #42916, #383 ) ) ;
#50312 = CARTESIAN_POINT ( 'NONE',  ( 34.08406891383362591, -15.63733501198463038, -8.192531242611266862 ) ) ;
#50313 = CARTESIAN_POINT ( 'NONE',  ( 210.0000000000000568, 0.000000000000000000, 0.8182875569279768335 ) ) ;
#50314 = LINE ( 'NONE', #14968, #18214 ) ;
#50315 = ADVANCED_FACE ( 'NONE', ( #10088 ), #48794, .F. ) ;
#50316 = ORIENTED_EDGE ( 'NONE', *, *, #12725, .T. ) ;
#50317 = LINE ( 'NONE', #30892, #7965 ) ;
#50318 = VERTEX_POINT ( 'NONE', #13681 ) ;
#50319 = LINE ( 'NONE', #39104, #26317 ) ;
#50320 = CARTESIAN_POINT ( 'NONE',  ( 35.00000000000061107, 17.00000000000000000, -30.00000000000000000 ) ) ;
#50321 = DIRECTION ( 'NONE',  ( 1.132880637372608740E-16, 4.718402560806925739E-50, 1.000000000000000000 ) ) ;
#50322 = EDGE_CURVE ( 'NONE', #26096, #19789, #21449, .T. ) ;
#50323 = CIRCLE ( 'NONE', #17631, 40.00000000000000000 ) ;
#50325 = ORIENTED_EDGE ( 'NONE', *, *, #46638, .T. ) ;
#50324 = EDGE_CURVE ( 'NONE', #34466, #22541, #37063, .T. ) ;
#50326 = ORIENTED_EDGE ( 'NONE', *, *, #43545, .F. ) ;
#50327 = SHAPE_REPRESENTATION ( 'wire', ( #45486 ), #43870 ) ;
#50328 = ORIENTED_EDGE ( 'NONE', *, *, #44930, .F. ) ;
#50329 = AXIS2_PLACEMENT_3D ( 'NONE', #17462, #4894, #40316 ) ;
#50330 = PLANE ( 'NONE',  #42695 ) ;
#50331 = CARTESIAN_POINT ( 'NONE',  ( 185.0000000000000000, -256.4999999999999432, -114.9999999999999432 ) ) ;
#50332 = CYLINDRICAL_SURFACE ( 'NONE', #19123, 1.750000000000008438 ) ;
#50333 = EDGE_CURVE ( 'NONE', #5824, #42182, #49533, .T. ) ;
#50334 = VERTEX_POINT ( 'NONE', #20877 ) ;
#50335 = CARTESIAN_POINT ( 'NONE',  ( -164.4973046169135955, -97.66198943095992036, 23.74256005001722158 ) ) ;
#50336 = VERTEX_POINT ( 'NONE', #24993 ) ;
#50337 = EDGE_CURVE ( 'NONE', #26504, #36589, #31971, .T. ) ;
#50338 = PLANE ( 'NONE',  #12709 ) ;
#50339 = ORIENTED_EDGE ( 'NONE', *, *, #26448, .T. ) ;
#50340 = DIRECTION ( 'NONE',  ( -1.000000000000000000, 0.000000000000000000, 1.860490536778032451E-50 ) ) ;
#50341 = EDGE_CURVE ( 'NONE', #343, #39269, #37564, .T. ) ;
#50342 = DIRECTION ( 'NONE',  ( -1.000000000000000000, -0.000000000000000000, -0.000000000000000000 ) ) ;
#50343 = CARTESIAN_POINT ( 'NONE',  ( -16.69947034530963847, 2.312583065866374632, 2.590526750877053086 ) ) ;
#50344 = DIRECTION ( 'NONE',  ( 1.000000000000000000, 0.000000000000000000, 0.000000000000000000 ) ) ;
#50345 = CARTESIAN_POINT ( 'NONE',  ( 0.6108107228405675881, -1.056024183042613140, 9.963925895596188909 ) ) ;
#50346 = ORIENTED_EDGE ( 'NONE', *, *, #39395, .T. ) ;
#50347 = ORIENTED_EDGE ( 'NONE', *, *, #16741, .F. ) ;
#50348 = DIRECTION ( 'NONE',  ( 0.000000000000000000, 0.000000000000000000, -1.000000000000000000 ) ) ;
#50349 = CARTESIAN_POINT ( 'NONE',  ( 0.000000000000000000, 28.48684210526315752, -5.000000000000000000 ) ) ;
#50350 = EDGE_CURVE ( 'NONE', #20029, #14416, #13425, .T. ) ;
#50351 = LINE ( 'NONE', #19353, #11362 ) ;
#50352 = DIRECTION ( 'NONE',  ( -0.000000000000000000, -0.000000000000000000, -1.000000000000000000 ) ) ;
#50353 = AXIS2_PLACEMENT_3D ( 'NONE', #2290, #45857, #33358 ) ;
#50354 = CARTESIAN_POINT ( 'NONE',  ( -4.999999999999948486, -204.9999999999999716, -230.2499999999999716 ) ) ;
#50355 = EDGE_CURVE ( 'NONE', #28730, #43135, #2384, .T. ) ;
#50356 = CARTESIAN_POINT ( 'NONE',  ( 181.0000000000000000, -93.49999999999997158, -115.0000000000001563 ) ) ;
#50357 = EDGE_LOOP ( 'NONE', ( #7491, #29913, #26935 ) ) ;
#50358 = LINE ( 'NONE', #45518, #31968 ) ;
#50359 = CARTESIAN_POINT ( 'NONE',  ( 181.0000000000000000, -268.4999999999999432, -349.9999999999999432 ) ) ;
#50360 = VERTEX_POINT ( 'NONE', #32956 ) ;
#50361 = AXIS2_PLACEMENT_3D ( 'NONE', #43721, #8590, #47292 ) ;
#50362 = DIRECTION ( 'NONE',  ( -0.000000000000000000, -1.000000000000000000, -0.000000000000000000 ) ) ;
#50363 = AXIS2_PLACEMENT_3D ( 'NONE', #24108, #21245, #20742 ) ;
#50364 = LINE ( 'NONE', #35815, #31947 ) ;
#50365 = CARTESIAN_POINT ( 'NONE',  ( 0.9599924130074096729, -0.8495346730527926216, 9.948547179989617462 ) ) ;
#50366 = AXIS2_PLACEMENT_3D ( 'NONE', #11911, #43692, #11393 ) ;
#50367 = ORIENTED_EDGE ( 'NONE', *, *, #31857, .F. ) ;
#50368 = ORIENTED_EDGE ( 'NONE', *, *, #23316, .T. ) ;
#50369 = CARTESIAN_POINT ( 'NONE',  ( 74.32915281903215998, 1.750000000000009548, 41.84341382277508359 ) ) ;
#50370 = CARTESIAN_POINT ( 'NONE',  ( -1.250000000000000222, 0.000000000000000000, 10.00000000000000000 ) ) ;
#50371 = VECTOR ( 'NONE', #41874, 1000.000000000000000 ) ;
#50372 = ORIENTED_EDGE ( 'NONE', *, *, #27872, .F. ) ;
#50373 = ORIENTED_EDGE ( 'NONE', *, *, #24123, .T. ) ;
#50374 = CARTESIAN_POINT ( 'NONE',  ( 29.61572577327002520, 16.11461842845735859, 8.807470649214879543 ) ) ;
#50375 = DIRECTION ( 'NONE',  ( 0.000000000000000000, 0.000000000000000000, 1.000000000000000000 ) ) ;
#50376 = DIRECTION ( 'NONE',  ( -1.586032892321652236E-16, -1.000000000000000000, -2.288264760618012091E-48 ) ) ;
#50377 = VECTOR ( 'NONE', #50340, 1000.000000000000000 ) ;
#50378 = VECTOR ( 'NONE', #21038, 1000.000000000000000 ) ;
#50379 = ORIENTED_EDGE ( 'NONE', *, *, #48489, .F. ) ;
#50380 = ORIENTED_EDGE ( 'NONE', *, *, #50162, .F. ) ;
#50381 = ORIENTED_EDGE ( 'NONE', *, *, #30641, .T. ) ;
#50382 = PRODUCT_DEFINITION_FORMATION_WITH_SPECIFIED_SOURCE ( 'ANY', '', #10156, .NOT_KNOWN. ) ;
#50383 = CIRCLE ( 'NONE', #6998, 0.4999999999999992228 ) ;
#50384 = CARTESIAN_POINT ( 'NONE',  ( -6.695973446814940111, -1.750000000000024203, 120.8182875569279702 ) ) ;
#50385 = DIRECTION ( 'NONE',  ( 7.793956916774525800E-48, 0.000000000000000000, 1.000000000000000000 ) ) ;
#50386 =( BOUNDED_CURVE ( )  B_SPLINE_CURVE ( 3, ( #2480, #9674, #29426, #14272 ),
 .UNSPECIFIED., .F., .F. ) 
 B_SPLINE_CURVE_WITH_KNOTS ( ( 4, 4 ),
 ( 0.000000000000000000, 1.570796326794896558 ),
 .UNSPECIFIED. ) 
 CURVE ( )  GEOMETRIC_REPRESENTATION_ITEM ( )  RATIONAL_B_SPLINE_CURVE ( ( 1.000000000000000000, 0.8047378541243649375, 0.8047378541243649375, 1.000000000000000000 ) ) 
 REPRESENTATION_ITEM ( '' )  );
#50387 = ORIENTED_EDGE ( 'NONE', *, *, #35549, .F. ) ;
#50388 = EDGE_CURVE ( 'NONE', #9299, #21262, #36559, .T. ) ;
#50389 = DIRECTION ( 'NONE',  ( 1.000000000000000000, 0.000000000000000000, 0.000000000000000000 ) ) ;
#50390 = EDGE_CURVE ( 'NONE', #40728, #12217, #44947, .T. ) ;
#50391 = LINE ( 'NONE', #11441, #26598 ) ;
#50392 = CARTESIAN_POINT ( 'NONE',  ( 112.2789002873379758, 1.749999999999996669, -118.1565861772249661 ) ) ;
#50393 = ORIENTED_EDGE ( 'NONE', *, *, #48086, .F. ) ;
#50394 = EDGE_LOOP ( 'NONE', ( #45153, #14380, #48674, #36270, #17794, #531 ) ) ;
#50395 = DIRECTION ( 'NONE',  ( 1.000000000000000000, 0.000000000000000000, 0.000000000000000000 ) ) ;
#50397 = DIRECTION ( 'NONE',  ( 1.341289691698241816E-15, -1.000000000000000000, 1.822804496942679766E-16 ) ) ;
#50396 =( BOUNDED_CURVE ( )  B_SPLINE_CURVE ( 3, ( #40740, #28928, #44302, #28436 ),
 .UNSPECIFIED., .F., .F. ) 
 B_SPLINE_CURVE_WITH_KNOTS ( ( 4, 4 ),
 ( 3.141592653589793116, 4.712388980384689674 ),
 .UNSPECIFIED. ) 
 CURVE ( )  GEOMETRIC_REPRESENTATION_ITEM ( )  RATIONAL_B_SPLINE_CURVE ( ( 1.000000000000000000, 0.8047378541243649375, 0.8047378541243649375, 1.000000000000000000 ) ) 
 REPRESENTATION_ITEM ( '' )  );
#50398 = DIRECTION ( 'NONE',  ( -1.000000000000000000, -0.000000000000000000, -0.000000000000000000 ) ) ;
#50399 = EDGE_CURVE ( 'NONE', #8725, #47613, #48535, .T. ) ;
#50400 = VERTEX_POINT ( 'NONE', #13178 ) ;
#50401 = VERTEX_POINT ( 'NONE', #9585 ) ;
#50402 = EDGE_CURVE ( 'NONE', #31529, #16294, #29547, .T. ) ;
#50403 = CARTESIAN_POINT ( 'NONE',  ( 48.33712804702526000, 13.03701565032775456, -9.367992836599954742 ) ) ;
#50404 = EDGE_CURVE ( 'NONE', #6144, #7014, #30016, .T. ) ;
#50405 = AXIS2_PLACEMENT_3D ( 'NONE', #28281, #43916, #13629 ) ;
#50406 = DIRECTION ( 'NONE',  ( -0.000000000000000000, 1.000000000000000000, 0.000000000000000000 ) ) ;
#50407 = CARTESIAN_POINT ( 'NONE',  ( 0.000000000000000000, 169.0000000000000000, 339.9999999999997726 ) ) ;
#50408 = CARTESIAN_POINT ( 'NONE',  ( 35.00000000000091660, 16.00000000000000000, 0.000000000000000000 ) ) ;
#50409 = CARTESIAN_POINT ( 'NONE',  ( 339.9999999999999432, -165.0000000000001137, -106.0000000000001990 ) ) ;
#50410 = EDGE_LOOP ( 'NONE', ( #16736, #30077, #36005, #42959 ) ) ;
#50412 = ADVANCED_FACE ( 'NONE', ( #3816 ), #11269, .T. ) ;
#50411 =( NAMED_UNIT ( * ) SI_UNIT ( $, .STERADIAN. ) SOLID_ANGLE_UNIT ( ) );
#50413 = FACE_OUTER_BOUND ( 'NONE', #4667, .T. ) ;
#50414 = CIRCLE ( 'NONE', #10204, 4.000000000000003553 ) ;
#50415 = EDGE_CURVE ( 'NONE', #44239, #41902, #38235, .T. ) ;
#50416 =( BOUNDED_CURVE ( )  B_SPLINE_CURVE ( 3, ( #9788, #24957, #25198, #5945 ),
 .UNSPECIFIED., .F., .F. ) 
 B_SPLINE_CURVE_WITH_KNOTS ( ( 4, 4 ),
 ( 0.000000000000000000, 1.570796326794896558 ),
 .UNSPECIFIED. ) 
 CURVE ( )  GEOMETRIC_REPRESENTATION_ITEM ( )  RATIONAL_B_SPLINE_CURVE ( ( 1.000000000000000000, 0.8047378541243649375, 0.8047378541243649375, 1.000000000000000000 ) ) 
 REPRESENTATION_ITEM ( '' )  );
#50417 = CARTESIAN_POINT ( 'NONE',  ( 0.9923808968705242206, -0.8303844723052218324, 9.947020512645417867 ) ) ;
#50418 = CARTESIAN_POINT ( 'NONE',  ( -44.94597344681493922, 2.143131898507882349E-16, 165.0000000000000000 ) ) ;
#50419 = PRESENTATION_LAYER_ASSIGNMENT (  '', '', ( #48780 ) ) ;
#50420 = ORIENTED_EDGE ( 'NONE', *, *, #18887, .T. ) ;
#50421 = CARTESIAN_POINT ( 'NONE',  ( 8.277096487746778308, -33.14818118907697198, 7.455576670931136185 ) ) ;
#50422 = DIRECTION ( 'NONE',  ( -1.000000000000000000, -0.000000000000000000, -0.000000000000000000 ) ) ;
#50423 = LINE ( 'NONE', #31751, #13994 ) ;
#50424 = VECTOR ( 'NONE', #22156, 1000.000000000000000 ) ;
#50425 = VERTEX_POINT ( 'NONE', #38983 ) ;
#50426 = PRESENTATION_STYLE_ASSIGNMENT (( #49904 ) ) ;
#50427 = CARTESIAN_POINT ( 'NONE',  ( 14.49999999999999822, 13.48684210526315930, -20.00000000000000000 ) ) ;
#50428 = ORIENTED_EDGE ( 'NONE', *, *, #41760, .F. ) ;
#50429 = CARTESIAN_POINT ( 'NONE',  ( -164.9999999999994031, 17.00000000000000000, -30.00000000000000000 ) ) ;
#50430 = CARTESIAN_POINT ( 'NONE',  ( 5.204748896376250699E-16, 13.48684210526315930, 4.250000000000000000 ) ) ;
#50431 = CARTESIAN_POINT ( 'NONE',  ( -86.69597344681494633, 1.750000000000010214, -39.18171244307202983 ) ) ;
#50432 = EDGE_CURVE ( 'NONE', #17930, #30535, #49955, .T. ) ;
#50433 = VERTEX_POINT ( 'NONE', #23055 ) ;
#50434 = ORIENTED_EDGE ( 'NONE', *, *, #36986, .F. ) ;
#50435 = ORIENTED_EDGE ( 'NONE', *, *, #12170, .T. ) ;
#50436 = EDGE_CURVE ( 'NONE', #25384, #4446, #48974, .T. ) ;
#50437 = CARTESIAN_POINT ( 'NONE',  ( -0.3501237319956617688, 1.209643720083639851, 9.974012008644017158 ) ) ;
#50438 = VECTOR ( 'NONE', #27715, 1000.000000000000000 ) ;
#50439 = VECTOR ( 'NONE', #43355, 1000.000000000000000 ) ;
#50440 = ORIENTED_EDGE ( 'NONE', *, *, #6677, .F. ) ;
#50441 = DIRECTION ( 'NONE',  ( -1.586032880504786307E-16, 1.654361225106055350E-24, -1.000000000000000000 ) ) ;
#50442 = CARTESIAN_POINT ( 'NONE',  ( -127.7210997126620242, 1.749999999999996669, 161.8434138227750907 ) ) ;
#50443 = VECTOR ( 'NONE', #47435, 1000.000000000000000 ) ;
#50444 = CARTESIAN_POINT ( 'NONE',  ( -194.9999999999999432, -173.0000000000000000, 352.0000000000000568 ) ) ;
#50445 = LINE ( 'NONE', #42527, #35012 ) ;
#50446 = ORIENTED_EDGE ( 'NONE', *, *, #42232, .F. ) ;
#50447 = CARTESIAN_POINT ( 'NONE',  ( -128.4459734468149179, 0.000000000000000000, -157.4317124430720582 ) ) ;
#50448 = FACE_OUTER_BOUND ( 'NONE', #27185, .T. ) ;
#50449 = CARTESIAN_POINT ( 'NONE',  ( -120.0000000000000426, 17.00000000000000000, -90.00000000000000000 ) ) ;
#50450 = VECTOR ( 'NONE', #5942, 1000.000000000000000 ) ;
#50451 = ORIENTED_EDGE ( 'NONE', *, *, #22677, .T. ) ;
#50452 = CARTESIAN_POINT ( 'NONE',  ( -168.4459734468149747, -1.025126265847089657, 42.56828755692799149 ) ) ;
#50453 = CARTESIAN_POINT ( 'NONE',  ( 339.9999999999998863, -180.9999999999999716, 341.9999999999997726 ) ) ;
#50454 = ORIENTED_EDGE ( 'NONE', *, *, #7011, .T. ) ;
#50455 = EDGE_LOOP ( 'NONE', ( #43180, #9616, #16406, #32695 ) ) ;
#50456 = ORIENTED_EDGE ( 'NONE', *, *, #22132, .T. ) ;
#50457 = CARTESIAN_POINT ( 'NONE',  ( -1.326845121651818227, 0.3624933883365418219, 9.972175347158394487 ) ) ;
#50458 = PLANE ( 'NONE',  #18482 ) ;
#50459 = ORIENTED_EDGE ( 'NONE', *, *, #47704, .F. ) ;
#50460 = CIRCLE ( 'NONE', #28395, 0.5000000000000004441 ) ;
#50461 = CARTESIAN_POINT ( 'NONE',  ( 44.99506233596246574, 23.32283626942318477, 7.455576670931136185 ) ) ;
#50462 = DIRECTION ( 'NONE',  ( 0.1191452206184309831, 0.000000000000000000, -0.9928768384869219865 ) ) ;
#50463 = CARTESIAN_POINT ( 'NONE',  ( 154.1026953830863420, -98.56198943095992604, -17.65743994998277699 ) ) ;
#50464 = CARTESIAN_POINT ( 'NONE',  ( -126.6959734468149321, 1.749999999999996891, -159.1817124430720298 ) ) ;
#50465 = CARTESIAN_POINT ( 'NONE',  ( 169.0000000000000000, -174.9999999999999716, -95.00000000000014211 ) ) ;
#50466 = CARTESIAN_POINT ( 'NONE',  ( 9.999999999999998224, 0.04986450829246079353, 8.654293224463657452 ) ) ;
#50467 = PLANE ( 'NONE',  #48642 ) ;
#50468 = EDGE_CURVE ( 'NONE', #40222, #7778, #42051, .T. ) ;
#50469 = CARTESIAN_POINT ( 'NONE',  ( 130.0000000000002842, 17.00000000000000000, -84.99999999999998579 ) ) ;
#50471 = B_SPLINE_CURVE_WITH_KNOTS ( 'NONE', 3,
 ( #31997, #32244, #20178, #17086 ),
 .UNSPECIFIED., .F., .F.,
 ( 4, 4 ),
 ( 0.001152428489661398931, 0.001623376834729704571 ),
 .UNSPECIFIED. ) ;
#50470 = DIRECTION ( 'NONE',  ( 1.000000000000000000, 0.000000000000000000, 0.000000000000000000 ) ) ;
#50472 = ORIENTED_EDGE ( 'NONE', *, *, #28126, .T. ) ;
#50473 = DIRECTION ( 'NONE',  ( 1.000000000000000000, 0.000000000000000000, -0.000000000000000000 ) ) ;
#50474 = CARTESIAN_POINT ( 'NONE',  ( 210.0000000000000568, 0.000000000000000000, 122.5682875569279844 ) ) ;
#50475 = VECTOR ( 'NONE', #32850, 1000.000000000000000 ) ;
#50477 = VECTOR ( 'NONE', #48570, 1000.000000000000000 ) ;
#50476 = DIRECTION ( 'NONE',  ( 1.333906992743555050E-23, -1.000000000000000000, 0.000000000000000000 ) ) ;
#50478 = CYLINDRICAL_SURFACE ( 'NONE', #15832, 1.750000000000008438 ) ;
#50479 = VERTEX_POINT ( 'NONE', #7427 ) ;
#50480 = CARTESIAN_POINT ( 'NONE',  ( -119.9999999999981668, 16.00000000000000000, 90.00000000000000000 ) ) ;
#50481 = DIRECTION ( 'NONE',  ( -1.586032892321652236E-16, -1.000000000000000000, -6.853681917100419162E-49 ) ) ;
#50482 = CARTESIAN_POINT ( 'NONE',  ( -45.42829307628559832, -21.98948915213271960, 8.356839323120299312 ) ) ;
#50483 = CARTESIAN_POINT ( 'NONE',  ( 181.0000000000000284, -174.9999999999999716, -115.0000000000001563 ) ) ;
#50484 = CARTESIAN_POINT ( 'NONE',  ( -0.3862712429686977478, 1.188820645368937390, -3.333333333333333481 ) ) ;
#50485 = VERTEX_POINT ( 'NONE', #22805 ) ;
#50486 = DIRECTION ( 'NONE',  ( -0.000000000000000000, -0.000000000000000000, -1.000000000000000000 ) ) ;
#50487 = VERTEX_POINT ( 'NONE', #42800 ) ;
#50488 = CARTESIAN_POINT ( 'NONE',  ( 75.05402655318509630, 2.143131898507880377E-16, 159.0682875569279702 ) ) ;
#50489 = ORIENTED_EDGE ( 'NONE', *, *, #23750, .T. ) ;
#50490 = DIRECTION ( 'NONE',  ( -1.000000000000000000, 4.758098676964957447E-16, 1.586032892321651989E-16 ) ) ;
#50491 = ORIENTED_EDGE ( 'NONE', *, *, #12166, .F. ) ;
#50492 = LINE ( 'NONE', #31317, #8481 ) ;
#50493 = B_SPLINE_CURVE_WITH_KNOTS ( 'NONE', 3,
 ( #41368, #13895, #41618, #37788 ),
 .UNSPECIFIED., .F., .F.,
 ( 4, 4 ),
 ( 0.000000000000000000, 0.0002610106747148429121 ),
 .UNSPECIFIED. ) ;
#50494 = ORIENTED_EDGE ( 'NONE', *, *, #49365, .F. ) ;
#50495 = VECTOR ( 'NONE', #37696, 1000.000000000000000 ) ;
#50496 = EDGE_CURVE ( 'NONE', #18024, #25772, #40500, .T. ) ;
#50497 = ORIENTED_EDGE ( 'NONE', *, *, #38535, .T. ) ;
#50498 = FACE_OUTER_BOUND ( 'NONE', #32897, .T. ) ;
#50499 = CARTESIAN_POINT ( 'NONE',  ( 339.9999999999999432, 181.0000000000002274, -356.0000000000003411 ) ) ;
#50500 = VERTEX_POINT ( 'NONE', #30261 ) ;
#50501 = CARTESIAN_POINT ( 'NONE',  ( -27.33593271309441519, 41.94268121623345991, -9.367992836599954742 ) ) ;
#50502 = CARTESIAN_POINT ( 'NONE',  ( 350.0000000000000000, 181.0000000000000284, -356.0000000000002274 ) ) ;
#50503 = DIRECTION ( 'NONE',  ( 0.000000000000000000, -2.265761274745217480E-16, 1.000000000000000000 ) ) ;
#50504 = ORIENTED_EDGE ( 'NONE', *, *, #46903, .F. ) ;
#50505 = CARTESIAN_POINT ( 'NONE',  ( 339.9999999999998863, -174.9999999999999716, 359.9999999999998295 ) ) ;
#50506 = DIRECTION ( 'NONE',  ( 0.000000000000000000, 0.000000000000000000, 1.000000000000000000 ) ) ;
#50507 = VERTEX_POINT ( 'NONE', #7938 ) ;
#50508 = CIRCLE ( 'NONE', #2215, 1.750000000000008438 ) ;
#50509 = CARTESIAN_POINT ( 'NONE',  ( -166.6959734468149463, 1.750000000000010214, -39.18171244307202983 ) ) ;
#50510 = CARTESIAN_POINT ( 'NONE',  ( 350.0000000000001137, 167.0000000000000000, 355.9999999999997726 ) ) ;
#50511 = ORIENTED_EDGE ( 'NONE', *, *, #5097, .T. ) ;
#50512 = DIRECTION ( 'NONE',  ( -1.000000000000000000, -0.000000000000000000, -0.000000000000000000 ) ) ;
#50513 = DIRECTION ( 'NONE',  ( 0.000000000000000000, 0.000000000000000000, 1.000000000000000000 ) ) ;
#50514 = ORIENTED_EDGE ( 'NONE', *, *, #46993, .F. ) ;
#50515 = CARTESIAN_POINT ( 'NONE',  ( 210.0000000000000568, 2.143131898507880377E-16, -0.9317124430720331585 ) ) ;
#50516 = CARTESIAN_POINT ( 'NONE',  ( 342.0000000000000000, -167.8284271247461561, 342.8284271247460424 ) ) ;
#50517 = FACE_OUTER_BOUND ( 'NONE', #32073, .T. ) ;
#50518 = DIRECTION ( 'NONE',  ( -8.673617379884028076E-17, 1.000000000000000000, 0.000000000000000000 ) ) ;
#50519 = ORIENTED_EDGE ( 'NONE', *, *, #9570, .F. ) ;
#50520 = CARTESIAN_POINT ( 'NONE',  ( 73.30402655318508209, 0.000000000000000000, 165.0000000000000000 ) ) ;
#50522 = EDGE_CURVE ( 'NONE', #23700, #28202, #15617, .T. ) ;
#50521 = CARTESIAN_POINT ( 'NONE',  ( 195.0540265531851105, 2.143131898507880377E-16, 162.5682875569279702 ) ) ;
#50523 = CARTESIAN_POINT ( 'NONE',  ( 0.1287570809895660084, -0.3962735484563127408, 10.00000000000000000 ) ) ;
#50524 = ORIENTED_EDGE ( 'NONE', *, *, #36466, .F. ) ;
#50525 = EDGE_CURVE ( 'NONE', #11488, #13632, #50634, .T. ) ;
#50526 = ORIENTED_EDGE ( 'NONE', *, *, #43751, .F. ) ;
#50527 = DIRECTION ( 'NONE',  ( -0.02649601436921053890, 1.407572200354884729E-14, 0.9996489189823327681 ) ) ;
#50528 = EDGE_CURVE ( 'NONE', #30729, #40331, #2550, .T. ) ;
#50529 = CARTESIAN_POINT ( 'NONE',  ( 31.55402655318503236, 0.000000000000000000, 39.06828755692798438 ) ) ;
#50530 = DIRECTION ( 'NONE',  ( -0.000000000000000000, -1.000000000000000000, -0.000000000000000000 ) ) ;
#50531 = FACE_OUTER_BOUND ( 'NONE', #2899, .T. ) ;
#50532 = DIRECTION ( 'NONE',  ( 0.000000000000000000, 0.000000000000000000, -1.000000000000000000 ) ) ;
#50533 = LINE ( 'NONE', #46695, #19890 ) ;
#50534 = VERTEX_POINT ( 'NONE', #26663 ) ;
#50535 = CARTESIAN_POINT ( 'NONE',  ( -33.89193117067290473, 0.000000000000000000, 910.0000000000000000 ) ) ;
#50536 = EDGE_CURVE ( 'NONE', #46762, #20108, #11522, .T. ) ;
#50537 = EDGE_CURVE ( 'NONE', #39708, #45594, #7675, .T. ) ;
#50538 = DIRECTION ( 'NONE',  ( -1.000000000000000000, -0.000000000000000000, -0.000000000000000000 ) ) ;
#50539 = CARTESIAN_POINT ( 'NONE',  ( -165.6708471809677974, 1.750000000000009548, 159.7931612910809065 ) ) ;
#50540 = DIRECTION ( 'NONE',  ( -1.000000000000000000, 0.000000000000000000, -1.612977847700450206E-50 ) ) ;
#50541 = ADVANCED_FACE ( 'NONE', ( #27174 ), #42547, .T. ) ;
#50542 = B_SPLINE_CURVE_WITH_KNOTS ( 'NONE', 3,
 ( #17294, #24757, #40147, #20640 ),
 .UNSPECIFIED., .F., .F.,
 ( 4, 4 ),
 ( 0.9688112071879384501, 0.9724175925769211748 ),
 .UNSPECIFIED. ) ;
#50544 = ORIENTED_EDGE ( 'NONE', *, *, #16062, .T. ) ;
#50543 = AXIS2_PLACEMENT_3D ( 'NONE', #33251, #25527, #29627 ) ;
#50545 = DIRECTION ( 'NONE',  ( 0.000000000000000000, 1.000000000000000000, -3.186989995019654210E-49 ) ) ;
#50546 = CARTESIAN_POINT ( 'NONE',  ( 23.26005729352310425, 44.90397804740356236, 7.906207997025717304 ) ) ;
#50547 = ORIENTED_EDGE ( 'NONE', *, *, #28220, .T. ) ;
#50548 = CARTESIAN_POINT ( 'NONE',  ( 181.0000000000000000, -256.4999999999999432, -349.9999999999999432 ) ) ;
#50549 = FACE_OUTER_BOUND ( 'NONE', #3085, .T. ) ;
#50550 =( BOUNDED_CURVE ( )  B_SPLINE_CURVE ( 3, ( #12211, #423, #36345, #24284 ),
 .UNSPECIFIED., .F., .F. ) 
 B_SPLINE_CURVE_WITH_KNOTS ( ( 4, 4 ),
 ( 4.712388980384689674, 6.283185307179586232 ),
 .UNSPECIFIED. ) 
 CURVE ( )  GEOMETRIC_REPRESENTATION_ITEM ( )  RATIONAL_B_SPLINE_CURVE ( ( 1.000000000000000000, 0.8047378541243649375, 0.8047378541243649375, 1.000000000000000000 ) ) 
 REPRESENTATION_ITEM ( '' )  );
#50551 = EDGE_CURVE ( 'NONE', #50112, #29800, #26401, .T. ) ;
#50552 = CARTESIAN_POINT ( 'NONE',  ( 210.0000000000000568, 0.000000000000000000, -79.18171244307201562 ) ) ;
#50553 = ADVANCED_FACE ( 'NONE', ( #18693 ), #48605, .T. ) ;
#50554 = ORIENTED_EDGE ( 'NONE', *, *, #6400, .T. ) ;
#50555 = EDGE_CURVE ( 'NONE', #15793, #29971, #13214, .T. ) ;
#50556 = EDGE_CURVE ( 'NONE', #23256, #45635, #30743, .T. ) ;
#50557 = CARTESIAN_POINT ( 'NONE',  ( -207.2473046169136808, 2.688010569040066411, 23.74256005001722158 ) ) ;
#50558 = LINE ( 'NONE', #30608, #41790 ) ;
#50559 = VERTEX_POINT ( 'NONE', #25036 ) ;
#50560 = LINE ( 'NONE', #12361, #4987 ) ;
#50561 = DIRECTION ( 'NONE',  ( 0.000000000000000000, -0.3846153846153844702, 0.9230769230769231282 ) ) ;
#50562 = UNCERTAINTY_MEASURE_WITH_UNIT (LENGTH_MEASURE( 1.000000000000000082E-05 ), #5960, 'distance_accuracy_value', 'NONE');
#50563 = CARTESIAN_POINT ( 'NONE',  ( -166.6959734468149463, 0.000000000000000000, 165.0000000000000000 ) ) ;
#50564 = ADVANCED_FACE ( 'NONE', ( #27677, #24092 ), #17573, .T. ) ;
#50565 = ORIENTED_EDGE ( 'NONE', *, *, #14634, .T. ) ;
#50566 = ORIENTED_EDGE ( 'NONE', *, *, #45961, .T. ) ;
#50567 = PLANE ( 'NONE',  #36626 ) ;
#50568 = CARTESIAN_POINT ( 'NONE',  ( 1.588963213309524152E-14, -0.4183134307191408996, 9.992713367193013951 ) ) ;
#50569 = ORIENTED_EDGE ( 'NONE', *, *, #26775, .F. ) ;
#50570 = VERTEX_POINT ( 'NONE', #13468 ) ;
#50571 = DIRECTION ( 'NONE',  ( 1.000000000000000000, 0.000000000000000000, 0.000000000000000000 ) ) ;
#50572 = DIRECTION ( 'NONE',  ( 0.000000000000000000, 1.000000000000000000, 0.000000000000000000 ) ) ;
#50573 = FACE_OUTER_BOUND ( 'NONE', #42659, .T. ) ;
#50574 = ORIENTED_EDGE ( 'NONE', *, *, #8334, .F. ) ;
#50575 = CARTESIAN_POINT ( 'NONE',  ( 164.9999999999999716, 6.000000000000060396, -340.0000000000001137 ) ) ;
#50576 = ORIENTED_EDGE ( 'NONE', *, *, #21728, .T. ) ;
#50577 = CARTESIAN_POINT ( 'NONE',  ( -6.880036658038867436, 222.4999999999999716, -228.6347188485896140 ) ) ;
#50578 = EDGE_CURVE ( 'NONE', #34748, #2812, #29395, .T. ) ;
#50579 = CARTESIAN_POINT ( 'NONE',  ( 344.0000000000000000, 167.0000000000000000, -342.0000000000001137 ) ) ;
#50580 = CARTESIAN_POINT ( 'NONE',  ( -2.538055338523177440, -50.00000000000000711, -9.367992836599954742 ) ) ;
#50581 = EDGE_CURVE ( 'NONE', #19633, #50336, #40925, .T. ) ;
#50582 = EDGE_LOOP ( 'NONE', ( #3424, #19382, #21924, #41023 ) ) ;
#50583 = CIRCLE ( 'NONE', #39190, 2.000000000000001776 ) ;
#50584 = EDGE_CURVE ( 'NONE', #23383, #23653, #48826, .T. ) ;
#50585 = VERTEX_POINT ( 'NONE', #1680 ) ;
#50586 = ORIENTED_EDGE ( 'NONE', *, *, #13768, .T. ) ;
#50587 = DIRECTION ( 'NONE',  ( 0.000000000000000000, -0.7071067811865475727, 0.7071067811865474617 ) ) ;
#50589 = EDGE_CURVE ( 'NONE', #15045, #29675, #40683, .T. ) ;
#50588 = CARTESIAN_POINT ( 'NONE',  ( -124.9459734468149463, 2.143131898507847836E-16, 159.0682875569279702 ) ) ;
#50590 = CARTESIAN_POINT ( 'NONE',  ( 0.1083376082445593747, 1.382287789010189449, 9.960027343378010656 ) ) ;
#50591 = ORIENTED_EDGE ( 'NONE', *, *, #23993, .T. ) ;
#50592 = CARTESIAN_POINT ( 'NONE',  ( -64.99999999999815259, 17.00000000000000000, 90.00000000000000000 ) ) ;
#50593 = ORIENTED_EDGE ( 'NONE', *, *, #41613, .T. ) ;
#50594 = ADVANCED_FACE ( 'NONE', ( #39492 ), #12272, .F. ) ;
#50595 = DIRECTION ( 'NONE',  ( 0.000000000000000000, 0.000000000000000000, -1.000000000000000000 ) ) ;
#50596 = ORIENTED_EDGE ( 'NONE', *, *, #21596, .F. ) ;
#50597 =( LENGTH_UNIT ( ) NAMED_UNIT ( * ) SI_UNIT ( .MILLI., .METRE. ) );
#50598 = DIRECTION ( 'NONE',  ( 0.000000000000000000, 1.000000000000000000, -8.021842663476564905E-17 ) ) ;
#50599 = CARTESIAN_POINT ( 'NONE',  ( 12.78770032058947237, 31.68259716188277864, 7.455576670931136185 ) ) ;
#50600 = CARTESIAN_POINT ( 'NONE',  ( 35.05402655318504657, -1.025126265847089435, 162.5682875569279133 ) ) ;
#50601 = CARTESIAN_POINT ( 'NONE',  ( -206.6959734468149463, -1.750000000000010214, -39.18171244307202983 ) ) ;
#50602 = EDGE_LOOP ( 'NONE', ( #27781, #42005, #228, #42675, #40012, #1219 ) ) ;
#50603 = ORIENTED_EDGE ( 'NONE', *, *, #22443, .F. ) ;
#50604 = CARTESIAN_POINT ( 'NONE',  ( 0.000000000000000000, 17.00000000000000000, 0.000000000000000000 ) ) ;
#50605 = CARTESIAN_POINT ( 'NONE',  ( -84.94597344681494633, 2.143131898507880377E-16, -80.93171244307201562 ) ) ;
#50606 = B_SPLINE_SURFACE_WITH_KNOTS ( 'NONE', 3, 3, ( 
 ( #1963, #34031, #49369, #10416 ),
 ( #14000, #10162, #25820, #25311 ),
 ( #6321, #45536, #6818, #26066 ),
 ( #2709, #37140, #40966, #49614 ) ),
 .UNSPECIFIED., .F., .F., .F.,
 ( 4, 4 ),
 ( 4, 4 ),
 ( 0.000000000000000000, 1.000000000000000000 ),
 ( 0.000000000000000000, 1.000000000000000000 ),
 .UNSPECIFIED. ) ;
#50607 = DIRECTION ( 'NONE',  ( -1.000000000000000000, 0.000000000000000000, 1.132880637372608740E-16 ) ) ;
#50608 = PLANE ( 'NONE',  #28339 ) ;
#50609 = EDGE_CURVE ( 'NONE', #9207, #35315, #17319, .T. ) ;
#50610 = CARTESIAN_POINT ( 'NONE',  ( -69.99999999999816680, 16.00000000000000000, 90.00000000000000000 ) ) ;
#50611 = EDGE_CURVE ( 'NONE', #48152, #39727, #19197, .T. ) ;
#50612 = CARTESIAN_POINT ( 'NONE',  ( -15.00099850811941948, -7.462898891544107016, 9.403735324607438884 ) ) ;
#50613 = ORIENTED_EDGE ( 'NONE', *, *, #17459, .F. ) ;
#50614 = CARTESIAN_POINT ( 'NONE',  ( 0.000000000000000000, 23.48684210526316107, 0.000000000000000000 ) ) ;
#50615 = CARTESIAN_POINT ( 'NONE',  ( -164.9459734468149463, 1.025126265847089435, -157.4317124430720582 ) ) ;
#50616 = ORIENTED_EDGE ( 'NONE', *, *, #25529, .F. ) ;
#50617 = EDGE_CURVE ( 'NONE', #17359, #29784, #28914, .T. ) ;
#50618 = ADVANCED_FACE ( 'NONE', ( #43570, #13719 ), #6291, .T. ) ;
#50619 = CARTESIAN_POINT ( 'NONE',  ( 33.16902712922644270, -37.70469005304286725, 1.847720168420772691 ) ) ;
#50620 = DIRECTION ( 'NONE',  ( 0.000000000000000000, 1.000000000000000000, 0.000000000000000000 ) ) ;
#50621 = EDGE_CURVE ( 'NONE', #40762, #9299, #5422, .T. ) ;
#50622 = PLANE ( 'NONE',  #40569 ) ;
#50623 = ADVANCED_FACE ( 'NONE', ( #13965 ), #25782, .T. ) ;
#50624 = ORIENTED_EDGE ( 'NONE', *, *, #6971, .F. ) ;
#50625 = ORIENTED_EDGE ( 'NONE', *, *, #45180, .F. ) ;
#50626 = CARTESIAN_POINT ( 'NONE',  ( 167.5000000000000000, 102.5000000000000142, -8.474599139414886295 ) ) ;
#50627 = EDGE_CURVE ( 'NONE', #31049, #40007, #20863, .T. ) ;
#50628 = CARTESIAN_POINT ( 'NONE',  ( 168.9999999999999716, -79.49999999999997158, -340.0000000000001137 ) ) ;
#50629 = EDGE_LOOP ( 'NONE', ( #17610, #31451, #48726, #20915, #32135, #25249 ) ) ;
#50630 = ORIENTED_EDGE ( 'NONE', *, *, #29279, .T. ) ;
#50631 = LINE ( 'NONE', #46283, #4305 ) ;
#50632 = CARTESIAN_POINT ( 'NONE',  ( 1.250000000000000222, 0.000000000000000000, 10.00000000000000000 ) ) ;
#50633 = CARTESIAN_POINT ( 'NONE',  ( 111.5540265531850537, -1.025126265847081886, 39.06828755692799149 ) ) ;
#50634 =( BOUNDED_CURVE ( )  B_SPLINE_CURVE ( 3, ( #35399, #46875, #34885, #46114 ),
 .UNSPECIFIED., .F., .F. ) 
 B_SPLINE_CURVE_WITH_KNOTS ( ( 4, 4 ),
 ( 1.570796326794896558, 3.141592653589793116 ),
 .UNSPECIFIED. ) 
 CURVE ( )  GEOMETRIC_REPRESENTATION_ITEM ( )  RATIONAL_B_SPLINE_CURVE ( ( 1.000000000000000000, 0.8047378541243649375, 0.8047378541243649375, 1.000000000000000000 ) ) 
 REPRESENTATION_ITEM ( '' )  );
#50635 = VERTEX_POINT ( 'NONE', #2429 ) ;
#50636 = ORIENTED_EDGE ( 'NONE', *, *, #26808, .F. ) ;
#50637 = EDGE_LOOP ( 'NONE', ( #32099, #16535, #18977, #26767 ) ) ;
#50638 = CARTESIAN_POINT ( 'NONE',  ( -33.43156050989129824, 4.370686678976795747, 8.807470649214879543 ) ) ;
#50639 = CARTESIAN_POINT ( 'NONE',  ( -40.00000000000000000, -7.564790863224938100, 897.6604670114604687 ) ) ;
#50640 = ORIENTED_EDGE ( 'NONE', *, *, #40435, .T. ) ;
#50641 = CARTESIAN_POINT ( 'NONE',  ( 6.174150299305392053, -50.00000000000000711, 8.807470649214879543 ) ) ;
#50642 = EDGE_CURVE ( 'NONE', #4741, #38121, #32425, .T. ) ;
#50643 = CARTESIAN_POINT ( 'NONE',  ( 0.9162543521529814550, -1.312131394983855781, 9.919954280166519922 ) ) ;
#50644 = DIRECTION ( 'NONE',  ( 1.000000000000000000, 0.000000000000000000, 0.000000000000000000 ) ) ;
#50645 = ORIENTED_EDGE ( 'NONE', *, *, #43491, .T. ) ;
#50646 = EDGE_LOOP ( 'NONE', ( #665, #43487, #27390, #14001 ) ) ;
#50647 = CYLINDRICAL_SURFACE ( 'NONE', #37723, 1.750000000000008438 ) ;
#50648 = CARTESIAN_POINT ( 'NONE',  ( 1.902011274814930042, 1.028513261185797223, 9.882709995651167034 ) ) ;
#50649 = CARTESIAN_POINT ( 'NONE',  ( 111.5540265531850537, -1.025126265847081442, -0.9317124430720195027 ) ) ;
#50650 = UNCERTAINTY_MEASURE_WITH_UNIT (LENGTH_MEASURE( 1.000000000000000082E-05 ), #27696, 'distance_accuracy_value', 'NONE');
#50651 = EDGE_LOOP ( 'NONE', ( #8422, #10148, #2041, #48933 ) ) ;
#50652 = ORIENTED_EDGE ( 'NONE', *, *, #29760, .T. ) ;
#50653 = CARTESIAN_POINT ( 'NONE',  ( -0.3862712429686977478, 1.188820645368937390, 3.333333333333333481 ) ) ;
#50654 = DIRECTION ( 'NONE',  ( -3.172065784643302499E-16, -1.000000000000000000, 2.537652627714642000E-15 ) ) ;
#50656 = VERTEX_POINT ( 'NONE', #14214 ) ;
#50655 = VECTOR ( 'NONE', #37104, 1000.000000000000000 ) ;
#50657 = CARTESIAN_POINT ( 'NONE',  ( 114.3291528190321173, 1.749999999999996669, 39.79316129108089228 ) ) ;
#50658 = LINE ( 'NONE', #11707, #39996 ) ;
#50659 = CARTESIAN_POINT ( 'NONE',  ( 5.505322767148756569, -37.09368438467003415, 8.914903342594564961 ) ) ;
#50660 = VECTOR ( 'NONE', #7443, 1000.000000000000000 ) ;
#50661 = CARTESIAN_POINT ( 'NONE',  ( 1.011271242968677653, 0.7347315653656002477, 10.00000000000000000 ) ) ;
#50662 = VERTEX_POINT ( 'NONE', #33745 ) ;
#50663 = ADVANCED_FACE ( 'NONE', ( #29879 ), #38100, .F. ) ;
#50664 = CARTESIAN_POINT ( 'NONE',  ( 30.00000000000062172, 17.00000000000000000, -30.00000000000000000 ) ) ;
#50665 = CARTESIAN_POINT ( 'NONE',  ( -128.4459734468149179, 0.000000000000000000, 79.06828755692799859 ) ) ;
#50666 = DIRECTION ( 'NONE',  ( 0.000000000000000000, 0.000000000000000000, -1.000000000000000000 ) ) ;
#50667 = CLOSED_SHELL ( 'NONE', ( #12857, #48730, #33141, #49280, #18247, #1447, #20300, #17064, #28644, #25948, #30151, #23822, #42852, #18263, #48042, #20630, #2548, #14861 ) ) ;
#50668 = VECTOR ( 'NONE', #4676, 999.9999999999998863 ) ;
#50669 = VERTEX_POINT ( 'NONE', #10882 ) ;
#50670 = CYLINDRICAL_SURFACE ( 'NONE', #4828, 0.4999999999999992228 ) ;
#50671 = CARTESIAN_POINT ( 'NONE',  ( 1.142975459103954705, 16.61830776097024653, -2.870787844569587133 ) ) ;
#50672 = CARTESIAN_POINT ( 'NONE',  ( 0.000000000000000000, 0.000000000000000000, 0.000000000000000000 ) ) ;
#50673 = ORIENTED_EDGE ( 'NONE', *, *, #48359, .T. ) ;
#50674 = DIRECTION ( 'NONE',  ( 0.000000000000000000, 4.687818848539279227E-49, -1.000000000000000000 ) ) ;
#50675 = EDGE_CURVE ( 'NONE', #34186, #28480, #29625, .T. ) ;
#50676 = ADVANCED_FACE ( 'NONE', ( #45995, #41678 ), #33492, .T. ) ;
#50677 = DIRECTION ( 'NONE',  ( -0.000000000000000000, -0.9749645535258953943, 0.2223603367690637489 ) ) ;
#50678 = ORIENTED_EDGE ( 'NONE', *, *, #22742, .F. ) ;
#50679 = DIRECTION ( 'NONE',  ( 0.000000000000000000, 0.000000000000000000, -1.000000000000000000 ) ) ;
#50680 = FACE_OUTER_BOUND ( 'NONE', #9726, .T. ) ;
#50681 = DIRECTION ( 'NONE',  ( 0.000000000000000000, 0.000000000000000000, -1.000000000000000000 ) ) ;
#50682 = CARTESIAN_POINT ( 'NONE',  ( -86.69597344681494633, 1.750000000000010214, 40.81828755692798438 ) ) ;
#50683 = EDGE_CURVE ( 'NONE', #13485, #11294, #29696, .T. ) ;
#50684 = ORIENTED_EDGE ( 'NONE', *, *, #4698, .T. ) ;
#50685 = CYLINDRICAL_SURFACE ( 'NONE', #29820, 1.750000000000015543 ) ;
#50686 = ORIENTED_EDGE ( 'NONE', *, *, #24357, .T. ) ;
#50687 = ORIENTED_EDGE ( 'NONE', *, *, #39108, .T. ) ;
#50688 = B_SPLINE_CURVE_WITH_KNOTS ( 'NONE', 3,
 ( #43876, #48689, #44116, #5886 ),
 .UNSPECIFIED., .F., .F.,
 ( 4, 4 ),
 ( 0.9811748202683100439, 0.9878904167554125593 ),
 .UNSPECIFIED. ) ;
#50689 = LINE ( 'NONE', #27394, #2910 ) ;
#50690 = ADVANCED_FACE ( 'NONE', ( #2914 ), #22037, .T. ) ;
#50691 = CARTESIAN_POINT ( 'NONE',  ( 193.3040265531851105, -1.750000000000010658, 120.8182875569279702 ) ) ;
#50692 = ADVANCED_FACE ( 'NONE', ( #50078 ), #14989, .F. ) ;
#50693 =( BOUNDED_CURVE ( )  B_SPLINE_CURVE ( 3, ( #32379, #24936, #40082, #32634 ),
 .UNSPECIFIED., .F., .F. ) 
 B_SPLINE_CURVE_WITH_KNOTS ( ( 4, 4 ),
 ( 4.712388980384689674, 6.283185307179586232 ),
 .UNSPECIFIED. ) 
 CURVE ( )  GEOMETRIC_REPRESENTATION_ITEM ( )  RATIONAL_B_SPLINE_CURVE ( ( 1.000000000000000000, 0.8047378541243649375, 0.8047378541243649375, 1.000000000000000000 ) ) 
 REPRESENTATION_ITEM ( '' )  );
#50694 = VECTOR ( 'NONE', #46012, 1000.000000000000000 ) ;
#50695 = ORIENTED_EDGE ( 'NONE', *, *, #40930, .F. ) ;
#50696 = PLANE ( 'NONE',  #25427 ) ;
#50697 = CARTESIAN_POINT ( 'NONE',  ( -36.97942854200451990, 6.226705766838657397, 8.914903342594564961 ) ) ;
#50698 = VECTOR ( 'NONE', #21527, 1000.000000000000000 ) ;
#50699 = VECTOR ( 'NONE', #13032, 1000.000000000000000 ) ;
#50700 =( BOUNDED_CURVE ( )  B_SPLINE_CURVE ( 3, ( #15797, #22479, #19644, #47053 ),
 .UNSPECIFIED., .F., .F. ) 
 B_SPLINE_CURVE_WITH_KNOTS ( ( 4, 4 ),
 ( 1.570796326794903441, 3.141592653589515560 ),
 .UNSPECIFIED. ) 
 CURVE ( )  GEOMETRIC_REPRESENTATION_ITEM ( )  RATIONAL_B_SPLINE_CURVE ( ( 1.000000000000000000, 0.8047378541244319949, 0.8047378541244319949, 1.000000000000000000 ) ) 
 REPRESENTATION_ITEM ( '' )  );
#50701 = EDGE_CURVE ( 'NONE', #33352, #23671, #19841, .T. ) ;
#50702 = LINE ( 'NONE', #15090, #31708 ) ;
#50703 = ORIENTED_EDGE ( 'NONE', *, *, #30990, .F. ) ;
#50704 = CARTESIAN_POINT ( 'NONE',  ( -204.9459734468149463, 2.143131898507880377E-16, 119.0682875569279702 ) ) ;
#50705 = CARTESIAN_POINT ( 'NONE',  ( -34.91952936320829792, 13.67027684621028349, -9.422646554964178023 ) ) ;
#50706 =( NAMED_UNIT ( * ) PLANE_ANGLE_UNIT ( ) SI_UNIT ( $, .RADIAN. ) );
#50707 = VECTOR ( 'NONE', #43276, 1000.000000000000000 ) ;
#50708 = EDGE_LOOP ( 'NONE', ( #46579, #24388, #19744, #22246 ) ) ;
#50709 = CARTESIAN_POINT ( 'NONE',  ( 12.97493236725083676, -11.05939663306990717, 8.953103998512858652 ) ) ;
#50710 = DIRECTION ( 'NONE',  ( 1.000000000000000000, -4.758098676964956461E-16, -8.975803739141899931E-48 ) ) ;
#50711 = ORIENTED_EDGE ( 'NONE', *, *, #34369, .T. ) ;
#50712 = ORIENTED_EDGE ( 'NONE', *, *, #21249, .T. ) ;
#50713 = ORIENTED_EDGE ( 'NONE', *, *, #14623, .F. ) ;
#50714 = DIRECTION ( 'NONE',  ( -1.000000000000000000, -0.000000000000000000, -0.000000000000000000 ) ) ;
#50715 =( BOUNDED_CURVE ( )  B_SPLINE_CURVE ( 3, ( #26047, #22438, #2927, #18082 ),
 .UNSPECIFIED., .F., .F. ) 
 B_SPLINE_CURVE_WITH_KNOTS ( ( 4, 4 ),
 ( 3.141592653589793116, 4.712388980384689674 ),
 .UNSPECIFIED. ) 
 CURVE ( )  GEOMETRIC_REPRESENTATION_ITEM ( )  RATIONAL_B_SPLINE_CURVE ( ( 1.000000000000000000, 0.8047378541243649375, 0.8047378541243649375, 1.000000000000000000 ) ) 
 REPRESENTATION_ITEM ( '' )  );
#50716 = CARTESIAN_POINT ( 'NONE',  ( 0.000000000000000000, 47.50000000000000000, 0.000000000000000000 ) ) ;
#50717 = PRODUCT_DEFINITION_SHAPE ( 'NONE', 'NONE',  #50723 ) ;
#50718 = VERTEX_POINT ( 'NONE', #43445 ) ;
#50719 = DIRECTION ( 'NONE',  ( -0.000000000000000000, -0.000000000000000000, -1.000000000000000000 ) ) ;
#50720 = CARTESIAN_POINT ( 'NONE',  ( -14.49999999999999822, -46.01315789473684248, -5.916985404131817283 ) ) ;
#50721 = DIRECTION ( 'NONE',  ( -1.000000000000000000, 0.000000000000000000, 0.000000000000000000 ) ) ;
#50722 = CARTESIAN_POINT ( 'NONE',  ( 344.0000000000000000, 183.0000000000000284, 357.9999999999998863 ) ) ;
#50723 = NEXT_ASSEMBLY_USAGE_OCCURRENCE ( 'NAUO1', ' ', ' ', #25918, #6792, $ ) ;
#50724 = NEXT_ASSEMBLY_USAGE_OCCURRENCE ( 'NAUO2', ' ', ' ', #25918, #13035, $ ) ;
#50725 = NEXT_ASSEMBLY_USAGE_OCCURRENCE ( 'NAUO3', ' ', ' ', #25918, #8372, $ ) ;
#50726 = NEXT_ASSEMBLY_USAGE_OCCURRENCE ( 'NAUO4', ' ', ' ', #25918, #48451, $ ) ;
#50727 = NEXT_ASSEMBLY_USAGE_OCCURRENCE ( 'NAUO5', ' ', ' ', #25918, #29665, $ ) ;
#50728 = NEXT_ASSEMBLY_USAGE_OCCURRENCE ( 'NAUO6', ' ', ' ', #25918, #8372, $ ) ;
#50729 = NEXT_ASSEMBLY_USAGE_OCCURRENCE ( 'NAUO7', ' ', ' ', #25918, #8372, $ ) ;
#50730 = NEXT_ASSEMBLY_USAGE_OCCURRENCE ( 'NAUO8', ' ', ' ', #25918, #8372, $ ) ;
#50731 = NEXT_ASSEMBLY_USAGE_OCCURRENCE ( 'NAUO9', ' ', ' ', #25918, #17451, $ ) ;
#50732 = NEXT_ASSEMBLY_USAGE_OCCURRENCE ( 'NAUO10', ' ', ' ', #25918, #38783, $ ) ;
#50733 = NEXT_ASSEMBLY_USAGE_OCCURRENCE ( 'NAUO11', ' ', ' ', #25918, #38783, $ ) ;
#50734 = NEXT_ASSEMBLY_USAGE_OCCURRENCE ( 'NAUO12', ' ', ' ', #25918, #38783, $ ) ;
#50735 = NEXT_ASSEMBLY_USAGE_OCCURRENCE ( 'NAUO13', ' ', ' ', #25918, #26547, $ ) ;
#50736 = NEXT_ASSEMBLY_USAGE_OCCURRENCE ( 'NAUO14', ' ', ' ', #25918, #47817, $ ) ;
#50737 = NEXT_ASSEMBLY_USAGE_OCCURRENCE ( 'NAUO15', ' ', ' ', #25918, #44709, $ ) ;
#50738 = NEXT_ASSEMBLY_USAGE_OCCURRENCE ( 'NAUO16', ' ', ' ', #25918, #842, $ ) ;
#50739 = NEXT_ASSEMBLY_USAGE_OCCURRENCE ( 'NAUO17', ' ', ' ', #8372, #48451, $ ) ;
#50740 = NEXT_ASSEMBLY_USAGE_OCCURRENCE ( 'NAUO18', ' ', ' ', #8372, #29665, $ ) ;
#50741=COLOUR_RGB('Dark Blue',0.08,0.2,0.34);
#50742=FILL_AREA_STYLE_COLOUR('',#50741);
#50743=FILL_AREA_STYLE('',(#50742));
#50744=SURFACE_STYLE_FILL_AREA(#50743);
#50745=SURFACE_SIDE_STYLE('',(#50744));
#50746=SURFACE_STYLE_USAGE(.BOTH.,#50745);
#50747=PRESENTATION_STYLE_ASSIGNMENT((#50746));
#50748=COLOUR_RGB('Light Blue',0.38,0.62,0.78);
#50749=FILL_AREA_STYLE_COLOUR('',#50748);
#50750=FILL_AREA_STYLE('',(#50749));
#50751=SURFACE_STYLE_FILL_AREA(#50750);
#50752=SURFACE_SIDE_STYLE('',(#50751));
#50753=SURFACE_STYLE_USAGE(.BOTH.,#50752);
#50754=PRESENTATION_STYLE_ASSIGNMENT((#50753));
#50755=COLOUR_RGB('Sky Blue',0.24,0.69,0.87);
#50756=FILL_AREA_STYLE_COLOUR('',#50755);
#50757=FILL_AREA_STYLE('',(#50756));
#50758=SURFACE_STYLE_FILL_AREA(#50757);
#50759=SURFACE_SIDE_STYLE('',(#50758));
#50760=SURFACE_STYLE_USAGE(.BOTH.,#50759);
#50761=PRESENTATION_STYLE_ASSIGNMENT((#50760));
#50762=COLOUR_RGB('Grey',0.48,0.52,0.57);
#50763=FILL_AREA_STYLE_COLOUR('',#50762);
#50764=FILL_AREA_STYLE('',(#50763));
#50765=SURFACE_STYLE_FILL_AREA(#50764);
#50766=SURFACE_SIDE_STYLE('',(#50765));
#50767=SURFACE_STYLE_USAGE(.BOTH.,#50766);
#50768=PRESENTATION_STYLE_ASSIGNMENT((#50767));
#50769=COLOUR_RGB('Black',0.12,0.14,0.17);
#50770=FILL_AREA_STYLE_COLOUR('',#50769);
#50771=FILL_AREA_STYLE('',(#50770));
#50772=SURFACE_STYLE_FILL_AREA(#50771);
#50773=SURFACE_SIDE_STYLE('',(#50772));
#50774=SURFACE_STYLE_USAGE(.BOTH.,#50773);
#50775=PRESENTATION_STYLE_ASSIGNMENT((#50774));
#50776=COLOUR_RGB('Off White',0.89,0.88,0.83);
#50777=FILL_AREA_STYLE_COLOUR('',#50776);
#50778=FILL_AREA_STYLE('',(#50777));
#50779=SURFACE_STYLE_FILL_AREA(#50778);
#50780=SURFACE_SIDE_STYLE('',(#50779));
#50781=SURFACE_STYLE_USAGE(.BOTH.,#50780);
#50782=PRESENTATION_STYLE_ASSIGNMENT((#50781));
ENDSEC;
END-ISO-10303-21;
